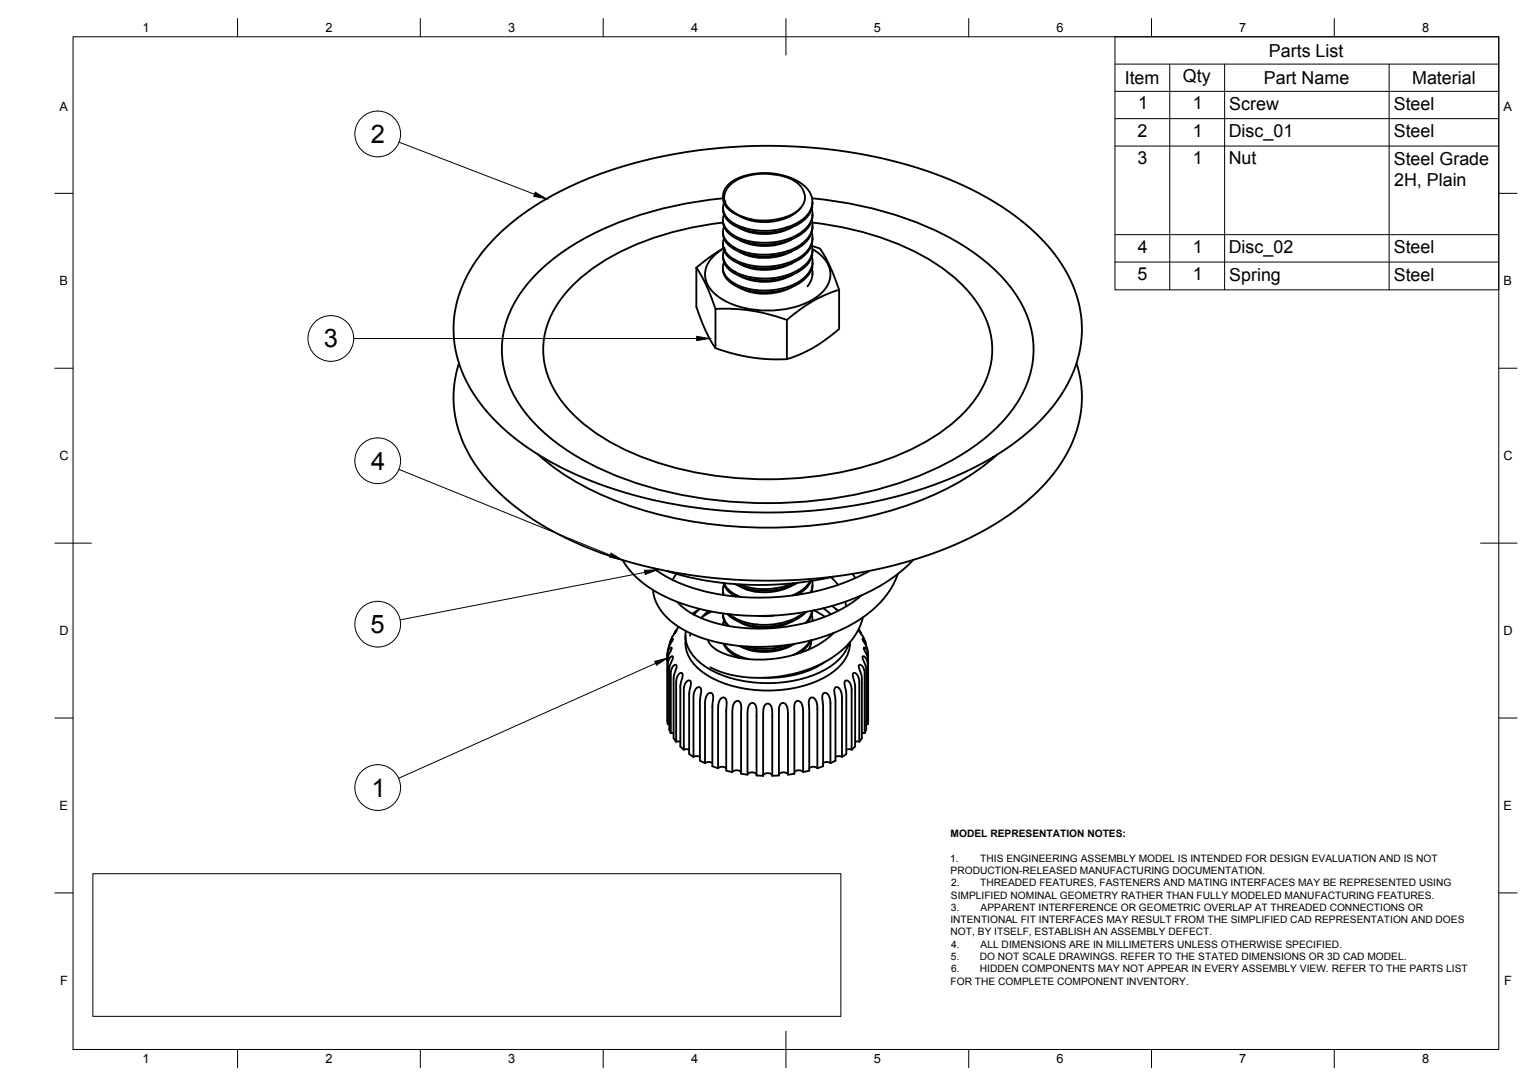
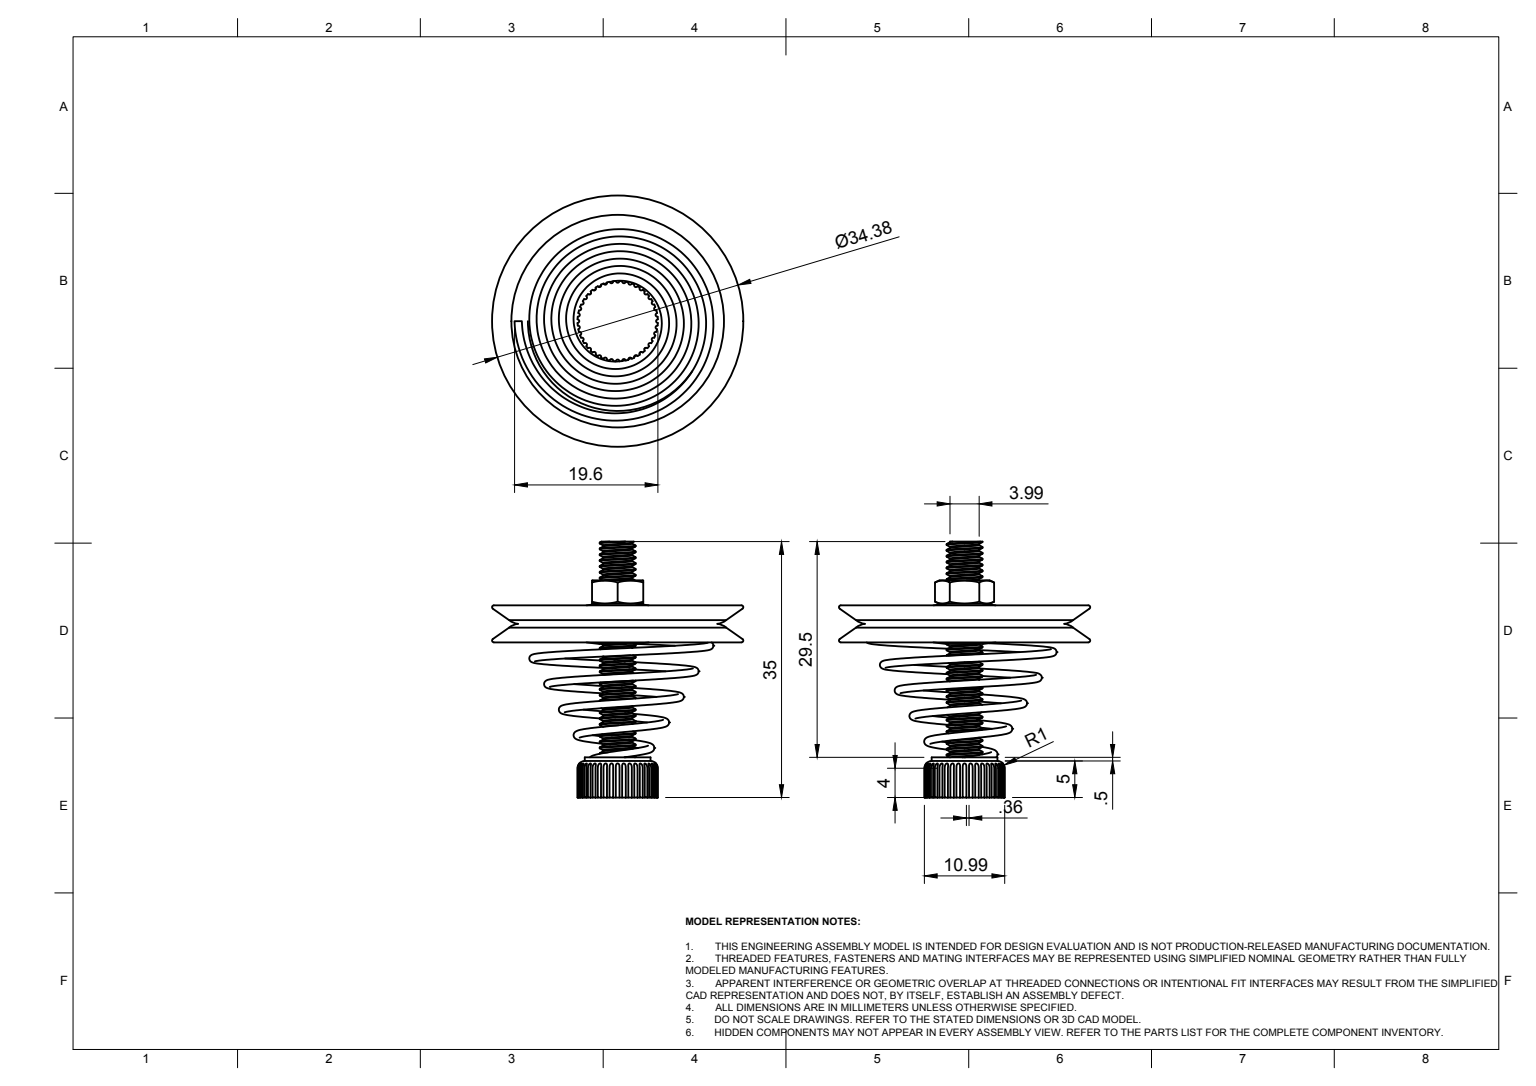
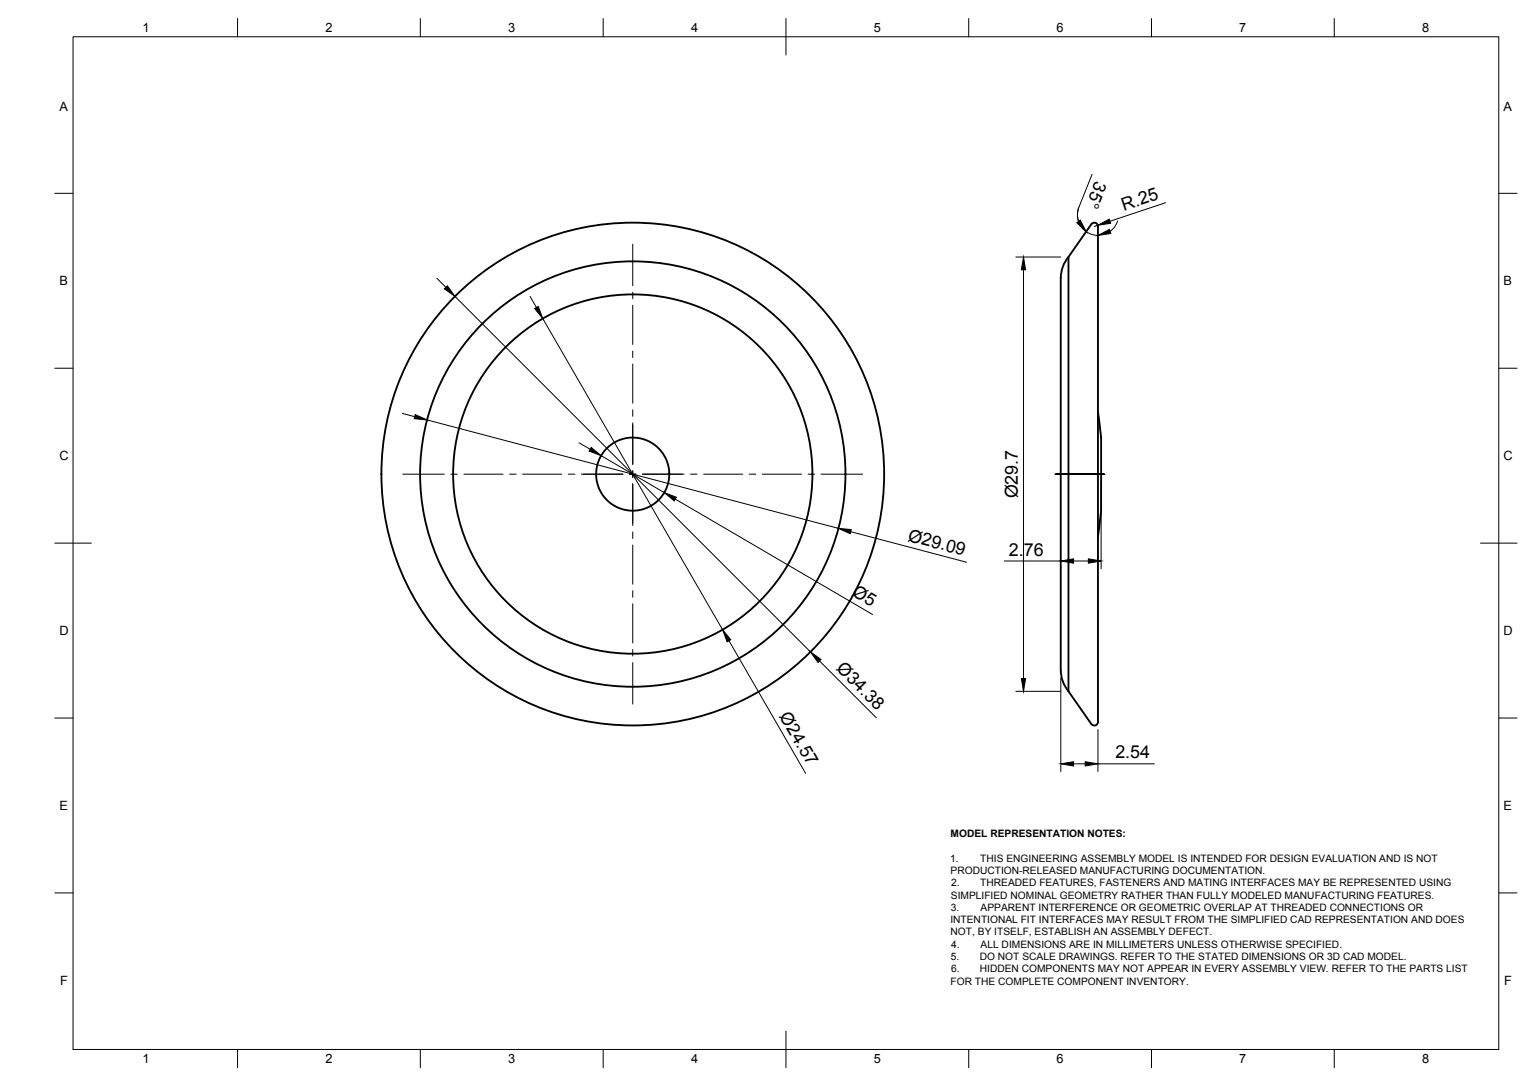
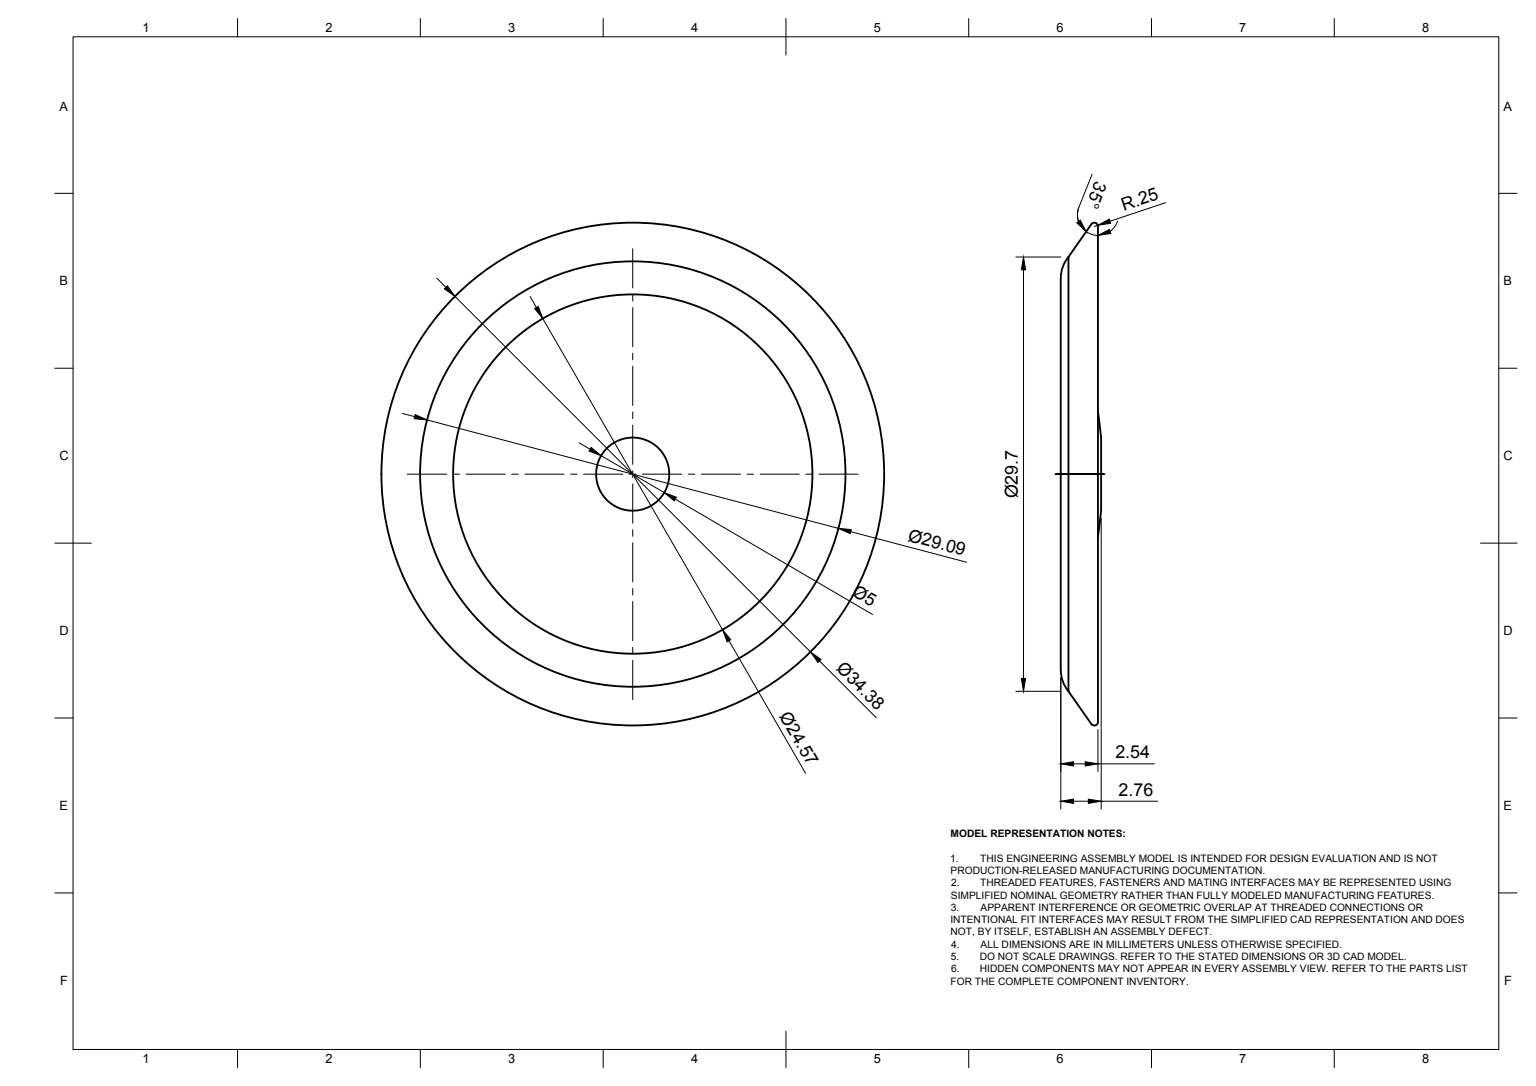
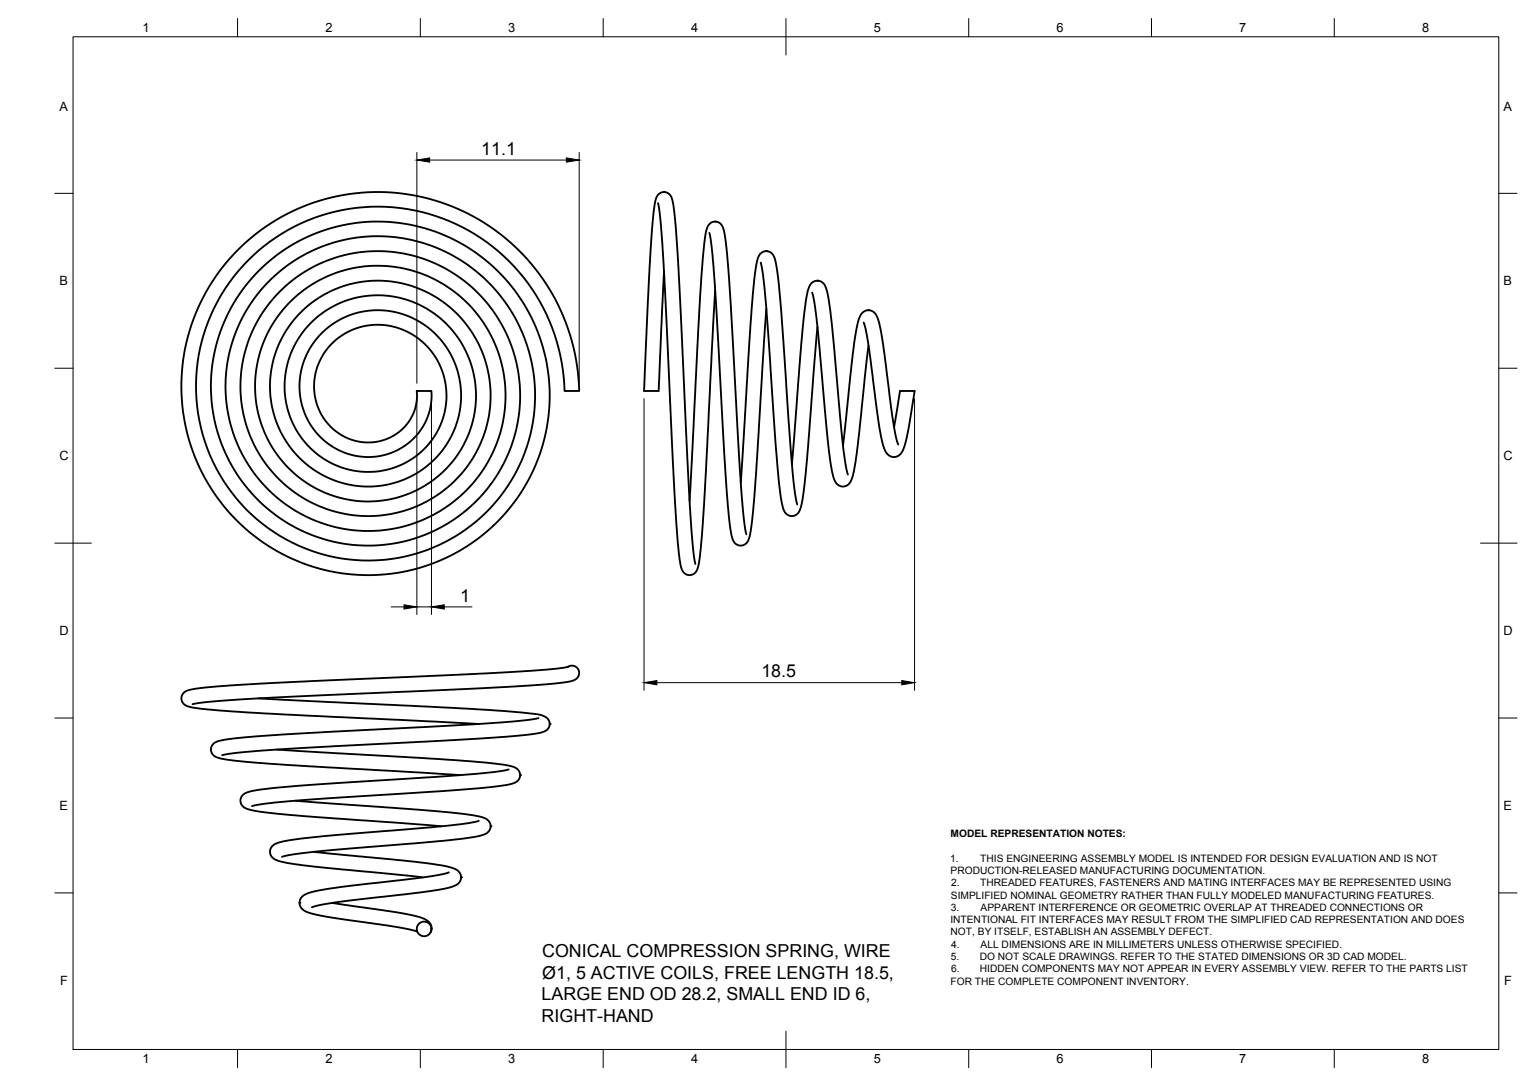
ISO-10303-21;
HEADER;
/* Generated by software containing ST-Developer
 * from STEP Tools, Inc. (www.steptools.com) 
 */

FILE_DESCRIPTION(
/* description */ (''),
/* implementation_level */ '2;1');

FILE_NAME(
/* name */ 'BR-106',
/* time_stamp */ '2026-10-04T16:36:43-07:00',
/* author */ (''),
/* organization */ (''),
/* preprocessor_version */ 'ST-DEVELOPER v20.2',
/* originating_system */ 'Autodesk Translation Framework v15.15.0.0',
/* authorisation */ '');

FILE_SCHEMA (('AUTOMOTIVE_DESIGN { 1 0 10303 214 3 1 1 }'));
ENDSEC;

DATA;
#10=MECHANICAL_DESIGN_GEOMETRIC_PRESENTATION_REPRESENTATION('',(#67,#68,
#69,#70,#71),#33474);
#11=ITEM_DEFINED_TRANSFORMATION($,$,#2869,#3144);
#12=ITEM_DEFINED_TRANSFORMATION($,$,#3089,#3145);
#13=ITEM_DEFINED_TRANSFORMATION($,$,#3107,#3146);
#14=ITEM_DEFINED_TRANSFORMATION($,$,#3125,#3147);
#15=ITEM_DEFINED_TRANSFORMATION($,$,#3128,#3148);
#16=(
REPRESENTATION_RELATIONSHIP($,$,#33497,#33496)
REPRESENTATION_RELATIONSHIP_WITH_TRANSFORMATION(#11)
SHAPE_REPRESENTATION_RELATIONSHIP()
);
#17=(
REPRESENTATION_RELATIONSHIP($,$,#33498,#33496)
REPRESENTATION_RELATIONSHIP_WITH_TRANSFORMATION(#12)
SHAPE_REPRESENTATION_RELATIONSHIP()
);
#18=(
REPRESENTATION_RELATIONSHIP($,$,#33499,#33496)
REPRESENTATION_RELATIONSHIP_WITH_TRANSFORMATION(#13)
SHAPE_REPRESENTATION_RELATIONSHIP()
);
#19=(
REPRESENTATION_RELATIONSHIP($,$,#33500,#33496)
REPRESENTATION_RELATIONSHIP_WITH_TRANSFORMATION(#14)
SHAPE_REPRESENTATION_RELATIONSHIP()
);
#20=(
REPRESENTATION_RELATIONSHIP($,$,#33501,#33496)
REPRESENTATION_RELATIONSHIP_WITH_TRANSFORMATION(#15)
SHAPE_REPRESENTATION_RELATIONSHIP()
);
#21=CONTEXT_DEPENDENT_SHAPE_REPRESENTATION(#16,#33491);
#22=CONTEXT_DEPENDENT_SHAPE_REPRESENTATION(#17,#33492);
#23=CONTEXT_DEPENDENT_SHAPE_REPRESENTATION(#18,#33493);
#24=CONTEXT_DEPENDENT_SHAPE_REPRESENTATION(#19,#33494);
#25=CONTEXT_DEPENDENT_SHAPE_REPRESENTATION(#20,#33495);
#26=NEXT_ASSEMBLY_USAGE_OCCURRENCE('Screw:1','Screw:1','Screw:1',#33503,
#33504,'Screw:1');
#27=NEXT_ASSEMBLY_USAGE_OCCURRENCE('Disc_01:1','Disc_01:1','Disc_01:1',
#33503,#33505,'Disc_01:1');
#28=NEXT_ASSEMBLY_USAGE_OCCURRENCE('Disc_02:1','Disc_02:1','Disc_02:1',
#33503,#33506,'Disc_02:1');
#29=NEXT_ASSEMBLY_USAGE_OCCURRENCE('Spring:1','Spring:1','Spring:1',#33503,
#33507,'Spring:1');
#30=NEXT_ASSEMBLY_USAGE_OCCURRENCE('Nut:1','Nut:1','Nut:1',#33503,#33508,
'Nut:1');
#31=(
BOUNDED_CURVE()
B_SPLINE_CURVE(5,(#31814,#31815,#31816,#31817,#31818,#31819,#31820,#31821,
#31822,#31823,#31824,#31825,#31826,#31827,#31828,#31829,#31830,#31831,#31832,
#31833,#31834,#31835,#31836,#31837,#31838),.UNSPECIFIED.,.F.,.F.)
B_SPLINE_CURVE_WITH_KNOTS((6,5,1,1,1,1,1,1,1,1,1,1,1,1,1,1,6),(-0.120132019601874,
0.,0.0666666666666667,0.133333333333333,0.2,0.266666666666667,0.333333333333333,
0.4,0.466666666666667,0.533333333333333,0.6,0.666666666666667,0.733333333333333,
0.8,0.866666666666667,0.933333333333333,1.),.UNSPECIFIED.)
CURVE()
GEOMETRIC_REPRESENTATION_ITEM()
RATIONAL_B_SPLINE_CURVE((1.,1.,1.,1.,1.,1.,1.,1.,1.,1.,1.,1.,1.,1.,1.,1.,
1.,1.,1.,1.,1.,1.,1.,1.,1.))
REPRESENTATION_ITEM('')
);
#32=(
BOUNDED_CURVE()
B_SPLINE_CURVE(5,(#32307,#32308,#32309,#32310,#32311,#32312,#32313,#32314,
#32315,#32316,#32317,#32318,#32319,#32320,#32321,#32322,#32323,#32324,#32325,
#32326,#32327,#32328,#32329,#32330,#32331),.UNSPECIFIED.,.F.,.F.)
B_SPLINE_CURVE_WITH_KNOTS((6,5,1,1,1,1,1,1,1,1,1,1,1,1,1,1,6),(-0.120132019601874,
0.,0.0666666666666667,0.133333333333333,0.2,0.266666666666667,0.333333333333333,
0.4,0.466666666666667,0.533333333333333,0.6,0.666666666666667,0.733333333333333,
0.8,0.866666666666667,0.933333333333333,1.),.UNSPECIFIED.)
CURVE()
GEOMETRIC_REPRESENTATION_ITEM()
RATIONAL_B_SPLINE_CURVE((1.,1.,1.,1.,1.,1.,1.,1.,1.,1.,1.,1.,1.,1.,1.,1.,
1.,1.,1.,1.,1.,1.,1.,1.,1.))
REPRESENTATION_ITEM('')
);
#33=(
BOUNDED_CURVE()
B_SPLINE_CURVE(2,(#33377,#33378,#33379),.UNSPECIFIED.,.F.,.F.)
B_SPLINE_CURVE_WITH_KNOTS((3,3),(0.000182870967167632,0.407532766922341),
 .UNSPECIFIED.)
CURVE()
GEOMETRIC_REPRESENTATION_ITEM()
RATIONAL_B_SPLINE_CURVE((1.00013898062186,1.15486101937814,1.00013898062186))
REPRESENTATION_ITEM('')
);
#34=(
BOUNDED_CURVE()
B_SPLINE_CURVE(2,(#33382,#33383,#33384),.UNSPECIFIED.,.F.,.F.)
B_SPLINE_CURVE_WITH_KNOTS((3,3),(0.000182870967168132,0.407532766922342),
 .UNSPECIFIED.)
CURVE()
GEOMETRIC_REPRESENTATION_ITEM()
RATIONAL_B_SPLINE_CURVE((1.00013898062186,1.15486101937814,1.00013898062186))
REPRESENTATION_ITEM('')
);
#35=(
BOUNDED_CURVE()
B_SPLINE_CURVE(2,(#33387,#33388,#33389),.UNSPECIFIED.,.F.,.F.)
B_SPLINE_CURVE_WITH_KNOTS((3,3),(0.000182870967167337,0.407532766922341),
 .UNSPECIFIED.)
CURVE()
GEOMETRIC_REPRESENTATION_ITEM()
RATIONAL_B_SPLINE_CURVE((1.00013898062186,1.15486101937814,1.00013898062186))
REPRESENTATION_ITEM('')
);
#36=(
BOUNDED_CURVE()
B_SPLINE_CURVE(2,(#33392,#33393,#33394),.UNSPECIFIED.,.F.,.F.)
B_SPLINE_CURVE_WITH_KNOTS((3,3),(0.000182870967167613,0.407532766922341),
 .UNSPECIFIED.)
CURVE()
GEOMETRIC_REPRESENTATION_ITEM()
RATIONAL_B_SPLINE_CURVE((1.00013898062186,1.15486101937814,1.00013898062186))
REPRESENTATION_ITEM('')
);
#37=(
BOUNDED_CURVE()
B_SPLINE_CURVE(2,(#33401,#33402,#33403),.UNSPECIFIED.,.F.,.F.)
B_SPLINE_CURVE_WITH_KNOTS((3,3),(0.203857818944754,0.407532766922341),
 .UNSPECIFIED.)
CURVE()
GEOMETRIC_REPRESENTATION_ITEM()
RATIONAL_B_SPLINE_CURVE((1.0775,1.0775,1.00013898062186))
REPRESENTATION_ITEM('')
);
#38=(
BOUNDED_CURVE()
B_SPLINE_CURVE(2,(#33405,#33406,#33407),.UNSPECIFIED.,.F.,.F.)
B_SPLINE_CURVE_WITH_KNOTS((3,3),(0.000182870967167808,0.407532766922341),
 .UNSPECIFIED.)
CURVE()
GEOMETRIC_REPRESENTATION_ITEM()
RATIONAL_B_SPLINE_CURVE((1.00013898062186,1.15486101937814,1.00013898062186))
REPRESENTATION_ITEM('')
);
#39=(
BOUNDED_CURVE()
B_SPLINE_CURVE(2,(#33408,#33409,#33410),.UNSPECIFIED.,.F.,.F.)
B_SPLINE_CURVE_WITH_KNOTS((3,3),(0.000182870967168059,0.407532766922341),
 .UNSPECIFIED.)
CURVE()
GEOMETRIC_REPRESENTATION_ITEM()
RATIONAL_B_SPLINE_CURVE((1.00013898062186,1.15486101937814,1.00013898062186))
REPRESENTATION_ITEM('')
);
#40=(
BOUNDED_CURVE()
B_SPLINE_CURVE(2,(#33412,#33413,#33414),.UNSPECIFIED.,.F.,.F.)
B_SPLINE_CURVE_WITH_KNOTS((3,3),(0.000182870967167986,0.407532766922341),
 .UNSPECIFIED.)
CURVE()
GEOMETRIC_REPRESENTATION_ITEM()
RATIONAL_B_SPLINE_CURVE((1.00013898062186,1.15486101937814,1.00013898062186))
REPRESENTATION_ITEM('')
);
#41=(
BOUNDED_CURVE()
B_SPLINE_CURVE(2,(#33415,#33416,#33417),.UNSPECIFIED.,.F.,.F.)
B_SPLINE_CURVE_WITH_KNOTS((3,3),(0.000182870967167794,0.203857818944754),
 .UNSPECIFIED.)
CURVE()
GEOMETRIC_REPRESENTATION_ITEM()
RATIONAL_B_SPLINE_CURVE((1.00013898062186,1.0775,1.0775))
REPRESENTATION_ITEM('')
);
#42=(
BOUNDED_CURVE()
B_SPLINE_CURVE(2,(#33420,#33421,#33422),.UNSPECIFIED.,.F.,.F.)
B_SPLINE_CURVE_WITH_KNOTS((3,3),(0.000182870967168019,0.407532766922341),
 .UNSPECIFIED.)
CURVE()
GEOMETRIC_REPRESENTATION_ITEM()
RATIONAL_B_SPLINE_CURVE((1.00013898062186,1.15486101937814,1.00013898062186))
REPRESENTATION_ITEM('')
);
#43=(
BOUNDED_CURVE()
B_SPLINE_CURVE(2,(#33426,#33427,#33428),.UNSPECIFIED.,.F.,.F.)
B_SPLINE_CURVE_WITH_KNOTS((3,3),(0.203857818944755,0.407532766922341),
 .UNSPECIFIED.)
CURVE()
GEOMETRIC_REPRESENTATION_ITEM()
RATIONAL_B_SPLINE_CURVE((1.0775,1.0775,1.00013898062186))
REPRESENTATION_ITEM('')
);
#44=(
BOUNDED_CURVE()
B_SPLINE_CURVE(2,(#33430,#33431,#33432),.UNSPECIFIED.,.F.,.F.)
B_SPLINE_CURVE_WITH_KNOTS((3,3),(0.000182870967167917,0.203857818944755),
 .UNSPECIFIED.)
CURVE()
GEOMETRIC_REPRESENTATION_ITEM()
RATIONAL_B_SPLINE_CURVE((1.00013898062186,1.0775,1.0775))
REPRESENTATION_ITEM('')
);
#45=(
BOUNDED_CURVE()
B_SPLINE_CURVE(2,(#33436,#33437,#33438),.UNSPECIFIED.,.F.,.F.)
B_SPLINE_CURVE_WITH_KNOTS((3,3),(0.000182870967168095,0.407532766922342),
 .UNSPECIFIED.)
CURVE()
GEOMETRIC_REPRESENTATION_ITEM()
RATIONAL_B_SPLINE_CURVE((1.00013898062186,1.15486101937814,1.00013898062186))
REPRESENTATION_ITEM('')
);
#46=(
BOUNDED_CURVE()
B_SPLINE_CURVE(2,(#33441,#33442,#33443),.UNSPECIFIED.,.F.,.F.)
B_SPLINE_CURVE_WITH_KNOTS((3,3),(0.000182870967167807,0.407532766922341),
 .UNSPECIFIED.)
CURVE()
GEOMETRIC_REPRESENTATION_ITEM()
RATIONAL_B_SPLINE_CURVE((1.00013898062186,1.15486101937814,1.00013898062186))
REPRESENTATION_ITEM('')
);
#47=(
BOUNDED_SURFACE()
B_SPLINE_SURFACE(5,2,((#31588,#31589,#31590,#31591,#31592,#31593,#31594,
#31595,#31596),(#31597,#31598,#31599,#31600,#31601,#31602,#31603,#31604,
#31605),(#31606,#31607,#31608,#31609,#31610,#31611,#31612,#31613,#31614),
(#31615,#31616,#31617,#31618,#31619,#31620,#31621,#31622,#31623),(#31624,
#31625,#31626,#31627,#31628,#31629,#31630,#31631,#31632),(#31633,#31634,
#31635,#31636,#31637,#31638,#31639,#31640,#31641),(#31642,#31643,#31644,
#31645,#31646,#31647,#31648,#31649,#31650),(#31651,#31652,#31653,#31654,
#31655,#31656,#31657,#31658,#31659),(#31660,#31661,#31662,#31663,#31664,
#31665,#31666,#31667,#31668),(#31669,#31670,#31671,#31672,#31673,#31674,
#31675,#31676,#31677),(#31678,#31679,#31680,#31681,#31682,#31683,#31684,
#31685,#31686),(#31687,#31688,#31689,#31690,#31691,#31692,#31693,#31694,
#31695),(#31696,#31697,#31698,#31699,#31700,#31701,#31702,#31703,#31704),
(#31705,#31706,#31707,#31708,#31709,#31710,#31711,#31712,#31713),(#31714,
#31715,#31716,#31717,#31718,#31719,#31720,#31721,#31722),(#31723,#31724,
#31725,#31726,#31727,#31728,#31729,#31730,#31731),(#31732,#31733,#31734,
#31735,#31736,#31737,#31738,#31739,#31740),(#31741,#31742,#31743,#31744,
#31745,#31746,#31747,#31748,#31749),(#31750,#31751,#31752,#31753,#31754,
#31755,#31756,#31757,#31758),(#31759,#31760,#31761,#31762,#31763,#31764,
#31765,#31766,#31767),(#31768,#31769,#31770,#31771,#31772,#31773,#31774,
#31775,#31776),(#31777,#31778,#31779,#31780,#31781,#31782,#31783,#31784,
#31785),(#31786,#31787,#31788,#31789,#31790,#31791,#31792,#31793,#31794),
(#31795,#31796,#31797,#31798,#31799,#31800,#31801,#31802,#31803),(#31804,
#31805,#31806,#31807,#31808,#31809,#31810,#31811,#31812)),.UNSPECIFIED.,
 .F.,.T.,.F.)
B_SPLINE_SURFACE_WITH_KNOTS((6,5,1,1,1,1,1,1,1,1,1,1,1,1,1,1,6),(3,2,2,
2,3),(-0.300330049004687,0.,0.0666666666666667,0.133333333333333,0.2,0.266666666666667,
0.333333333333333,0.4,0.466666666666667,0.533333333333333,0.6,0.666666666666667,
0.733333333333333,0.8,0.866666666666667,0.933333333333333,1.),(0.,1.5707963267949,
3.14159265358979,4.71238898038469,6.28318530717959),.UNSPECIFIED.)
GEOMETRIC_REPRESENTATION_ITEM()
RATIONAL_B_SPLINE_SURFACE(((1.,0.707106781186548,1.,0.707106781186548,1.,
0.707106781186548,1.,0.707106781186548,1.),(1.,0.707106781186548,1.,0.707106781186548,
1.,0.707106781186548,1.,0.707106781186548,1.),(1.,0.707106781186548,1.,
0.707106781186548,1.,0.707106781186548,1.,0.707106781186548,1.),(1.,0.707106781186548,
1.,0.707106781186548,1.,0.707106781186548,1.,0.707106781186548,1.),(1.,
0.707106781186548,1.,0.707106781186548,1.,0.707106781186548,1.,0.707106781186548,
1.),(1.,0.707106781186548,1.,0.707106781186548,1.,0.707106781186548,1.,
0.707106781186548,1.),(1.,0.707106781186548,1.,0.707106781186548,1.,0.707106781186548,
1.,0.707106781186548,1.),(1.,0.707106781186548,1.,0.707106781186548,1.,
0.707106781186548,1.,0.707106781186548,1.),(1.,0.707106781186548,1.,0.707106781186548,
1.,0.707106781186548,1.,0.707106781186548,1.),(1.,0.707106781186548,1.,
0.707106781186548,1.,0.707106781186548,1.,0.707106781186548,1.),(1.,0.707106781186548,
1.,0.707106781186548,1.,0.707106781186548,1.,0.707106781186548,1.),(1.,
0.707106781186548,1.,0.707106781186548,1.,0.707106781186548,1.,0.707106781186548,
1.),(1.,0.707106781186548,1.,0.707106781186548,1.,0.707106781186548,1.,
0.707106781186548,1.),(1.,0.707106781186548,1.,0.707106781186548,1.,0.707106781186548,
1.,0.707106781186548,1.),(1.,0.707106781186548,1.,0.707106781186548,1.,
0.707106781186548,1.,0.707106781186548,1.),(1.,0.707106781186548,1.,0.707106781186548,
1.,0.707106781186548,1.,0.707106781186548,1.),(1.,0.707106781186548,1.,
0.707106781186548,1.,0.707106781186548,1.,0.707106781186548,1.),(1.,0.707106781186548,
1.,0.707106781186548,1.,0.707106781186548,1.,0.707106781186548,1.),(1.,
0.707106781186548,1.,0.707106781186548,1.,0.707106781186548,1.,0.707106781186548,
1.),(1.,0.707106781186548,1.,0.707106781186548,1.,0.707106781186548,1.,
0.707106781186548,1.),(1.,0.707106781186548,1.,0.707106781186548,1.,0.707106781186548,
1.,0.707106781186548,1.),(1.,0.707106781186548,1.,0.707106781186548,1.,
0.707106781186548,1.,0.707106781186548,1.),(1.,0.707106781186548,1.,0.707106781186548,
1.,0.707106781186548,1.,0.707106781186548,1.),(1.,0.707106781186548,1.,
0.707106781186548,1.,0.707106781186548,1.,0.707106781186548,1.),(1.,0.707106781186548,
1.,0.707106781186548,1.,0.707106781186548,1.,0.707106781186548,1.)))
REPRESENTATION_ITEM('')
SURFACE()
);
#48=(
BOUNDED_SURFACE()
B_SPLINE_SURFACE(3,2,((#31924,#31925,#31926,#31927,#31928,#31929,#31930,
#31931,#31932),(#31933,#31934,#31935,#31936,#31937,#31938,#31939,#31940,
#31941),(#31942,#31943,#31944,#31945,#31946,#31947,#31948,#31949,#31950),
(#31951,#31952,#31953,#31954,#31955,#31956,#31957,#31958,#31959),(#31960,
#31961,#31962,#31963,#31964,#31965,#31966,#31967,#31968),(#31969,#31970,
#31971,#31972,#31973,#31974,#31975,#31976,#31977),(#31978,#31979,#31980,
#31981,#31982,#31983,#31984,#31985,#31986),(#31987,#31988,#31989,#31990,
#31991,#31992,#31993,#31994,#31995),(#31996,#31997,#31998,#31999,#32000,
#32001,#32002,#32003,#32004),(#32005,#32006,#32007,#32008,#32009,#32010,
#32011,#32012,#32013),(#32014,#32015,#32016,#32017,#32018,#32019,#32020,
#32021,#32022),(#32023,#32024,#32025,#32026,#32027,#32028,#32029,#32030,
#32031),(#32032,#32033,#32034,#32035,#32036,#32037,#32038,#32039,#32040)),
 .UNSPECIFIED.,.F.,.T.,.F.)
B_SPLINE_SURFACE_WITH_KNOTS((4,3,3,3,4),(3,2,2,2,3),(-0.984123122879426,
-0.97309206569331,-0.499330519660681,-0.00706539599512239,0.2972933688639),
(0.,1.5707963267949,3.14159265358979,4.71238898038469,6.28318530717959),
 .UNSPECIFIED.)
GEOMETRIC_REPRESENTATION_ITEM()
RATIONAL_B_SPLINE_SURFACE(((1.,0.707106781186548,1.,0.707106781186548,1.,
0.707106781186548,1.,0.707106781186548,1.),(1.,0.707106781186548,1.,0.707106781186548,
1.,0.707106781186548,1.,0.707106781186548,1.),(1.,0.707106781186548,1.,
0.707106781186548,1.,0.707106781186548,1.,0.707106781186548,1.),(1.,0.707106781186548,
1.,0.707106781186548,1.,0.707106781186548,1.,0.707106781186548,1.),(1.,
0.707106781186548,1.,0.707106781186548,1.,0.707106781186548,1.,0.707106781186548,
1.),(1.,0.707106781186548,1.,0.707106781186548,1.,0.707106781186548,1.,
0.707106781186548,1.),(1.,0.707106781186548,1.,0.707106781186548,1.,0.707106781186548,
1.,0.707106781186548,1.),(1.,0.707106781186548,1.,0.707106781186548,1.,
0.707106781186548,1.,0.707106781186548,1.),(1.,0.707106781186548,1.,0.707106781186548,
1.,0.707106781186548,1.,0.707106781186548,1.),(1.,0.707106781186548,1.,
0.707106781186548,1.,0.707106781186548,1.,0.707106781186548,1.),(1.,0.707106781186548,
1.,0.707106781186548,1.,0.707106781186548,1.,0.707106781186548,1.),(1.,
0.707106781186548,1.,0.707106781186548,1.,0.707106781186548,1.,0.707106781186548,
1.),(1.,0.707106781186548,1.,0.707106781186548,1.,0.707106781186548,1.,
0.707106781186548,1.)))
REPRESENTATION_ITEM('')
SURFACE()
);
#49=(
BOUNDED_SURFACE()
B_SPLINE_SURFACE(5,2,((#32081,#32082,#32083,#32084,#32085,#32086,#32087,
#32088,#32089),(#32090,#32091,#32092,#32093,#32094,#32095,#32096,#32097,
#32098),(#32099,#32100,#32101,#32102,#32103,#32104,#32105,#32106,#32107),
(#32108,#32109,#32110,#32111,#32112,#32113,#32114,#32115,#32116),(#32117,
#32118,#32119,#32120,#32121,#32122,#32123,#32124,#32125),(#32126,#32127,
#32128,#32129,#32130,#32131,#32132,#32133,#32134),(#32135,#32136,#32137,
#32138,#32139,#32140,#32141,#32142,#32143),(#32144,#32145,#32146,#32147,
#32148,#32149,#32150,#32151,#32152),(#32153,#32154,#32155,#32156,#32157,
#32158,#32159,#32160,#32161),(#32162,#32163,#32164,#32165,#32166,#32167,
#32168,#32169,#32170),(#32171,#32172,#32173,#32174,#32175,#32176,#32177,
#32178,#32179),(#32180,#32181,#32182,#32183,#32184,#32185,#32186,#32187,
#32188),(#32189,#32190,#32191,#32192,#32193,#32194,#32195,#32196,#32197),
(#32198,#32199,#32200,#32201,#32202,#32203,#32204,#32205,#32206),(#32207,
#32208,#32209,#32210,#32211,#32212,#32213,#32214,#32215),(#32216,#32217,
#32218,#32219,#32220,#32221,#32222,#32223,#32224),(#32225,#32226,#32227,
#32228,#32229,#32230,#32231,#32232,#32233),(#32234,#32235,#32236,#32237,
#32238,#32239,#32240,#32241,#32242),(#32243,#32244,#32245,#32246,#32247,
#32248,#32249,#32250,#32251),(#32252,#32253,#32254,#32255,#32256,#32257,
#32258,#32259,#32260),(#32261,#32262,#32263,#32264,#32265,#32266,#32267,
#32268,#32269),(#32270,#32271,#32272,#32273,#32274,#32275,#32276,#32277,
#32278),(#32279,#32280,#32281,#32282,#32283,#32284,#32285,#32286,#32287),
(#32288,#32289,#32290,#32291,#32292,#32293,#32294,#32295,#32296),(#32297,
#32298,#32299,#32300,#32301,#32302,#32303,#32304,#32305)),.UNSPECIFIED.,
 .F.,.T.,.F.)
B_SPLINE_SURFACE_WITH_KNOTS((6,5,1,1,1,1,1,1,1,1,1,1,1,1,1,1,6),(3,2,2,
2,3),(-0.300330049004687,0.,0.0666666666666667,0.133333333333333,0.2,0.266666666666667,
0.333333333333333,0.4,0.466666666666667,0.533333333333333,0.6,0.666666666666667,
0.733333333333333,0.8,0.866666666666667,0.933333333333333,1.),(0.,1.5707963267949,
3.14159265358979,4.71238898038469,6.28318530717959),.UNSPECIFIED.)
GEOMETRIC_REPRESENTATION_ITEM()
RATIONAL_B_SPLINE_SURFACE(((1.,0.707106781186548,1.,0.707106781186548,1.,
0.707106781186548,1.,0.707106781186548,1.),(1.,0.707106781186548,1.,0.707106781186548,
1.,0.707106781186548,1.,0.707106781186548,1.),(1.,0.707106781186548,1.,
0.707106781186548,1.,0.707106781186548,1.,0.707106781186548,1.),(1.,0.707106781186548,
1.,0.707106781186548,1.,0.707106781186548,1.,0.707106781186548,1.),(1.,
0.707106781186548,1.,0.707106781186548,1.,0.707106781186548,1.,0.707106781186548,
1.),(1.,0.707106781186548,1.,0.707106781186548,1.,0.707106781186548,1.,
0.707106781186548,1.),(1.,0.707106781186548,1.,0.707106781186548,1.,0.707106781186548,
1.,0.707106781186548,1.),(1.,0.707106781186548,1.,0.707106781186548,1.,
0.707106781186548,1.,0.707106781186548,1.),(1.,0.707106781186548,1.,0.707106781186548,
1.,0.707106781186548,1.,0.707106781186548,1.),(1.,0.707106781186548,1.,
0.707106781186548,1.,0.707106781186548,1.,0.707106781186548,1.),(1.,0.707106781186548,
1.,0.707106781186548,1.,0.707106781186548,1.,0.707106781186548,1.),(1.,
0.707106781186548,1.,0.707106781186548,1.,0.707106781186548,1.,0.707106781186548,
1.),(1.,0.707106781186548,1.,0.707106781186548,1.,0.707106781186548,1.,
0.707106781186548,1.),(1.,0.707106781186548,1.,0.707106781186548,1.,0.707106781186548,
1.,0.707106781186548,1.),(1.,0.707106781186548,1.,0.707106781186548,1.,
0.707106781186548,1.,0.707106781186548,1.),(1.,0.707106781186548,1.,0.707106781186548,
1.,0.707106781186548,1.,0.707106781186548,1.),(1.,0.707106781186548,1.,
0.707106781186548,1.,0.707106781186548,1.,0.707106781186548,1.),(1.,0.707106781186548,
1.,0.707106781186548,1.,0.707106781186548,1.,0.707106781186548,1.),(1.,
0.707106781186548,1.,0.707106781186548,1.,0.707106781186548,1.,0.707106781186548,
1.),(1.,0.707106781186548,1.,0.707106781186548,1.,0.707106781186548,1.,
0.707106781186548,1.),(1.,0.707106781186548,1.,0.707106781186548,1.,0.707106781186548,
1.,0.707106781186548,1.),(1.,0.707106781186548,1.,0.707106781186548,1.,
0.707106781186548,1.,0.707106781186548,1.),(1.,0.707106781186548,1.,0.707106781186548,
1.,0.707106781186548,1.,0.707106781186548,1.),(1.,0.707106781186548,1.,
0.707106781186548,1.,0.707106781186548,1.,0.707106781186548,1.),(1.,0.707106781186548,
1.,0.707106781186548,1.,0.707106781186548,1.,0.707106781186548,1.)))
REPRESENTATION_ITEM('')
SURFACE()
);
#50=(
BOUNDED_SURFACE()
B_SPLINE_SURFACE(3,2,((#32417,#32418,#32419,#32420,#32421,#32422,#32423,
#32424,#32425),(#32426,#32427,#32428,#32429,#32430,#32431,#32432,#32433,
#32434),(#32435,#32436,#32437,#32438,#32439,#32440,#32441,#32442,#32443),
(#32444,#32445,#32446,#32447,#32448,#32449,#32450,#32451,#32452),(#32453,
#32454,#32455,#32456,#32457,#32458,#32459,#32460,#32461),(#32462,#32463,
#32464,#32465,#32466,#32467,#32468,#32469,#32470),(#32471,#32472,#32473,
#32474,#32475,#32476,#32477,#32478,#32479),(#32480,#32481,#32482,#32483,
#32484,#32485,#32486,#32487,#32488),(#32489,#32490,#32491,#32492,#32493,
#32494,#32495,#32496,#32497),(#32498,#32499,#32500,#32501,#32502,#32503,
#32504,#32505,#32506),(#32507,#32508,#32509,#32510,#32511,#32512,#32513,
#32514,#32515),(#32516,#32517,#32518,#32519,#32520,#32521,#32522,#32523,
#32524),(#32525,#32526,#32527,#32528,#32529,#32530,#32531,#32532,#32533)),
 .UNSPECIFIED.,.F.,.T.,.F.)
B_SPLINE_SURFACE_WITH_KNOTS((4,3,3,3,4),(3,2,2,2,3),(-0.984123122879426,
-0.97309206569331,-0.499330519660681,-0.00706539599512239,0.297293368863902),
(0.,1.5707963267949,3.14159265358979,4.71238898038469,6.28318530717959),
 .UNSPECIFIED.)
GEOMETRIC_REPRESENTATION_ITEM()
RATIONAL_B_SPLINE_SURFACE(((1.,0.707106781186548,1.,0.707106781186548,1.,
0.707106781186548,1.,0.707106781186548,1.),(1.,0.707106781186548,1.,0.707106781186548,
1.,0.707106781186548,1.,0.707106781186548,1.),(1.,0.707106781186548,1.,
0.707106781186548,1.,0.707106781186548,1.,0.707106781186548,1.),(1.,0.707106781186548,
1.,0.707106781186548,1.,0.707106781186548,1.,0.707106781186548,1.),(1.,
0.707106781186548,1.,0.707106781186548,1.,0.707106781186548,1.,0.707106781186548,
1.),(1.,0.707106781186548,1.,0.707106781186548,1.,0.707106781186548,1.,
0.707106781186548,1.),(1.,0.707106781186548,1.,0.707106781186548,1.,0.707106781186548,
1.,0.707106781186548,1.),(1.,0.707106781186548,1.,0.707106781186548,1.,
0.707106781186548,1.,0.707106781186548,1.),(1.,0.707106781186548,1.,0.707106781186548,
1.,0.707106781186548,1.,0.707106781186548,1.),(1.,0.707106781186548,1.,
0.707106781186548,1.,0.707106781186548,1.,0.707106781186548,1.),(1.,0.707106781186548,
1.,0.707106781186548,1.,0.707106781186548,1.,0.707106781186548,1.),(1.,
0.707106781186548,1.,0.707106781186548,1.,0.707106781186548,1.,0.707106781186548,
1.),(1.,0.707106781186548,1.,0.707106781186548,1.,0.707106781186548,1.,
0.707106781186548,1.)))
REPRESENTATION_ITEM('')
SURFACE()
);
#51=CONICAL_SURFACE('',#3090,16.067990296595,0.959931088596882);
#52=CONICAL_SURFACE('',#3096,15.7712719335665,0.959931088596882);
#53=CONICAL_SURFACE('',#3108,16.067990296595,0.959931088596882);
#54=CONICAL_SURFACE('',#3114,15.7712719335665,0.959931088596882);
#55=CONICAL_SURFACE('',#3131,3.73625,1.13446401379631);
#56=CONICAL_SURFACE('',#3140,3.73625,1.13446401379632);
#57=SHAPE_REPRESENTATION_RELATIONSHIP('SRR','None',#33497,#62);
#58=SHAPE_REPRESENTATION_RELATIONSHIP('SRR','None',#33498,#63);
#59=SHAPE_REPRESENTATION_RELATIONSHIP('SRR','None',#33499,#64);
#60=SHAPE_REPRESENTATION_RELATIONSHIP('SRR','None',#33500,#65);
#61=SHAPE_REPRESENTATION_RELATIONSHIP('SRR','None',#33501,#66);
#62=ADVANCED_BREP_SHAPE_REPRESENTATION('',(#72),#33469);
#63=ADVANCED_BREP_SHAPE_REPRESENTATION('',(#73),#33470);
#64=ADVANCED_BREP_SHAPE_REPRESENTATION('',(#74),#33471);
#65=ADVANCED_BREP_SHAPE_REPRESENTATION('',(#75),#33472);
#66=ADVANCED_BREP_SHAPE_REPRESENTATION('',(#76),#33473);
#67=STYLED_ITEM('',(#33531),#72);
#68=STYLED_ITEM('',(#33531),#73);
#69=STYLED_ITEM('',(#33531),#74);
#70=STYLED_ITEM('',(#33531),#75);
#71=STYLED_ITEM('',(#33530),#76);
#72=MANIFOLD_SOLID_BREP('Body1',#2807);
#73=MANIFOLD_SOLID_BREP('Body1',#2808);
#74=MANIFOLD_SOLID_BREP('Body1',#2809);
#75=MANIFOLD_SOLID_BREP('Body1',#2810);
#76=MANIFOLD_SOLID_BREP('Body1',#2811);
#77=TOROIDAL_SURFACE('',#3082,4.5,1.);
#78=TOROIDAL_SURFACE('',#3093,16.9386060980155,0.25);
#79=TOROIDAL_SURFACE('',#3098,13.4131653526691,1.72390117308562);
#80=TOROIDAL_SURFACE('',#3105,13.4131653526691,2.22390117308562);
#81=TOROIDAL_SURFACE('',#3111,16.9386060980155,0.25);
#82=TOROIDAL_SURFACE('',#3116,13.4131653526691,1.72390117308562);
#83=TOROIDAL_SURFACE('',#3123,13.4131653526691,2.22390117308562);
#84=B_SPLINE_SURFACE_WITH_KNOTS('',3,3,((#27469,#27470,#27471,#27472,#27473,
#27474,#27475,#27476,#27477,#27478,#27479,#27480,#27481,#27482,#27483,#27484,
#27485,#27486,#27487,#27488,#27489,#27490,#27491,#27492,#27493,#27494,#27495,
#27496,#27497,#27498,#27499,#27500,#27501,#27502,#27503,#27504,#27505,#27506,
#27507,#27508,#27509,#27510,#27511,#27512,#27513,#27514,#27515,#27516,#27517,
#27518,#27519,#27520,#27521,#27522,#27523,#27524,#27525,#27526,#27527,#27528,
#27529,#27530,#27531,#27532,#27533,#27534,#27535,#27536,#27537,#27538,#27539,
#27540,#27541,#27542,#27543,#27544,#27545,#27546,#27547,#27548,#27549,#27550,
#27551,#27552,#27553,#27554,#27555,#27556,#27557,#27558,#27559,#27560,#27561,
#27562,#27563,#27564,#27565,#27566,#27567,#27568,#27569,#27570,#27571,#27572,
#27573,#27574,#27575,#27576,#27577,#27578,#27579,#27580,#27581,#27582,#27583,
#27584,#27585,#27586,#27587,#27588,#27589,#27590,#27591,#27592,#27593,#27594,
#27595,#27596,#27597,#27598,#27599,#27600,#27601,#27602,#27603,#27604,#27605,
#27606,#27607,#27608,#27609,#27610,#27611,#27612,#27613,#27614,#27615,#27616,
#27617,#27618,#27619,#27620,#27621,#27622,#27623,#27624,#27625,#27626,#27627,
#27628,#27629,#27630,#27631,#27632,#27633,#27634,#27635,#27636,#27637,#27638,
#27639,#27640,#27641,#27642,#27643,#27644,#27645,#27646,#27647,#27648,#27649,
#27650,#27651,#27652,#27653,#27654,#27655,#27656,#27657,#27658,#27659,#27660,
#27661,#27662,#27663,#27664,#27665,#27666,#27667,#27668,#27669,#27670,#27671,
#27672,#27673,#27674,#27675,#27676,#27677,#27678,#27679,#27680,#27681,#27682,
#27683,#27684,#27685,#27686,#27687,#27688,#27689,#27690,#27691,#27692,#27693,
#27694,#27695,#27696,#27697,#27698,#27699,#27700,#27701,#27702,#27703,#27704,
#27705,#27706,#27707,#27708,#27709),(#27710,#27711,#27712,#27713,#27714,
#27715,#27716,#27717,#27718,#27719,#27720,#27721,#27722,#27723,#27724,#27725,
#27726,#27727,#27728,#27729,#27730,#27731,#27732,#27733,#27734,#27735,#27736,
#27737,#27738,#27739,#27740,#27741,#27742,#27743,#27744,#27745,#27746,#27747,
#27748,#27749,#27750,#27751,#27752,#27753,#27754,#27755,#27756,#27757,#27758,
#27759,#27760,#27761,#27762,#27763,#27764,#27765,#27766,#27767,#27768,#27769,
#27770,#27771,#27772,#27773,#27774,#27775,#27776,#27777,#27778,#27779,#27780,
#27781,#27782,#27783,#27784,#27785,#27786,#27787,#27788,#27789,#27790,#27791,
#27792,#27793,#27794,#27795,#27796,#27797,#27798,#27799,#27800,#27801,#27802,
#27803,#27804,#27805,#27806,#27807,#27808,#27809,#27810,#27811,#27812,#27813,
#27814,#27815,#27816,#27817,#27818,#27819,#27820,#27821,#27822,#27823,#27824,
#27825,#27826,#27827,#27828,#27829,#27830,#27831,#27832,#27833,#27834,#27835,
#27836,#27837,#27838,#27839,#27840,#27841,#27842,#27843,#27844,#27845,#27846,
#27847,#27848,#27849,#27850,#27851,#27852,#27853,#27854,#27855,#27856,#27857,
#27858,#27859,#27860,#27861,#27862,#27863,#27864,#27865,#27866,#27867,#27868,
#27869,#27870,#27871,#27872,#27873,#27874,#27875,#27876,#27877,#27878,#27879,
#27880,#27881,#27882,#27883,#27884,#27885,#27886,#27887,#27888,#27889,#27890,
#27891,#27892,#27893,#27894,#27895,#27896,#27897,#27898,#27899,#27900,#27901,
#27902,#27903,#27904,#27905,#27906,#27907,#27908,#27909,#27910,#27911,#27912,
#27913,#27914,#27915,#27916,#27917,#27918,#27919,#27920,#27921,#27922,#27923,
#27924,#27925,#27926,#27927,#27928,#27929,#27930,#27931,#27932,#27933,#27934,
#27935,#27936,#27937,#27938,#27939,#27940,#27941,#27942,#27943,#27944,#27945,
#27946,#27947,#27948,#27949,#27950),(#27951,#27952,#27953,#27954,#27955,
#27956,#27957,#27958,#27959,#27960,#27961,#27962,#27963,#27964,#27965,#27966,
#27967,#27968,#27969,#27970,#27971,#27972,#27973,#27974,#27975,#27976,#27977,
#27978,#27979,#27980,#27981,#27982,#27983,#27984,#27985,#27986,#27987,#27988,
#27989,#27990,#27991,#27992,#27993,#27994,#27995,#27996,#27997,#27998,#27999,
#28000,#28001,#28002,#28003,#28004,#28005,#28006,#28007,#28008,#28009,#28010,
#28011,#28012,#28013,#28014,#28015,#28016,#28017,#28018,#28019,#28020,#28021,
#28022,#28023,#28024,#28025,#28026,#28027,#28028,#28029,#28030,#28031,#28032,
#28033,#28034,#28035,#28036,#28037,#28038,#28039,#28040,#28041,#28042,#28043,
#28044,#28045,#28046,#28047,#28048,#28049,#28050,#28051,#28052,#28053,#28054,
#28055,#28056,#28057,#28058,#28059,#28060,#28061,#28062,#28063,#28064,#28065,
#28066,#28067,#28068,#28069,#28070,#28071,#28072,#28073,#28074,#28075,#28076,
#28077,#28078,#28079,#28080,#28081,#28082,#28083,#28084,#28085,#28086,#28087,
#28088,#28089,#28090,#28091,#28092,#28093,#28094,#28095,#28096,#28097,#28098,
#28099,#28100,#28101,#28102,#28103,#28104,#28105,#28106,#28107,#28108,#28109,
#28110,#28111,#28112,#28113,#28114,#28115,#28116,#28117,#28118,#28119,#28120,
#28121,#28122,#28123,#28124,#28125,#28126,#28127,#28128,#28129,#28130,#28131,
#28132,#28133,#28134,#28135,#28136,#28137,#28138,#28139,#28140,#28141,#28142,
#28143,#28144,#28145,#28146,#28147,#28148,#28149,#28150,#28151,#28152,#28153,
#28154,#28155,#28156,#28157,#28158,#28159,#28160,#28161,#28162,#28163,#28164,
#28165,#28166,#28167,#28168,#28169,#28170,#28171,#28172,#28173,#28174,#28175,
#28176,#28177,#28178,#28179,#28180,#28181,#28182,#28183,#28184,#28185,#28186,
#28187,#28188,#28189,#28190,#28191),(#28192,#28193,#28194,#28195,#28196,
#28197,#28198,#28199,#28200,#28201,#28202,#28203,#28204,#28205,#28206,#28207,
#28208,#28209,#28210,#28211,#28212,#28213,#28214,#28215,#28216,#28217,#28218,
#28219,#28220,#28221,#28222,#28223,#28224,#28225,#28226,#28227,#28228,#28229,
#28230,#28231,#28232,#28233,#28234,#28235,#28236,#28237,#28238,#28239,#28240,
#28241,#28242,#28243,#28244,#28245,#28246,#28247,#28248,#28249,#28250,#28251,
#28252,#28253,#28254,#28255,#28256,#28257,#28258,#28259,#28260,#28261,#28262,
#28263,#28264,#28265,#28266,#28267,#28268,#28269,#28270,#28271,#28272,#28273,
#28274,#28275,#28276,#28277,#28278,#28279,#28280,#28281,#28282,#28283,#28284,
#28285,#28286,#28287,#28288,#28289,#28290,#28291,#28292,#28293,#28294,#28295,
#28296,#28297,#28298,#28299,#28300,#28301,#28302,#28303,#28304,#28305,#28306,
#28307,#28308,#28309,#28310,#28311,#28312,#28313,#28314,#28315,#28316,#28317,
#28318,#28319,#28320,#28321,#28322,#28323,#28324,#28325,#28326,#28327,#28328,
#28329,#28330,#28331,#28332,#28333,#28334,#28335,#28336,#28337,#28338,#28339,
#28340,#28341,#28342,#28343,#28344,#28345,#28346,#28347,#28348,#28349,#28350,
#28351,#28352,#28353,#28354,#28355,#28356,#28357,#28358,#28359,#28360,#28361,
#28362,#28363,#28364,#28365,#28366,#28367,#28368,#28369,#28370,#28371,#28372,
#28373,#28374,#28375,#28376,#28377,#28378,#28379,#28380,#28381,#28382,#28383,
#28384,#28385,#28386,#28387,#28388,#28389,#28390,#28391,#28392,#28393,#28394,
#28395,#28396,#28397,#28398,#28399,#28400,#28401,#28402,#28403,#28404,#28405,
#28406,#28407,#28408,#28409,#28410,#28411,#28412,#28413,#28414,#28415,#28416,
#28417,#28418,#28419,#28420,#28421,#28422,#28423,#28424,#28425,#28426,#28427,
#28428,#28429,#28430,#28431,#28432)),.UNSPECIFIED.,.F.,.F.,.F.,(4,4),(4,
1,1,1,1,1,1,1,1,1,1,1,1,1,1,1,1,1,1,1,1,1,1,1,1,1,1,1,1,1,1,1,1,1,1,1,1,
1,1,1,1,1,1,1,1,1,1,1,1,1,1,1,1,1,1,1,1,1,1,1,1,1,1,1,1,1,1,1,1,1,1,1,1,
1,1,1,1,1,1,1,1,1,1,1,1,1,1,1,1,1,1,1,1,1,1,1,1,1,1,1,1,1,1,1,1,1,1,1,1,
1,1,1,1,1,1,1,1,1,1,1,1,1,1,1,1,1,1,1,1,1,1,1,1,1,1,1,1,1,1,1,1,1,1,1,1,
1,1,1,1,1,1,1,1,1,1,1,1,1,1,1,1,1,1,1,1,1,1,1,1,1,1,1,1,1,1,1,1,1,1,1,1,
1,1,1,1,1,1,1,1,1,1,1,1,1,1,1,1,1,1,1,1,1,1,1,1,1,1,1,1,1,1,1,1,1,1,1,1,
1,1,1,1,1,1,1,1,1,1,1,1,1,1,1,1,1,1,1,1,1,4),(-0.000412226121642421,0.0529946871768046),
(8.30797483681352,9.30683859552365,10.3055194638844,11.3042003322452,12.3028812006059,
13.3015620689667,14.3002429373274,15.2989238056882,16.2976046740489,17.2962855424097,
18.2949664107704,19.2936472791312,20.2923281474919,21.2910090158527,22.2896898842134,
23.2883707525742,24.2870516209349,25.2857324892957,26.2844133576564,27.2830942260172,
28.2817750943779,29.2804559627387,30.2791368310994,31.2778176994602,32.2764985678209,
33.2751794361817,34.2738603045424,35.2725411729032,36.2712220412639,37.2699029096247,
38.2685837779855,39.2672646463462,40.265945514707,41.2646263830677,42.2633072514285,
43.2619881197892,44.26066898815,45.2593498565107,46.2580307248715,47.2567115932322,
48.255392461593,49.2540733299537,50.2527541983145,51.2514350666752,52.250115935036,
53.2487968033967,54.2474776717575,55.2461585401182,56.244839408479,57.2435202768397,
58.2422011452005,59.2408820135612,60.239562881922,61.2382437502827,62.2369246186435,
63.2356054870042,64.234286355365,65.2329672237257,66.2316480920865,67.2303289604472,
68.229009828808,69.2276906971688,70.2263715655295,71.2250524338903,72.223733302251,
73.2224141706118,74.2210950389725,75.2197759073333,76.218456775694,77.2171376440548,
78.2158185124155,79.2144993807763,80.213180249137,81.2118611174978,82.2105419858585,
83.2092228542193,84.20790372258,85.2065845909408,86.2052654593015,87.2039463276623,
88.202627196023,89.2013080643838,90.1999889327445,91.1986698011053,92.197350669466,
93.1960315378268,94.1947124061875,95.1933932745483,96.192074142909,97.1907550112698,
98.1894358796306,99.1881167479913,100.186797616352,101.185478484713,102.184159353074,
103.182840221434,104.181521089795,105.180201958156,106.178882826517,107.177563694877,
108.176244563238,109.174925431599,110.17360629996,111.17228716832,112.170968036681,
113.169648905042,114.168329773403,115.167010641763,116.165691510124,117.164372378485,
118.163053246846,119.161734115206,120.160414983567,121.159095851928,122.157776720289,
123.156457588649,124.15513845701,125.153819325371,126.152500193732,127.151181062092,
128.149861930453,129.148542798814,130.147223667175,131.145904535535,132.144585403896,
133.143266272257,134.141947140618,135.140628008978,136.139308877339,137.1379897457,
138.136670614061,139.135351482421,140.134032350782,141.132713219143,142.131394087504,
143.130074955864,144.128755824225,145.127436692586,146.126117560947,147.124798429307,
148.123479297668,149.122160166029,150.12084103439,151.11952190275,152.118202771111,
153.116883639472,154.115564507833,155.114245376193,156.112926244554,157.111607112915,
158.110287981276,159.108968849636,160.107649717997,161.106330586358,162.105011454719,
163.103692323079,164.10237319144,165.101054059801,166.099734928162,167.098415796522,
168.097096664883,169.095777533244,170.094458401605,171.093139269965,172.091820138326,
173.090501006687,174.089181875048,175.087862743408,176.086543611769,177.08522448013,
178.083905348491,179.082586216851,180.081267085212,181.079947953573,182.078628821934,
183.077309690294,184.075990558655,185.074671427016,186.073352295377,187.072033163737,
188.070714032098,189.069394900459,190.06807576882,191.06675663718,192.065437505541,
193.064118373902,194.062799242263,195.061480110623,196.060160978984,197.058841847345,
198.057522715706,199.056203584066,200.054884452427,201.053565320788,202.052246189149,
203.050927057509,204.04960792587,205.048288794231,206.046969662592,207.045650530952,
208.044331399313,209.043012267674,210.041693136035,211.040374004395,212.039054872756,
213.037735741117,214.036416609478,215.035097477838,216.033778346199,217.03245921456,
218.031140082921,219.029820951281,220.028501819642,221.027182688003,222.025863556364,
223.024544424724,224.023225293085,225.021906161446,226.020587029807,227.019267898167,
228.017948766528,229.016629634889,230.01531050325,231.01399137161,232.012672239971,
233.011353108332,234.010033976693,235.008714845054,236.007395713414,237.006076581775,
238.004757450136,239.003438318497,240.002119186857,241.000800055218,241.999480923579,
242.99816179194,243.9968426603,244.995523528661,245.994616623144),
 .UNSPECIFIED.);
#85=B_SPLINE_SURFACE_WITH_KNOTS('',3,3,((#28611,#28612,#28613,#28614,#28615,
#28616,#28617,#28618,#28619,#28620,#28621,#28622,#28623,#28624,#28625,#28626,
#28627,#28628,#28629,#28630,#28631,#28632,#28633,#28634,#28635,#28636,#28637,
#28638,#28639,#28640,#28641,#28642,#28643,#28644,#28645,#28646,#28647,#28648,
#28649,#28650,#28651,#28652,#28653,#28654,#28655,#28656,#28657,#28658,#28659,
#28660,#28661,#28662,#28663,#28664,#28665,#28666,#28667,#28668,#28669,#28670,
#28671,#28672,#28673,#28674,#28675,#28676,#28677,#28678,#28679,#28680,#28681,
#28682,#28683,#28684,#28685,#28686,#28687,#28688,#28689,#28690,#28691,#28692,
#28693,#28694,#28695,#28696,#28697,#28698,#28699,#28700,#28701,#28702,#28703,
#28704,#28705,#28706,#28707,#28708,#28709,#28710,#28711,#28712,#28713,#28714,
#28715,#28716,#28717,#28718,#28719,#28720,#28721,#28722,#28723,#28724,#28725,
#28726,#28727,#28728,#28729,#28730,#28731,#28732,#28733,#28734,#28735,#28736,
#28737,#28738,#28739,#28740,#28741,#28742,#28743,#28744,#28745,#28746,#28747,
#28748,#28749,#28750,#28751,#28752,#28753,#28754,#28755,#28756,#28757,#28758,
#28759,#28760,#28761,#28762,#28763,#28764,#28765,#28766,#28767,#28768,#28769,
#28770,#28771,#28772,#28773,#28774,#28775,#28776,#28777,#28778,#28779,#28780,
#28781,#28782,#28783,#28784,#28785,#28786,#28787,#28788,#28789,#28790,#28791,
#28792,#28793,#28794,#28795,#28796,#28797,#28798,#28799,#28800,#28801,#28802,
#28803,#28804,#28805,#28806,#28807,#28808,#28809,#28810,#28811,#28812,#28813,
#28814,#28815,#28816,#28817,#28818,#28819,#28820,#28821,#28822,#28823,#28824,
#28825,#28826,#28827,#28828,#28829,#28830,#28831,#28832,#28833,#28834,#28835,
#28836,#28837,#28838,#28839,#28840,#28841,#28842,#28843,#28844,#28845,#28846,
#28847,#28848,#28849,#28850,#28851),(#28852,#28853,#28854,#28855,#28856,
#28857,#28858,#28859,#28860,#28861,#28862,#28863,#28864,#28865,#28866,#28867,
#28868,#28869,#28870,#28871,#28872,#28873,#28874,#28875,#28876,#28877,#28878,
#28879,#28880,#28881,#28882,#28883,#28884,#28885,#28886,#28887,#28888,#28889,
#28890,#28891,#28892,#28893,#28894,#28895,#28896,#28897,#28898,#28899,#28900,
#28901,#28902,#28903,#28904,#28905,#28906,#28907,#28908,#28909,#28910,#28911,
#28912,#28913,#28914,#28915,#28916,#28917,#28918,#28919,#28920,#28921,#28922,
#28923,#28924,#28925,#28926,#28927,#28928,#28929,#28930,#28931,#28932,#28933,
#28934,#28935,#28936,#28937,#28938,#28939,#28940,#28941,#28942,#28943,#28944,
#28945,#28946,#28947,#28948,#28949,#28950,#28951,#28952,#28953,#28954,#28955,
#28956,#28957,#28958,#28959,#28960,#28961,#28962,#28963,#28964,#28965,#28966,
#28967,#28968,#28969,#28970,#28971,#28972,#28973,#28974,#28975,#28976,#28977,
#28978,#28979,#28980,#28981,#28982,#28983,#28984,#28985,#28986,#28987,#28988,
#28989,#28990,#28991,#28992,#28993,#28994,#28995,#28996,#28997,#28998,#28999,
#29000,#29001,#29002,#29003,#29004,#29005,#29006,#29007,#29008,#29009,#29010,
#29011,#29012,#29013,#29014,#29015,#29016,#29017,#29018,#29019,#29020,#29021,
#29022,#29023,#29024,#29025,#29026,#29027,#29028,#29029,#29030,#29031,#29032,
#29033,#29034,#29035,#29036,#29037,#29038,#29039,#29040,#29041,#29042,#29043,
#29044,#29045,#29046,#29047,#29048,#29049,#29050,#29051,#29052,#29053,#29054,
#29055,#29056,#29057,#29058,#29059,#29060,#29061,#29062,#29063,#29064,#29065,
#29066,#29067,#29068,#29069,#29070,#29071,#29072,#29073,#29074,#29075,#29076,
#29077,#29078,#29079,#29080,#29081,#29082,#29083,#29084,#29085,#29086,#29087,
#29088,#29089,#29090,#29091,#29092),(#29093,#29094,#29095,#29096,#29097,
#29098,#29099,#29100,#29101,#29102,#29103,#29104,#29105,#29106,#29107,#29108,
#29109,#29110,#29111,#29112,#29113,#29114,#29115,#29116,#29117,#29118,#29119,
#29120,#29121,#29122,#29123,#29124,#29125,#29126,#29127,#29128,#29129,#29130,
#29131,#29132,#29133,#29134,#29135,#29136,#29137,#29138,#29139,#29140,#29141,
#29142,#29143,#29144,#29145,#29146,#29147,#29148,#29149,#29150,#29151,#29152,
#29153,#29154,#29155,#29156,#29157,#29158,#29159,#29160,#29161,#29162,#29163,
#29164,#29165,#29166,#29167,#29168,#29169,#29170,#29171,#29172,#29173,#29174,
#29175,#29176,#29177,#29178,#29179,#29180,#29181,#29182,#29183,#29184,#29185,
#29186,#29187,#29188,#29189,#29190,#29191,#29192,#29193,#29194,#29195,#29196,
#29197,#29198,#29199,#29200,#29201,#29202,#29203,#29204,#29205,#29206,#29207,
#29208,#29209,#29210,#29211,#29212,#29213,#29214,#29215,#29216,#29217,#29218,
#29219,#29220,#29221,#29222,#29223,#29224,#29225,#29226,#29227,#29228,#29229,
#29230,#29231,#29232,#29233,#29234,#29235,#29236,#29237,#29238,#29239,#29240,
#29241,#29242,#29243,#29244,#29245,#29246,#29247,#29248,#29249,#29250,#29251,
#29252,#29253,#29254,#29255,#29256,#29257,#29258,#29259,#29260,#29261,#29262,
#29263,#29264,#29265,#29266,#29267,#29268,#29269,#29270,#29271,#29272,#29273,
#29274,#29275,#29276,#29277,#29278,#29279,#29280,#29281,#29282,#29283,#29284,
#29285,#29286,#29287,#29288,#29289,#29290,#29291,#29292,#29293,#29294,#29295,
#29296,#29297,#29298,#29299,#29300,#29301,#29302,#29303,#29304,#29305,#29306,
#29307,#29308,#29309,#29310,#29311,#29312,#29313,#29314,#29315,#29316,#29317,
#29318,#29319,#29320,#29321,#29322,#29323,#29324,#29325,#29326,#29327,#29328,
#29329,#29330,#29331,#29332,#29333),(#29334,#29335,#29336,#29337,#29338,
#29339,#29340,#29341,#29342,#29343,#29344,#29345,#29346,#29347,#29348,#29349,
#29350,#29351,#29352,#29353,#29354,#29355,#29356,#29357,#29358,#29359,#29360,
#29361,#29362,#29363,#29364,#29365,#29366,#29367,#29368,#29369,#29370,#29371,
#29372,#29373,#29374,#29375,#29376,#29377,#29378,#29379,#29380,#29381,#29382,
#29383,#29384,#29385,#29386,#29387,#29388,#29389,#29390,#29391,#29392,#29393,
#29394,#29395,#29396,#29397,#29398,#29399,#29400,#29401,#29402,#29403,#29404,
#29405,#29406,#29407,#29408,#29409,#29410,#29411,#29412,#29413,#29414,#29415,
#29416,#29417,#29418,#29419,#29420,#29421,#29422,#29423,#29424,#29425,#29426,
#29427,#29428,#29429,#29430,#29431,#29432,#29433,#29434,#29435,#29436,#29437,
#29438,#29439,#29440,#29441,#29442,#29443,#29444,#29445,#29446,#29447,#29448,
#29449,#29450,#29451,#29452,#29453,#29454,#29455,#29456,#29457,#29458,#29459,
#29460,#29461,#29462,#29463,#29464,#29465,#29466,#29467,#29468,#29469,#29470,
#29471,#29472,#29473,#29474,#29475,#29476,#29477,#29478,#29479,#29480,#29481,
#29482,#29483,#29484,#29485,#29486,#29487,#29488,#29489,#29490,#29491,#29492,
#29493,#29494,#29495,#29496,#29497,#29498,#29499,#29500,#29501,#29502,#29503,
#29504,#29505,#29506,#29507,#29508,#29509,#29510,#29511,#29512,#29513,#29514,
#29515,#29516,#29517,#29518,#29519,#29520,#29521,#29522,#29523,#29524,#29525,
#29526,#29527,#29528,#29529,#29530,#29531,#29532,#29533,#29534,#29535,#29536,
#29537,#29538,#29539,#29540,#29541,#29542,#29543,#29544,#29545,#29546,#29547,
#29548,#29549,#29550,#29551,#29552,#29553,#29554,#29555,#29556,#29557,#29558,
#29559,#29560,#29561,#29562,#29563,#29564,#29565,#29566,#29567,#29568,#29569,
#29570,#29571,#29572,#29573,#29574)),.UNSPECIFIED.,.F.,.F.,.F.,(4,4),(4,
1,1,1,1,1,1,1,1,1,1,1,1,1,1,1,1,1,1,1,1,1,1,1,1,1,1,1,1,1,1,1,1,1,1,1,1,
1,1,1,1,1,1,1,1,1,1,1,1,1,1,1,1,1,1,1,1,1,1,1,1,1,1,1,1,1,1,1,1,1,1,1,1,
1,1,1,1,1,1,1,1,1,1,1,1,1,1,1,1,1,1,1,1,1,1,1,1,1,1,1,1,1,1,1,1,1,1,1,1,
1,1,1,1,1,1,1,1,1,1,1,1,1,1,1,1,1,1,1,1,1,1,1,1,1,1,1,1,1,1,1,1,1,1,1,1,
1,1,1,1,1,1,1,1,1,1,1,1,1,1,1,1,1,1,1,1,1,1,1,1,1,1,1,1,1,1,1,1,1,1,1,1,
1,1,1,1,1,1,1,1,1,1,1,1,1,1,1,1,1,1,1,1,1,1,1,1,1,1,1,1,1,1,1,1,1,1,1,1,
1,1,1,1,1,1,1,1,1,1,1,1,1,1,1,1,1,1,1,1,1,4),(-0.000369208222476486,0.0530376906591354),
(11.6159809837193,12.6150740657025,13.6137549340633,14.612435802424,15.6111166707848,
16.6097975391455,17.6084784075063,18.607159275867,19.6058401442278,20.6045210125885,
21.6032018809493,22.60188274931,23.6005636176708,24.5992444860315,25.5979253543923,
26.596606222753,27.5952870911138,28.5939679594746,29.5926488278353,30.5913296961961,
31.5900105645568,32.5886914329176,33.5873723012783,34.5860531696391,35.5847340379998,
36.5834149063606,37.5820957747213,38.5807766430821,39.5794575114428,40.5781383798036,
41.5768192481643,42.5755001165251,43.5741809848858,44.5728618532466,45.5715427216073,
46.5702235899681,47.5689044583288,48.5675853266896,49.5662661950503,50.5649470634111,
51.5636279317718,52.5623088001326,53.5609896684933,54.5596705368541,55.5583514052148,
56.5570322735756,57.5557131419363,58.5543940102971,59.5530748786578,60.5517557470186,
61.5504366153793,62.5491174837401,63.5477983521008,64.5464792204616,65.5451600888223,
66.5438409571831,67.5425218255438,68.5412026939046,69.5398835622653,70.5385644306261,
71.5372452989868,72.5359261673476,73.5346070357083,74.5332879040691,75.5319687724298,
76.5306496407906,77.5293305091514,78.5280113775121,79.5266922458729,80.5253731142336,
81.5240539825944,82.5227348509551,83.5214157193159,84.5200965876766,85.5187774560374,
86.5174583243981,87.5161391927589,88.5148200611196,89.5135009294804,90.5121817978411,
91.5108626662019,92.5095435345626,93.5082244029234,94.5069052712841,95.5055861396449,
96.5042670080056,97.5029478763664,98.5016287447271,99.5003096130879,100.498990481449,
101.497671349809,102.49635221817,103.495033086531,104.493713954892,105.492394823252,
106.491075691613,107.489756559974,108.488437428335,109.487118296695,110.485799165056,
111.484480033417,112.483160901778,113.481841770138,114.480522638499,115.47920350686,
116.477884375221,117.476565243581,118.475246111942,119.473926980303,120.472607848664,
121.471288717024,122.469969585385,123.468650453746,124.467331322107,125.466012190467,
126.464693058828,127.463373927189,128.46205479555,129.46073566391,130.459416532271,
131.458097400632,132.456778268993,133.455459137353,134.454140005714,135.452820874075,
136.451501742436,137.450182610796,138.448863479157,139.447544347518,140.446225215879,
141.444906084239,142.4435869526,143.442267820961,144.440948689322,145.439629557682,
146.438310426043,147.436991294404,148.435672162765,149.434353031125,150.433033899486,
151.431714767847,152.430395636208,153.429076504568,154.427757372929,155.42643824129,
156.425119109651,157.423799978011,158.422480846372,159.421161714733,160.419842583094,
161.418523451454,162.417204319815,163.415885188176,164.414566056537,165.413246924897,
166.411927793258,167.410608661619,168.40928952998,169.40797039834,170.406651266701,
171.405332135062,172.404013003423,173.402693871783,174.401374740144,175.400055608505,
176.398736476866,177.397417345226,178.396098213587,179.394779081948,180.393459950309,
181.392140818669,182.39082168703,183.389502555391,184.388183423752,185.386864292112,
186.385545160473,187.384226028834,188.382906897195,189.381587765555,190.380268633916,
191.378949502277,192.377630370638,193.376311238999,194.374992107359,195.37367297572,
196.372353844081,197.371034712442,198.369715580802,199.368396449163,200.367077317524,
201.365758185885,202.364439054245,203.363119922606,204.361800790967,205.360481659328,
206.359162527688,207.357843396049,208.35652426441,209.355205132771,210.353886001131,
211.352566869492,212.351247737853,213.349928606214,214.348609474574,215.347290342935,
216.345971211296,217.344652079657,218.343332948017,219.342013816378,220.340694684739,
221.3393755531,222.33805642146,223.336737289821,224.335418158182,225.334099026543,
226.332779894903,227.331460763264,228.330141631625,229.328822499986,230.327503368346,
231.326184236707,232.324865105068,233.323545973429,234.322226841789,235.32090771015,
236.319588578511,237.318269446872,238.316950315232,239.315631183593,240.314312051954,
241.312992920315,242.311673788675,243.310354657036,244.309035525397,245.307716393758,
246.306397262118,247.305078130479,248.30375899884,249.302622768849),
 .UNSPECIFIED.);
#86=B_SPLINE_SURFACE_WITH_KNOTS('',3,3,((#32554,#32555,#32556,#32557,#32558,
#32559,#32560,#32561,#32562,#32563,#32564,#32565,#32566,#32567,#32568,#32569,
#32570,#32571,#32572,#32573,#32574,#32575,#32576,#32577,#32578,#32579,#32580,
#32581,#32582,#32583,#32584,#32585,#32586,#32587,#32588,#32589,#32590,#32591,
#32592,#32593,#32594,#32595,#32596,#32597,#32598,#32599,#32600,#32601,#32602,
#32603,#32604,#32605,#32606,#32607,#32608,#32609,#32610,#32611,#32612,#32613,
#32614,#32615,#32616,#32617,#32618,#32619,#32620),(#32621,#32622,#32623,
#32624,#32625,#32626,#32627,#32628,#32629,#32630,#32631,#32632,#32633,#32634,
#32635,#32636,#32637,#32638,#32639,#32640,#32641,#32642,#32643,#32644,#32645,
#32646,#32647,#32648,#32649,#32650,#32651,#32652,#32653,#32654,#32655,#32656,
#32657,#32658,#32659,#32660,#32661,#32662,#32663,#32664,#32665,#32666,#32667,
#32668,#32669,#32670,#32671,#32672,#32673,#32674,#32675,#32676,#32677,#32678,
#32679,#32680,#32681,#32682,#32683,#32684,#32685,#32686,#32687),(#32688,
#32689,#32690,#32691,#32692,#32693,#32694,#32695,#32696,#32697,#32698,#32699,
#32700,#32701,#32702,#32703,#32704,#32705,#32706,#32707,#32708,#32709,#32710,
#32711,#32712,#32713,#32714,#32715,#32716,#32717,#32718,#32719,#32720,#32721,
#32722,#32723,#32724,#32725,#32726,#32727,#32728,#32729,#32730,#32731,#32732,
#32733,#32734,#32735,#32736,#32737,#32738,#32739,#32740,#32741,#32742,#32743,
#32744,#32745,#32746,#32747,#32748,#32749,#32750,#32751,#32752,#32753,#32754),
(#32755,#32756,#32757,#32758,#32759,#32760,#32761,#32762,#32763,#32764,
#32765,#32766,#32767,#32768,#32769,#32770,#32771,#32772,#32773,#32774,#32775,
#32776,#32777,#32778,#32779,#32780,#32781,#32782,#32783,#32784,#32785,#32786,
#32787,#32788,#32789,#32790,#32791,#32792,#32793,#32794,#32795,#32796,#32797,
#32798,#32799,#32800,#32801,#32802,#32803,#32804,#32805,#32806,#32807,#32808,
#32809,#32810,#32811,#32812,#32813,#32814,#32815,#32816,#32817,#32818,#32819,
#32820,#32821),(#32822,#32823,#32824,#32825,#32826,#32827,#32828,#32829,
#32830,#32831,#32832,#32833,#32834,#32835,#32836,#32837,#32838,#32839,#32840,
#32841,#32842,#32843,#32844,#32845,#32846,#32847,#32848,#32849,#32850,#32851,
#32852,#32853,#32854,#32855,#32856,#32857,#32858,#32859,#32860,#32861,#32862,
#32863,#32864,#32865,#32866,#32867,#32868,#32869,#32870,#32871,#32872,#32873,
#32874,#32875,#32876,#32877,#32878,#32879,#32880,#32881,#32882,#32883,#32884,
#32885,#32886,#32887,#32888),(#32889,#32890,#32891,#32892,#32893,#32894,
#32895,#32896,#32897,#32898,#32899,#32900,#32901,#32902,#32903,#32904,#32905,
#32906,#32907,#32908,#32909,#32910,#32911,#32912,#32913,#32914,#32915,#32916,
#32917,#32918,#32919,#32920,#32921,#32922,#32923,#32924,#32925,#32926,#32927,
#32928,#32929,#32930,#32931,#32932,#32933,#32934,#32935,#32936,#32937,#32938,
#32939,#32940,#32941,#32942,#32943,#32944,#32945,#32946,#32947,#32948,#32949,
#32950,#32951,#32952,#32953,#32954,#32955),(#32956,#32957,#32958,#32959,
#32960,#32961,#32962,#32963,#32964,#32965,#32966,#32967,#32968,#32969,#32970,
#32971,#32972,#32973,#32974,#32975,#32976,#32977,#32978,#32979,#32980,#32981,
#32982,#32983,#32984,#32985,#32986,#32987,#32988,#32989,#32990,#32991,#32992,
#32993,#32994,#32995,#32996,#32997,#32998,#32999,#33000,#33001,#33002,#33003,
#33004,#33005,#33006,#33007,#33008,#33009,#33010,#33011,#33012,#33013,#33014,
#33015,#33016,#33017,#33018,#33019,#33020,#33021,#33022),(#33023,#33024,
#33025,#33026,#33027,#33028,#33029,#33030,#33031,#33032,#33033,#33034,#33035,
#33036,#33037,#33038,#33039,#33040,#33041,#33042,#33043,#33044,#33045,#33046,
#33047,#33048,#33049,#33050,#33051,#33052,#33053,#33054,#33055,#33056,#33057,
#33058,#33059,#33060,#33061,#33062,#33063,#33064,#33065,#33066,#33067,#33068,
#33069,#33070,#33071,#33072,#33073,#33074,#33075,#33076,#33077,#33078,#33079,
#33080,#33081,#33082,#33083,#33084,#33085,#33086,#33087,#33088,#33089),
(#33090,#33091,#33092,#33093,#33094,#33095,#33096,#33097,#33098,#33099,
#33100,#33101,#33102,#33103,#33104,#33105,#33106,#33107,#33108,#33109,#33110,
#33111,#33112,#33113,#33114,#33115,#33116,#33117,#33118,#33119,#33120,#33121,
#33122,#33123,#33124,#33125,#33126,#33127,#33128,#33129,#33130,#33131,#33132,
#33133,#33134,#33135,#33136,#33137,#33138,#33139,#33140,#33141,#33142,#33143,
#33144,#33145,#33146,#33147,#33148,#33149,#33150,#33151,#33152,#33153,#33154,
#33155,#33156),(#33157,#33158,#33159,#33160,#33161,#33162,#33163,#33164,
#33165,#33166,#33167,#33168,#33169,#33170,#33171,#33172,#33173,#33174,#33175,
#33176,#33177,#33178,#33179,#33180,#33181,#33182,#33183,#33184,#33185,#33186,
#33187,#33188,#33189,#33190,#33191,#33192,#33193,#33194,#33195,#33196,#33197,
#33198,#33199,#33200,#33201,#33202,#33203,#33204,#33205,#33206,#33207,#33208,
#33209,#33210,#33211,#33212,#33213,#33214,#33215,#33216,#33217,#33218,#33219,
#33220,#33221,#33222,#33223)),.UNSPECIFIED.,.T.,.F.,.F.,(4,1,1,1,1,1,1,
4),(4,1,1,1,1,1,1,1,1,1,1,1,1,1,1,1,1,1,1,1,1,1,1,1,1,1,1,1,1,1,1,1,1,1,
1,1,1,1,1,1,1,1,1,1,1,1,1,1,1,1,1,1,1,1,1,1,1,1,1,1,1,1,1,1,4),(-3.14159265358979,
-2.24399475256414,-1.34639685153848,-0.448798950512828,0.448798950512828,
1.34639685153848,2.24399475256414,3.14159265358979),(0.,0.490873852123405,
0.98174770424681,1.47262155637022,1.96349540849362,2.45436926061703,2.94524311274043,
3.43611696486384,3.92699081698724,4.41786466911065,4.90873852123405,5.39961237335746,
5.89048622548086,6.38136007760427,6.87223392972767,7.36310778185108,7.85398163397448,
8.34485548609789,8.83572933822129,9.3266031903447,9.8174770424681,10.3083508945915,
10.7992247467149,11.2900985988383,11.7809724509617,12.2718463030851,12.7627201552085,
13.2535940073319,13.7444678594553,14.2353417115787,14.7262155637022,15.2170894158256,
15.707963267949,16.1988371200724,16.6897109721958,17.1805848243192,17.6714586764426,
18.162332528566,18.6532063806894,19.1440802328128,19.6349540849362,20.1258279370596,
20.616701789183,21.1075756413064,21.5984494934298,22.0893233455532,22.5801971976766,
23.0710710498,23.5619449019234,24.0528187540469,24.5436926061703,25.0345664582937,
25.5254403104171,26.0163141625405,26.5071880146639,26.9980618667873,27.4889357189107,
27.9798095710341,28.4706834231575,28.9615572752809,29.4524311274043,29.9433049795277,
30.4341788316511,30.9250526837745,31.4159265358979),.UNSPECIFIED.);
#87=FACE_BOUND('',#425,.T.);
#88=FACE_BOUND('',#511,.T.);
#89=FACE_BOUND('',#540,.T.);
#90=FACE_BOUND('',#543,.T.);
#91=PLANE('',#2883);
#92=PLANE('',#2962);
#93=PLANE('',#3087);
#94=PLANE('',#3088);
#95=PLANE('',#3126);
#96=PLANE('',#3127);
#97=PLANE('',#3129);
#98=PLANE('',#3130);
#99=PLANE('',#3133);
#100=PLANE('',#3134);
#101=PLANE('',#3135);
#102=PLANE('',#3136);
#103=PLANE('',#3137);
#104=PLANE('',#3141);
#105=LINE('',#27458,#202);
#106=LINE('',#27464,#203);
#107=LINE('',#29795,#204);
#108=LINE('',#29798,#205);
#109=LINE('',#29837,#206);
#110=LINE('',#29840,#207);
#111=LINE('',#29879,#208);
#112=LINE('',#29882,#209);
#113=LINE('',#29921,#210);
#114=LINE('',#29924,#211);
#115=LINE('',#29963,#212);
#116=LINE('',#29966,#213);
#117=LINE('',#30005,#214);
#118=LINE('',#30008,#215);
#119=LINE('',#30047,#216);
#120=LINE('',#30050,#217);
#121=LINE('',#30089,#218);
#122=LINE('',#30092,#219);
#123=LINE('',#30131,#220);
#124=LINE('',#30134,#221);
#125=LINE('',#30159,#222);
#126=LINE('',#30163,#223);
#127=LINE('',#30220,#224);
#128=LINE('',#30223,#225);
#129=LINE('',#30262,#226);
#130=LINE('',#30265,#227);
#131=LINE('',#30304,#228);
#132=LINE('',#30307,#229);
#133=LINE('',#30346,#230);
#134=LINE('',#30349,#231);
#135=LINE('',#30388,#232);
#136=LINE('',#30391,#233);
#137=LINE('',#30430,#234);
#138=LINE('',#30433,#235);
#139=LINE('',#30472,#236);
#140=LINE('',#30475,#237);
#141=LINE('',#30514,#238);
#142=LINE('',#30517,#239);
#143=LINE('',#30556,#240);
#144=LINE('',#30559,#241);
#145=LINE('',#30598,#242);
#146=LINE('',#30601,#243);
#147=LINE('',#30640,#244);
#148=LINE('',#30643,#245);
#149=LINE('',#30682,#246);
#150=LINE('',#30685,#247);
#151=LINE('',#30724,#248);
#152=LINE('',#30727,#249);
#153=LINE('',#30766,#250);
#154=LINE('',#30769,#251);
#155=LINE('',#30808,#252);
#156=LINE('',#30811,#253);
#157=LINE('',#30850,#254);
#158=LINE('',#30853,#255);
#159=LINE('',#30892,#256);
#160=LINE('',#30895,#257);
#161=LINE('',#30934,#258);
#162=LINE('',#30937,#259);
#163=LINE('',#30976,#260);
#164=LINE('',#30979,#261);
#165=LINE('',#31018,#262);
#166=LINE('',#31021,#263);
#167=LINE('',#31060,#264);
#168=LINE('',#31063,#265);
#169=LINE('',#31102,#266);
#170=LINE('',#31105,#267);
#171=LINE('',#31144,#268);
#172=LINE('',#31147,#269);
#173=LINE('',#31186,#270);
#174=LINE('',#31189,#271);
#175=LINE('',#31228,#272);
#176=LINE('',#31231,#273);
#177=LINE('',#31270,#274);
#178=LINE('',#31273,#275);
#179=LINE('',#31312,#276);
#180=LINE('',#31315,#277);
#181=LINE('',#31354,#278);
#182=LINE('',#31357,#279);
#183=LINE('',#31396,#280);
#184=LINE('',#31399,#281);
#185=LINE('',#31447,#282);
#186=LINE('',#31563,#283);
#187=LINE('',#31572,#284);
#188=LINE('',#31581,#285);
#189=LINE('',#31923,#286);
#190=LINE('',#32065,#287);
#191=LINE('',#32074,#288);
#192=LINE('',#32416,#289);
#193=LINE('',#33375,#290);
#194=LINE('',#33381,#291);
#195=LINE('',#33391,#292);
#196=LINE('',#33399,#293);
#197=LINE('',#33423,#294);
#198=LINE('',#33433,#295);
#199=LINE('',#33439,#296);
#200=LINE('',#33450,#297);
#201=LINE('',#33455,#298);
#202=VECTOR('',#3169,4.);
#203=VECTOR('',#3176,4.5);
#204=VECTOR('',#3185,10.);
#205=VECTOR('',#3188,10.);
#206=VECTOR('',#3191,10.);
#207=VECTOR('',#3194,10.);
#208=VECTOR('',#3197,10.);
#209=VECTOR('',#3200,10.);
#210=VECTOR('',#3203,10.);
#211=VECTOR('',#3206,10.);
#212=VECTOR('',#3209,10.);
#213=VECTOR('',#3212,10.);
#214=VECTOR('',#3215,10.);
#215=VECTOR('',#3218,10.);
#216=VECTOR('',#3221,10.);
#217=VECTOR('',#3224,10.);
#218=VECTOR('',#3227,10.);
#219=VECTOR('',#3230,10.);
#220=VECTOR('',#3233,10.);
#221=VECTOR('',#3236,10.);
#222=VECTOR('',#3239,10.);
#223=VECTOR('',#3242,10.);
#224=VECTOR('',#3245,10.);
#225=VECTOR('',#3248,10.);
#226=VECTOR('',#3251,10.);
#227=VECTOR('',#3254,10.);
#228=VECTOR('',#3257,10.);
#229=VECTOR('',#3260,10.);
#230=VECTOR('',#3263,10.);
#231=VECTOR('',#3266,10.);
#232=VECTOR('',#3269,10.);
#233=VECTOR('',#3272,10.);
#234=VECTOR('',#3275,10.);
#235=VECTOR('',#3278,10.);
#236=VECTOR('',#3281,10.);
#237=VECTOR('',#3284,10.);
#238=VECTOR('',#3287,10.);
#239=VECTOR('',#3290,10.);
#240=VECTOR('',#3293,10.);
#241=VECTOR('',#3296,10.);
#242=VECTOR('',#3299,10.);
#243=VECTOR('',#3302,10.);
#244=VECTOR('',#3305,10.);
#245=VECTOR('',#3308,10.);
#246=VECTOR('',#3311,10.);
#247=VECTOR('',#3314,10.);
#248=VECTOR('',#3317,10.);
#249=VECTOR('',#3320,10.);
#250=VECTOR('',#3323,10.);
#251=VECTOR('',#3326,10.);
#252=VECTOR('',#3329,10.);
#253=VECTOR('',#3332,10.);
#254=VECTOR('',#3335,10.);
#255=VECTOR('',#3338,10.);
#256=VECTOR('',#3341,10.);
#257=VECTOR('',#3344,10.);
#258=VECTOR('',#3347,10.);
#259=VECTOR('',#3350,10.);
#260=VECTOR('',#3353,10.);
#261=VECTOR('',#3356,10.);
#262=VECTOR('',#3359,10.);
#263=VECTOR('',#3362,10.);
#264=VECTOR('',#3365,10.);
#265=VECTOR('',#3368,10.);
#266=VECTOR('',#3371,10.);
#267=VECTOR('',#3374,10.);
#268=VECTOR('',#3377,10.);
#269=VECTOR('',#3380,10.);
#270=VECTOR('',#3383,10.);
#271=VECTOR('',#3386,10.);
#272=VECTOR('',#3389,10.);
#273=VECTOR('',#3392,10.);
#274=VECTOR('',#3395,10.);
#275=VECTOR('',#3398,10.);
#276=VECTOR('',#3401,10.);
#277=VECTOR('',#3404,10.);
#278=VECTOR('',#3407,10.);
#279=VECTOR('',#3410,10.);
#280=VECTOR('',#3413,10.);
#281=VECTOR('',#3416,10.);
#282=VECTOR('',#3505,10.);
#283=VECTOR('',#3666,10.);
#284=VECTOR('',#3679,16.067990296595);
#285=VECTOR('',#3692,15.7712719335665);
#286=VECTOR('',#3703,3.5);
#287=VECTOR('',#3718,16.067990296595);
#288=VECTOR('',#3731,15.7712719335665);
#289=VECTOR('',#3742,3.5);
#290=VECTOR('',#3761,10.);
#291=VECTOR('',#3762,10.);
#292=VECTOR('',#3765,10.);
#293=VECTOR('',#3770,3.73625);
#294=VECTOR('',#3773,10.);
#295=VECTOR('',#3776,10.);
#296=VECTOR('',#3779,10.);
#297=VECTOR('',#3790,3.73625);
#298=VECTOR('',#3797,2.);
#299=FACE_OUTER_BOUND('',#420,.T.);
#300=FACE_OUTER_BOUND('',#421,.T.);
#301=FACE_OUTER_BOUND('',#422,.T.);
#302=FACE_OUTER_BOUND('',#423,.T.);
#303=FACE_OUTER_BOUND('',#424,.T.);
#304=FACE_OUTER_BOUND('',#426,.T.);
#305=FACE_OUTER_BOUND('',#427,.T.);
#306=FACE_OUTER_BOUND('',#428,.T.);
#307=FACE_OUTER_BOUND('',#429,.T.);
#308=FACE_OUTER_BOUND('',#430,.T.);
#309=FACE_OUTER_BOUND('',#431,.T.);
#310=FACE_OUTER_BOUND('',#432,.T.);
#311=FACE_OUTER_BOUND('',#433,.T.);
#312=FACE_OUTER_BOUND('',#434,.T.);
#313=FACE_OUTER_BOUND('',#435,.T.);
#314=FACE_OUTER_BOUND('',#436,.T.);
#315=FACE_OUTER_BOUND('',#437,.T.);
#316=FACE_OUTER_BOUND('',#438,.T.);
#317=FACE_OUTER_BOUND('',#439,.T.);
#318=FACE_OUTER_BOUND('',#440,.T.);
#319=FACE_OUTER_BOUND('',#441,.T.);
#320=FACE_OUTER_BOUND('',#442,.T.);
#321=FACE_OUTER_BOUND('',#443,.T.);
#322=FACE_OUTER_BOUND('',#444,.T.);
#323=FACE_OUTER_BOUND('',#445,.T.);
#324=FACE_OUTER_BOUND('',#446,.T.);
#325=FACE_OUTER_BOUND('',#447,.T.);
#326=FACE_OUTER_BOUND('',#448,.T.);
#327=FACE_OUTER_BOUND('',#449,.T.);
#328=FACE_OUTER_BOUND('',#450,.T.);
#329=FACE_OUTER_BOUND('',#451,.T.);
#330=FACE_OUTER_BOUND('',#452,.T.);
#331=FACE_OUTER_BOUND('',#453,.T.);
#332=FACE_OUTER_BOUND('',#454,.T.);
#333=FACE_OUTER_BOUND('',#455,.T.);
#334=FACE_OUTER_BOUND('',#456,.T.);
#335=FACE_OUTER_BOUND('',#457,.T.);
#336=FACE_OUTER_BOUND('',#458,.T.);
#337=FACE_OUTER_BOUND('',#459,.T.);
#338=FACE_OUTER_BOUND('',#460,.T.);
#339=FACE_OUTER_BOUND('',#461,.T.);
#340=FACE_OUTER_BOUND('',#462,.T.);
#341=FACE_OUTER_BOUND('',#463,.T.);
#342=FACE_OUTER_BOUND('',#464,.T.);
#343=FACE_OUTER_BOUND('',#465,.T.);
#344=FACE_OUTER_BOUND('',#466,.T.);
#345=FACE_OUTER_BOUND('',#467,.T.);
#346=FACE_OUTER_BOUND('',#468,.T.);
#347=FACE_OUTER_BOUND('',#469,.T.);
#348=FACE_OUTER_BOUND('',#470,.T.);
#349=FACE_OUTER_BOUND('',#471,.T.);
#350=FACE_OUTER_BOUND('',#472,.T.);
#351=FACE_OUTER_BOUND('',#473,.T.);
#352=FACE_OUTER_BOUND('',#474,.T.);
#353=FACE_OUTER_BOUND('',#475,.T.);
#354=FACE_OUTER_BOUND('',#476,.T.);
#355=FACE_OUTER_BOUND('',#477,.T.);
#356=FACE_OUTER_BOUND('',#478,.T.);
#357=FACE_OUTER_BOUND('',#479,.T.);
#358=FACE_OUTER_BOUND('',#480,.T.);
#359=FACE_OUTER_BOUND('',#481,.T.);
#360=FACE_OUTER_BOUND('',#482,.T.);
#361=FACE_OUTER_BOUND('',#483,.T.);
#362=FACE_OUTER_BOUND('',#484,.T.);
#363=FACE_OUTER_BOUND('',#485,.T.);
#364=FACE_OUTER_BOUND('',#486,.T.);
#365=FACE_OUTER_BOUND('',#487,.T.);
#366=FACE_OUTER_BOUND('',#488,.T.);
#367=FACE_OUTER_BOUND('',#489,.T.);
#368=FACE_OUTER_BOUND('',#490,.T.);
#369=FACE_OUTER_BOUND('',#491,.T.);
#370=FACE_OUTER_BOUND('',#492,.T.);
#371=FACE_OUTER_BOUND('',#493,.T.);
#372=FACE_OUTER_BOUND('',#494,.T.);
#373=FACE_OUTER_BOUND('',#495,.T.);
#374=FACE_OUTER_BOUND('',#496,.T.);
#375=FACE_OUTER_BOUND('',#497,.T.);
#376=FACE_OUTER_BOUND('',#498,.T.);
#377=FACE_OUTER_BOUND('',#499,.T.);
#378=FACE_OUTER_BOUND('',#500,.T.);
#379=FACE_OUTER_BOUND('',#501,.T.);
#380=FACE_OUTER_BOUND('',#502,.T.);
#381=FACE_OUTER_BOUND('',#503,.T.);
#382=FACE_OUTER_BOUND('',#504,.T.);
#383=FACE_OUTER_BOUND('',#505,.T.);
#384=FACE_OUTER_BOUND('',#506,.T.);
#385=FACE_OUTER_BOUND('',#507,.T.);
#386=FACE_OUTER_BOUND('',#508,.T.);
#387=FACE_OUTER_BOUND('',#509,.T.);
#388=FACE_OUTER_BOUND('',#510,.T.);
#389=FACE_OUTER_BOUND('',#512,.T.);
#390=FACE_OUTER_BOUND('',#513,.T.);
#391=FACE_OUTER_BOUND('',#514,.T.);
#392=FACE_OUTER_BOUND('',#515,.T.);
#393=FACE_OUTER_BOUND('',#516,.T.);
#394=FACE_OUTER_BOUND('',#517,.T.);
#395=FACE_OUTER_BOUND('',#518,.T.);
#396=FACE_OUTER_BOUND('',#519,.T.);
#397=FACE_OUTER_BOUND('',#520,.T.);
#398=FACE_OUTER_BOUND('',#521,.T.);
#399=FACE_OUTER_BOUND('',#522,.T.);
#400=FACE_OUTER_BOUND('',#523,.T.);
#401=FACE_OUTER_BOUND('',#524,.T.);
#402=FACE_OUTER_BOUND('',#525,.T.);
#403=FACE_OUTER_BOUND('',#526,.T.);
#404=FACE_OUTER_BOUND('',#527,.T.);
#405=FACE_OUTER_BOUND('',#528,.T.);
#406=FACE_OUTER_BOUND('',#529,.T.);
#407=FACE_OUTER_BOUND('',#530,.T.);
#408=FACE_OUTER_BOUND('',#531,.T.);
#409=FACE_OUTER_BOUND('',#532,.T.);
#410=FACE_OUTER_BOUND('',#533,.T.);
#411=FACE_OUTER_BOUND('',#534,.T.);
#412=FACE_OUTER_BOUND('',#535,.T.);
#413=FACE_OUTER_BOUND('',#536,.T.);
#414=FACE_OUTER_BOUND('',#537,.T.);
#415=FACE_OUTER_BOUND('',#538,.T.);
#416=FACE_OUTER_BOUND('',#539,.T.);
#417=FACE_OUTER_BOUND('',#541,.T.);
#418=FACE_OUTER_BOUND('',#542,.T.);
#419=FACE_OUTER_BOUND('',#544,.T.);
#420=EDGE_LOOP('',(#1687,#1688,#1689,#1690,#1691,#1692,#1693,#1694,#1695,
#1696,#1697,#1698,#1699,#1700,#1701,#1702,#1703,#1704,#1705,#1706,#1707,
#1708,#1709,#1710,#1711,#1712,#1713,#1714,#1715,#1716,#1717,#1718,#1719,
#1720,#1721,#1722,#1723,#1724,#1725,#1726,#1727,#1728,#1729,#1730,#1731,
#1732,#1733,#1734,#1735,#1736,#1737,#1738,#1739,#1740,#1741,#1742,#1743,
#1744,#1745,#1746,#1747,#1748,#1749,#1750,#1751,#1752,#1753,#1754,#1755,
#1756,#1757,#1758,#1759,#1760,#1761,#1762,#1763,#1764,#1765,#1766));
#421=EDGE_LOOP('',(#1767,#1768,#1769,#1770,#1771,#1772,#1773,#1774,#1775,
#1776,#1777,#1778,#1779,#1780,#1781,#1782,#1783,#1784,#1785,#1786,#1787,
#1788,#1789,#1790,#1791,#1792,#1793,#1794,#1795,#1796,#1797,#1798,#1799,
#1800,#1801,#1802,#1803,#1804,#1805,#1806,#1807,#1808,#1809,#1810,#1811,
#1812,#1813,#1814,#1815,#1816,#1817,#1818));
#422=EDGE_LOOP('',(#1819,#1820,#1821,#1822));
#423=EDGE_LOOP('',(#1823,#1824,#1825,#1826,#1827));
#424=EDGE_LOOP('',(#1828));
#425=EDGE_LOOP('',(#1829));
#426=EDGE_LOOP('',(#1830,#1831,#1832,#1833,#1834,#1835,#1836,#1837,#1838,
#1839,#1840,#1841,#1842,#1843,#1844,#1845,#1846,#1847,#1848,#1849,#1850,
#1851,#1852,#1853,#1854,#1855,#1856,#1857,#1858,#1859,#1860,#1861,#1862,
#1863,#1864,#1865,#1866,#1867,#1868,#1869,#1870,#1871,#1872,#1873,#1874,
#1875,#1876,#1877,#1878,#1879,#1880,#1881,#1882,#1883,#1884,#1885,#1886,
#1887,#1888,#1889,#1890,#1891,#1892,#1893,#1894,#1895,#1896));
#427=EDGE_LOOP('',(#1897,#1898,#1899,#1900,#1901,#1902,#1903,#1904,#1905,
#1906,#1907,#1908,#1909,#1910,#1911,#1912,#1913,#1914,#1915,#1916,#1917,
#1918,#1919,#1920,#1921,#1922,#1923,#1924,#1925,#1926,#1927,#1928,#1929,
#1930,#1931,#1932,#1933,#1934,#1935,#1936,#1937,#1938,#1939,#1940,#1941,
#1942,#1943,#1944,#1945,#1946,#1947,#1948,#1949,#1950,#1951,#1952,#1953,
#1954,#1955,#1956,#1957,#1958,#1959,#1960,#1961,#1962));
#428=EDGE_LOOP('',(#1963,#1964,#1965,#1966));
#429=EDGE_LOOP('',(#1967,#1968,#1969,#1970));
#430=EDGE_LOOP('',(#1971,#1972,#1973,#1974));
#431=EDGE_LOOP('',(#1975,#1976,#1977,#1978));
#432=EDGE_LOOP('',(#1979,#1980,#1981,#1982));
#433=EDGE_LOOP('',(#1983,#1984,#1985,#1986));
#434=EDGE_LOOP('',(#1987,#1988,#1989,#1990));
#435=EDGE_LOOP('',(#1991,#1992,#1993,#1994));
#436=EDGE_LOOP('',(#1995,#1996,#1997,#1998));
#437=EDGE_LOOP('',(#1999,#2000,#2001,#2002,#2003));
#438=EDGE_LOOP('',(#2004,#2005,#2006,#2007));
#439=EDGE_LOOP('',(#2008,#2009,#2010,#2011));
#440=EDGE_LOOP('',(#2012,#2013,#2014,#2015));
#441=EDGE_LOOP('',(#2016,#2017,#2018,#2019));
#442=EDGE_LOOP('',(#2020,#2021,#2022,#2023));
#443=EDGE_LOOP('',(#2024,#2025,#2026,#2027));
#444=EDGE_LOOP('',(#2028,#2029,#2030,#2031));
#445=EDGE_LOOP('',(#2032,#2033,#2034,#2035));
#446=EDGE_LOOP('',(#2036,#2037,#2038,#2039));
#447=EDGE_LOOP('',(#2040,#2041,#2042,#2043));
#448=EDGE_LOOP('',(#2044,#2045,#2046,#2047));
#449=EDGE_LOOP('',(#2048,#2049,#2050,#2051));
#450=EDGE_LOOP('',(#2052,#2053,#2054,#2055));
#451=EDGE_LOOP('',(#2056,#2057,#2058,#2059));
#452=EDGE_LOOP('',(#2060,#2061,#2062,#2063));
#453=EDGE_LOOP('',(#2064,#2065,#2066,#2067));
#454=EDGE_LOOP('',(#2068,#2069,#2070,#2071));
#455=EDGE_LOOP('',(#2072,#2073,#2074,#2075));
#456=EDGE_LOOP('',(#2076,#2077,#2078,#2079));
#457=EDGE_LOOP('',(#2080,#2081,#2082,#2083));
#458=EDGE_LOOP('',(#2084,#2085,#2086,#2087));
#459=EDGE_LOOP('',(#2088,#2089,#2090,#2091));
#460=EDGE_LOOP('',(#2092,#2093,#2094,#2095));
#461=EDGE_LOOP('',(#2096,#2097,#2098,#2099));
#462=EDGE_LOOP('',(#2100,#2101,#2102,#2103));
#463=EDGE_LOOP('',(#2104,#2105,#2106,#2107));
#464=EDGE_LOOP('',(#2108,#2109,#2110,#2111));
#465=EDGE_LOOP('',(#2112,#2113,#2114,#2115));
#466=EDGE_LOOP('',(#2116,#2117,#2118,#2119));
#467=EDGE_LOOP('',(#2120,#2121,#2122,#2123,#2124,#2125,#2126,#2127,#2128,
#2129,#2130,#2131,#2132,#2133,#2134,#2135,#2136,#2137,#2138,#2139,#2140,
#2141,#2142,#2143,#2144,#2145,#2146,#2147,#2148,#2149,#2150,#2151,#2152,
#2153,#2154,#2155,#2156,#2157,#2158,#2159,#2160,#2161,#2162,#2163,#2164,
#2165,#2166,#2167,#2168,#2169,#2170,#2171,#2172,#2173,#2174,#2175,#2176,
#2177,#2178,#2179,#2180,#2181,#2182,#2183,#2184,#2185,#2186,#2187,#2188,
#2189,#2190,#2191,#2192,#2193,#2194,#2195,#2196,#2197,#2198,#2199));
#468=EDGE_LOOP('',(#2200,#2201,#2202,#2203));
#469=EDGE_LOOP('',(#2204,#2205,#2206,#2207));
#470=EDGE_LOOP('',(#2208,#2209,#2210,#2211));
#471=EDGE_LOOP('',(#2212,#2213,#2214,#2215));
#472=EDGE_LOOP('',(#2216,#2217,#2218,#2219));
#473=EDGE_LOOP('',(#2220,#2221,#2222,#2223));
#474=EDGE_LOOP('',(#2224,#2225,#2226,#2227));
#475=EDGE_LOOP('',(#2228,#2229,#2230,#2231));
#476=EDGE_LOOP('',(#2232,#2233,#2234,#2235));
#477=EDGE_LOOP('',(#2236,#2237,#2238,#2239));
#478=EDGE_LOOP('',(#2240,#2241,#2242,#2243));
#479=EDGE_LOOP('',(#2244,#2245,#2246,#2247));
#480=EDGE_LOOP('',(#2248,#2249,#2250,#2251));
#481=EDGE_LOOP('',(#2252,#2253,#2254,#2255));
#482=EDGE_LOOP('',(#2256,#2257,#2258,#2259));
#483=EDGE_LOOP('',(#2260,#2261,#2262,#2263));
#484=EDGE_LOOP('',(#2264,#2265,#2266,#2267));
#485=EDGE_LOOP('',(#2268,#2269,#2270,#2271));
#486=EDGE_LOOP('',(#2272,#2273,#2274,#2275));
#487=EDGE_LOOP('',(#2276,#2277,#2278,#2279));
#488=EDGE_LOOP('',(#2280,#2281,#2282,#2283));
#489=EDGE_LOOP('',(#2284,#2285,#2286,#2287));
#490=EDGE_LOOP('',(#2288,#2289,#2290,#2291));
#491=EDGE_LOOP('',(#2292,#2293,#2294,#2295));
#492=EDGE_LOOP('',(#2296,#2297,#2298,#2299));
#493=EDGE_LOOP('',(#2300,#2301,#2302,#2303));
#494=EDGE_LOOP('',(#2304,#2305,#2306,#2307));
#495=EDGE_LOOP('',(#2308,#2309,#2310,#2311));
#496=EDGE_LOOP('',(#2312,#2313,#2314,#2315));
#497=EDGE_LOOP('',(#2316,#2317,#2318,#2319));
#498=EDGE_LOOP('',(#2320,#2321,#2322,#2323));
#499=EDGE_LOOP('',(#2324,#2325,#2326,#2327));
#500=EDGE_LOOP('',(#2328,#2329,#2330,#2331));
#501=EDGE_LOOP('',(#2332,#2333,#2334,#2335));
#502=EDGE_LOOP('',(#2336,#2337,#2338,#2339));
#503=EDGE_LOOP('',(#2340,#2341,#2342,#2343));
#504=EDGE_LOOP('',(#2344,#2345,#2346,#2347));
#505=EDGE_LOOP('',(#2348,#2349,#2350,#2351));
#506=EDGE_LOOP('',(#2352,#2353,#2354,#2355));
#507=EDGE_LOOP('',(#2356,#2357,#2358,#2359,#2360,#2361,#2362,#2363,#2364,
#2365,#2366,#2367,#2368,#2369,#2370,#2371,#2372,#2373,#2374,#2375,#2376,
#2377,#2378,#2379,#2380,#2381,#2382,#2383,#2384,#2385,#2386,#2387,#2388,
#2389,#2390,#2391,#2392,#2393,#2394,#2395,#2396,#2397,#2398,#2399,#2400,
#2401,#2402,#2403,#2404,#2405,#2406,#2407,#2408,#2409,#2410,#2411,#2412,
#2413,#2414,#2415,#2416,#2417,#2418,#2419,#2420,#2421,#2422,#2423,#2424,
#2425,#2426,#2427,#2428,#2429,#2430,#2431,#2432,#2433,#2434,#2435,#2436,
#2437,#2438,#2439,#2440));
#508=EDGE_LOOP('',(#2441,#2442,#2443,#2444));
#509=EDGE_LOOP('',(#2445,#2446,#2447,#2448));
#510=EDGE_LOOP('',(#2449));
#511=EDGE_LOOP('',(#2450,#2451,#2452,#2453,#2454));
#512=EDGE_LOOP('',(#2455,#2456,#2457,#2458));
#513=EDGE_LOOP('',(#2459,#2460,#2461,#2462));
#514=EDGE_LOOP('',(#2463,#2464,#2465,#2466));
#515=EDGE_LOOP('',(#2467,#2468,#2469,#2470));
#516=EDGE_LOOP('',(#2471,#2472,#2473,#2474,#2475));
#517=EDGE_LOOP('',(#2476,#2477,#2478,#2479,#2480,#2481));
#518=EDGE_LOOP('',(#2482,#2483,#2484,#2485,#2486,#2487));
#519=EDGE_LOOP('',(#2488,#2489,#2490,#2491,#2492,#2493));
#520=EDGE_LOOP('',(#2494,#2495,#2496,#2497,#2498));
#521=EDGE_LOOP('',(#2499,#2500,#2501,#2502));
#522=EDGE_LOOP('',(#2503,#2504,#2505,#2506));
#523=EDGE_LOOP('',(#2507,#2508,#2509,#2510));
#524=EDGE_LOOP('',(#2511,#2512,#2513,#2514,#2515));
#525=EDGE_LOOP('',(#2516,#2517,#2518,#2519,#2520,#2521));
#526=EDGE_LOOP('',(#2522,#2523,#2524,#2525,#2526,#2527));
#527=EDGE_LOOP('',(#2528,#2529,#2530,#2531,#2532,#2533));
#528=EDGE_LOOP('',(#2534,#2535,#2536,#2537,#2538));
#529=EDGE_LOOP('',(#2539,#2540,#2541,#2542));
#530=EDGE_LOOP('',(#2543));
#531=EDGE_LOOP('',(#2544));
#532=EDGE_LOOP('',(#2545,#2546,#2547,#2548));
#533=EDGE_LOOP('',(#2549,#2550,#2551,#2552));
#534=EDGE_LOOP('',(#2553,#2554,#2555,#2556,#2557,#2558,#2559,#2560,#2561,
#2562));
#535=EDGE_LOOP('',(#2563,#2564,#2565,#2566));
#536=EDGE_LOOP('',(#2567,#2568,#2569,#2570,#2571,#2572));
#537=EDGE_LOOP('',(#2573,#2574,#2575,#2576));
#538=EDGE_LOOP('',(#2577,#2578,#2579,#2580));
#539=EDGE_LOOP('',(#2581));
#540=EDGE_LOOP('',(#2582));
#541=EDGE_LOOP('',(#2583,#2584,#2585,#2586,#2587,#2588,#2589,#2590,#2591,
#2592));
#542=EDGE_LOOP('',(#2593));
#543=EDGE_LOOP('',(#2594));
#544=EDGE_LOOP('',(#2595,#2596,#2597,#2598));
#545=CIRCLE('',#2871,2.4505);
#546=CIRCLE('',#2872,2.4505);
#547=CIRCLE('',#2874,1.99475);
#548=CIRCLE('',#2875,1.99475);
#549=CIRCLE('',#2877,4.);
#550=CIRCLE('',#2878,4.);
#551=CIRCLE('',#2880,4.5);
#552=CIRCLE('',#2881,4.5);
#553=CIRCLE('',#2882,4.5);
#554=CIRCLE('',#2885,0.25);
#555=CIRCLE('',#2887,0.25);
#556=CIRCLE('',#2889,0.25);
#557=CIRCLE('',#2891,0.25);
#558=CIRCLE('',#2893,0.25);
#559=CIRCLE('',#2895,0.25);
#560=CIRCLE('',#2897,0.25);
#561=CIRCLE('',#2899,0.25);
#562=CIRCLE('',#2901,0.25);
#563=CIRCLE('',#2903,0.25);
#564=CIRCLE('',#2905,0.25);
#565=CIRCLE('',#2907,0.25);
#566=CIRCLE('',#2909,0.25);
#567=CIRCLE('',#2911,0.25);
#568=CIRCLE('',#2913,0.25);
#569=CIRCLE('',#2915,0.25);
#570=CIRCLE('',#2917,0.25);
#571=CIRCLE('',#2919,0.25);
#572=CIRCLE('',#2921,0.25);
#573=CIRCLE('',#2923,0.25);
#574=CIRCLE('',#2925,0.25);
#575=CIRCLE('',#2927,0.25);
#576=CIRCLE('',#2929,0.25);
#577=CIRCLE('',#2931,0.25);
#578=CIRCLE('',#2933,0.25);
#579=CIRCLE('',#2935,0.25);
#580=CIRCLE('',#2937,0.25);
#581=CIRCLE('',#2939,0.25);
#582=CIRCLE('',#2941,0.25);
#583=CIRCLE('',#2943,0.25);
#584=CIRCLE('',#2945,0.25);
#585=CIRCLE('',#2947,0.25);
#586=CIRCLE('',#2949,0.25);
#587=CIRCLE('',#2951,0.25);
#588=CIRCLE('',#2953,0.25);
#589=CIRCLE('',#2955,0.25);
#590=CIRCLE('',#2957,0.25);
#591=CIRCLE('',#2959,0.25);
#592=CIRCLE('',#2961,0.25);
#593=CIRCLE('',#2963,5.5);
#594=CIRCLE('',#2964,5.5);
#595=CIRCLE('',#2965,5.5);
#596=CIRCLE('',#2966,5.5);
#597=CIRCLE('',#2967,5.5);
#598=CIRCLE('',#2968,5.5);
#599=CIRCLE('',#2969,5.5);
#600=CIRCLE('',#2970,5.5);
#601=CIRCLE('',#2971,5.5);
#602=CIRCLE('',#2972,5.5);
#603=CIRCLE('',#2973,5.5);
#604=CIRCLE('',#2974,5.5);
#605=CIRCLE('',#2975,5.5);
#606=CIRCLE('',#2976,5.5);
#607=CIRCLE('',#2977,5.5);
#608=CIRCLE('',#2978,5.5);
#609=CIRCLE('',#2979,5.5);
#610=CIRCLE('',#2980,5.5);
#611=CIRCLE('',#2981,5.5);
#612=CIRCLE('',#2982,5.5);
#613=CIRCLE('',#2983,5.5);
#614=CIRCLE('',#2984,5.5);
#615=CIRCLE('',#2985,5.5);
#616=CIRCLE('',#2986,5.5);
#617=CIRCLE('',#2987,5.5);
#618=CIRCLE('',#2988,5.5);
#619=CIRCLE('',#2989,5.5);
#620=CIRCLE('',#2990,5.5);
#621=CIRCLE('',#2991,5.5);
#622=CIRCLE('',#2992,5.5);
#623=CIRCLE('',#2993,5.5);
#624=CIRCLE('',#2994,5.5);
#625=CIRCLE('',#2995,5.5);
#626=CIRCLE('',#2996,5.5);
#627=CIRCLE('',#2997,5.5);
#628=CIRCLE('',#2998,5.5);
#629=CIRCLE('',#2999,5.5);
#630=CIRCLE('',#3000,5.5);
#631=CIRCLE('',#3001,5.5);
#632=CIRCLE('',#3002,0.25);
#633=CIRCLE('',#3003,5.5);
#634=CIRCLE('',#3005,5.5);
#635=CIRCLE('',#3007,5.5);
#636=CIRCLE('',#3009,5.5);
#637=CIRCLE('',#3011,5.5);
#638=CIRCLE('',#3013,5.5);
#639=CIRCLE('',#3015,5.5);
#640=CIRCLE('',#3017,5.5);
#641=CIRCLE('',#3019,5.5);
#642=CIRCLE('',#3021,5.5);
#643=CIRCLE('',#3023,5.5);
#644=CIRCLE('',#3025,5.5);
#645=CIRCLE('',#3027,5.5);
#646=CIRCLE('',#3029,5.5);
#647=CIRCLE('',#3031,5.5);
#648=CIRCLE('',#3033,5.5);
#649=CIRCLE('',#3035,5.5);
#650=CIRCLE('',#3037,5.5);
#651=CIRCLE('',#3039,5.5);
#652=CIRCLE('',#3041,5.5);
#653=CIRCLE('',#3043,5.5);
#654=CIRCLE('',#3045,5.5);
#655=CIRCLE('',#3047,5.5);
#656=CIRCLE('',#3049,5.5);
#657=CIRCLE('',#3051,5.5);
#658=CIRCLE('',#3053,5.5);
#659=CIRCLE('',#3055,5.5);
#660=CIRCLE('',#3057,5.5);
#661=CIRCLE('',#3059,5.5);
#662=CIRCLE('',#3061,5.5);
#663=CIRCLE('',#3063,5.5);
#664=CIRCLE('',#3065,5.5);
#665=CIRCLE('',#3067,5.5);
#666=CIRCLE('',#3069,5.5);
#667=CIRCLE('',#3071,5.5);
#668=CIRCLE('',#3073,5.5);
#669=CIRCLE('',#3075,5.5);
#670=CIRCLE('',#3077,5.5);
#671=CIRCLE('',#3079,5.5);
#672=CIRCLE('',#3081,5.5);
#673=CIRCLE('',#3083,1.);
#674=CIRCLE('',#3084,5.5);
#675=CIRCLE('',#3091,17.0820002071033);
#676=CIRCLE('',#3092,14.8491923750145);
#677=CIRCLE('',#3094,16.7952119889278);
#678=CIRCLE('',#3095,0.25);
#679=CIRCLE('',#3097,14.542543867133);
#680=CIRCLE('',#3099,12.2837868382051);
#681=CIRCLE('',#3100,12.2837868382051);
#682=CIRCLE('',#3101,1.72390117308562);
#683=CIRCLE('',#3103,12.0671767507335);
#684=CIRCLE('',#3104,12.0671767507335);
#685=CIRCLE('',#3106,2.22390117308562);
#686=CIRCLE('',#3109,17.0820002071033);
#687=CIRCLE('',#3110,14.8491923750145);
#688=CIRCLE('',#3112,16.7952119889278);
#689=CIRCLE('',#3113,0.25);
#690=CIRCLE('',#3115,14.542543867133);
#691=CIRCLE('',#3117,12.2837868382051);
#692=CIRCLE('',#3118,12.2837868382051);
#693=CIRCLE('',#3119,1.72390117308562);
#694=CIRCLE('',#3121,12.0671767507335);
#695=CIRCLE('',#3122,12.0671767507335);
#696=CIRCLE('',#3124,2.22390117308562);
#697=CIRCLE('',#3132,3.43);
#698=CIRCLE('',#3138,3.43);
#699=CIRCLE('',#3139,1.666);
#700=CIRCLE('',#3142,1.666);
#701=B_SPLINE_CURVE_WITH_KNOTS('',3,(#3813,#3814,#3815,#3816,#3817,#3818),
 .UNSPECIFIED.,.F.,.F.,(4,1,1,4),(-4.09157007060746,-3.994723473443,-2.99604260508226,
-2.0669567652117),.UNSPECIFIED.);
#702=B_SPLINE_CURVE_WITH_KNOTS('',3,(#3822,#3823,#3824,#3825,#3826,#3827,
#3828,#3829,#3830,#3831,#3832,#3833,#3834,#3835,#3836,#3837,#3838,#3839,
#3840,#3841,#3842,#3843,#3844,#3845,#3846,#3847,#3848,#3849,#3850,#3851,
#3852,#3853,#3854,#3855),.UNSPECIFIED.,.F.,.F.,(4,3,3,3,3,3,3,3,3,3,3,4),
(0.,0.102023156236483,0.203984576046395,0.30593583891409,0.407884768424913,
0.50985600275984,0.611874198231225,0.714044517939152,0.816293156139123,
0.918743873970227,0.998680868360744,1.11662023360707),.UNSPECIFIED.);
#703=B_SPLINE_CURVE_WITH_KNOTS('',3,(#3857,#3858,#3859,#3860,#3861,#3862,
#3863,#3864,#3865,#3866,#3867,#3868,#3869,#3870,#3871,#3872,#3873,#3874,
#3875,#3876,#3877,#3878,#3879,#3880,#3881,#3882,#3883,#3884,#3885,#3886,
#3887,#3888,#3889,#3890,#3891,#3892,#3893,#3894,#3895,#3896,#3897,#3898,
#3899,#3900,#3901,#3902,#3903,#3904,#3905,#3906,#3907,#3908,#3909,#3910,
#3911,#3912,#3913,#3914,#3915,#3916,#3917,#3918,#3919,#3920,#3921,#3922,
#3923,#3924,#3925,#3926,#3927,#3928,#3929,#3930,#3931,#3932,#3933,#3934,
#3935,#3936,#3937,#3938,#3939,#3940,#3941,#3942,#3943,#3944,#3945,#3946,
#3947,#3948,#3949,#3950,#3951,#3952,#3953,#3954,#3955,#3956,#3957,#3958,
#3959,#3960,#3961,#3962,#3963,#3964,#3965,#3966,#3967,#3968,#3969,#3970,
#3971,#3972,#3973,#3974,#3975,#3976,#3977,#3978,#3979,#3980,#3981,#3982,
#3983,#3984,#3985,#3986,#3987,#3988,#3989,#3990,#3991,#3992,#3993,#3994,
#3995,#3996,#3997,#3998,#3999,#4000,#4001,#4002,#4003,#4004,#4005,#4006,
#4007,#4008,#4009,#4010,#4011,#4012,#4013,#4014,#4015,#4016,#4017,#4018,
#4019,#4020,#4021,#4022,#4023,#4024,#4025,#4026,#4027,#4028,#4029,#4030,
#4031,#4032,#4033,#4034,#4035,#4036,#4037,#4038,#4039,#4040,#4041,#4042,
#4043,#4044,#4045,#4046),.UNSPECIFIED.,.F.,.F.,(4,3,3,3,3,3,3,3,3,3,3,3,
3,3,3,3,3,3,3,3,3,3,3,3,3,3,3,3,3,3,3,3,3,3,3,3,3,3,3,3,3,3,3,3,3,3,3,3,
3,3,3,3,3,3,3,3,3,3,3,3,3,3,3,4),(1.11662023381331,1.21393749512102,1.31186552532108,
1.40895568848407,1.50599774867716,1.60302436386015,1.70160870707549,1.79876006485995,
1.89806090079072,1.9973617367215,2.0971951147542,2.19688541258594,2.29678006164798,
2.39628986921115,2.49576606614439,2.59523889921085,2.6954398256787,2.79505356449904,
2.89554808479064,2.99604260508225,3.09590085771483,3.19561947633777,3.29550747597593,
3.39505385307093,3.4945696602538,3.59408510451255,3.69424469674516,3.79390804450808,
3.89431575897554,3.994723473443,4.09427171410558,4.19367485294064,4.29364103904853,
4.39286092752618,4.49204682472469,4.59122937758233,4.69177311863769,4.79109962130981,
4.89225198155678,4.99340434180375,5.09311693288323,5.19268643289398,5.29261128005279,
5.39200122521914,5.49135819719149,5.59071261738691,5.6910557655813,5.7905543529646,
5.89131978156455,5.9920852101645,6.0917896034481,6.19135123448222,6.2912780899876,
6.39066103446566,6.49001135007882,6.58935946901391,6.68971112139174,6.78920435337002,
6.88998521594764,6.99076607852525,7.10075815164408,7.21042743348155,7.31954741556262,
7.3998051206394),.UNSPECIFIED.);
#704=B_SPLINE_CURVE_WITH_KNOTS('',3,(#4048,#4049,#4050,#4051,#4052,#4053,
#4054,#4055,#4056,#4057),.UNSPECIFIED.,.F.,.F.,(4,1,1,1,1,1,1,4),(7.39980554078666,
7.98944694688601,8.98812781524676,9.98680868360752,10.9854895519683,11.984170420329,
12.9828512886898,13.6829908479662),.UNSPECIFIED.);
#705=B_SPLINE_CURVE_WITH_KNOTS('',3,(#4059,#4060,#4061,#4062,#4063,#4064,
#4065,#4066,#4067,#4068,#4069,#4070,#4071,#4072,#4073,#4074,#4075,#4076,
#4077,#4078,#4079,#4080,#4081,#4082,#4083,#4084,#4085,#4086,#4087,#4088,
#4089,#4090,#4091,#4092,#4093,#4094,#4095,#4096,#4097,#4098,#4099,#4100,
#4101,#4102,#4103,#4104,#4105,#4106,#4107,#4108,#4109,#4110,#4111,#4112,
#4113,#4114,#4115,#4116,#4117,#4118,#4119,#4120,#4121,#4122,#4123,#4124,
#4125,#4126,#4127,#4128,#4129,#4130,#4131,#4132,#4133,#4134,#4135,#4136,
#4137,#4138,#4139,#4140,#4141,#4142,#4143,#4144,#4145,#4146,#4147,#4148,
#4149,#4150,#4151,#4152,#4153,#4154,#4155,#4156,#4157,#4158,#4159,#4160,
#4161,#4162,#4163,#4164,#4165,#4166,#4167,#4168,#4169,#4170,#4171,#4172,
#4173,#4174,#4175,#4176,#4177,#4178,#4179,#4180,#4181,#4182,#4183,#4184,
#4185,#4186,#4187,#4188,#4189,#4190,#4191,#4192,#4193,#4194,#4195,#4196,
#4197,#4198,#4199,#4200,#4201,#4202,#4203,#4204,#4205,#4206,#4207,#4208,
#4209,#4210,#4211,#4212,#4213,#4214,#4215,#4216,#4217,#4218,#4219,#4220,
#4221,#4222,#4223,#4224,#4225,#4226,#4227,#4228,#4229,#4230,#4231,#4232,
#4233,#4234,#4235,#4236,#4237,#4238,#4239,#4240,#4241,#4242,#4243,#4244,
#4245,#4246,#4247,#4248),.UNSPECIFIED.,.F.,.F.,(4,3,3,3,3,3,3,3,3,3,3,3,
3,3,3,3,3,3,3,3,3,3,3,3,3,3,3,3,3,3,3,3,3,3,3,3,3,3,3,3,3,3,3,3,3,3,3,3,
3,3,3,3,3,3,3,3,3,3,3,3,3,3,3,4),(13.6829910273321,13.8027886851572,13.9242775395078,
13.9815321570505,14.0812158855861,14.1807563980189,14.2806884764429,14.3800493486247,
14.4793772813362,14.5787027361138,14.6790803084382,14.7785504119759,14.8793817186936,
14.9802130254113,15.0798966080951,15.1794369736886,15.279369088699,15.3787298127342,
15.4780575971396,15.5773829036542,15.6777606511837,15.7772306080887,15.8780622509303,
15.978893893772,16.0785774056108,16.1781176986771,16.2780498316091,16.3774104795357,
16.4767381866505,16.5760634147927,16.6764412516277,16.7759111282822,16.8767429452075,
16.9775747621328,17.0772583543262,17.176798728974,17.2767308416639,17.3760915735656,
17.4754193653706,17.5747446788055,17.6751224167275,17.7745923792929,17.8754240048932,
17.9762556304935,18.07593919654,18.1754795448068,18.2754116640627,18.3747723692092,
18.4741001341781,18.5734254207322,18.6738031902627,18.7732731261129,18.8741048124836,
18.9749364988543,19.0744883959638,19.1738971727394,19.2731905896819,19.3724208663801,
19.471618683102,19.570814680118,19.6701088383941,19.7694498169088,19.8689715645658,
19.9661761551458),.UNSPECIFIED.);
#706=B_SPLINE_CURVE_WITH_KNOTS('',3,(#4250,#4251,#4252,#4253,#4254,#4255,
#4256,#4257,#4258,#4259,#4260,#4261),.UNSPECIFIED.,.F.,.F.,(4,2,1,1,1,1,
1,1,4),(19.9661761551458,19.973617367215,20.9722982355758,21.9709791039365,
22.9696599722973,23.968340840658,24.9670217090188,25.9657025773795,26.2493568946854),
 .UNSPECIFIED.);
#707=B_SPLINE_CURVE_WITH_KNOTS('',3,(#4263,#4264,#4265,#4266,#4267,#4268,
#4269,#4270,#4271,#4272,#4273,#4274,#4275,#4276,#4277,#4278,#4279,#4280,
#4281,#4282,#4283,#4284,#4285,#4286,#4287,#4288,#4289,#4290,#4291,#4292,
#4293,#4294,#4295,#4296,#4297,#4298,#4299,#4300,#4301,#4302,#4303,#4304,
#4305,#4306,#4307,#4308,#4309,#4310,#4311,#4312,#4313,#4314,#4315,#4316,
#4317,#4318,#4319,#4320,#4321,#4322,#4323,#4324,#4325,#4326,#4327,#4328,
#4329,#4330,#4331,#4332,#4333,#4334,#4335,#4336,#4337,#4338,#4339,#4340,
#4341,#4342,#4343,#4344,#4345,#4346,#4347,#4348,#4349,#4350,#4351,#4352,
#4353,#4354,#4355,#4356,#4357,#4358,#4359,#4360,#4361,#4362,#4363,#4364,
#4365,#4366,#4367,#4368,#4369,#4370,#4371,#4372,#4373,#4374,#4375,#4376,
#4377,#4378,#4379,#4380,#4381,#4382,#4383,#4384,#4385,#4386,#4387,#4388,
#4389,#4390,#4391,#4392,#4393,#4394,#4395,#4396,#4397,#4398,#4399,#4400,
#4401,#4402,#4403,#4404,#4405,#4406,#4407,#4408,#4409,#4410,#4411,#4412,
#4413,#4414,#4415,#4416,#4417,#4418,#4419,#4420,#4421,#4422,#4423,#4424,
#4425,#4426,#4427,#4428,#4429,#4430,#4431,#4432,#4433,#4434,#4435,#4436,
#4437,#4438,#4439,#4440,#4441,#4442,#4443,#4444,#4445,#4446,#4447,#4448,
#4449,#4450,#4451,#4452,#4453,#4454,#4455),.UNSPECIFIED.,.F.,.F.,(4,3,3,
3,3,3,3,3,3,3,3,3,3,3,3,3,3,3,3,3,3,3,3,3,3,3,3,3,3,3,3,3,3,3,3,3,3,3,3,
3,3,3,3,3,3,3,3,3,3,3,3,3,3,3,3,3,3,3,3,3,3,3,3,3,4),(26.2493614623254,
26.3479492131184,26.4464925326639,26.545022844986,26.6435715522213,26.7422307023355,
26.8409562100383,26.9398413203745,26.9643834457403,27.0640670117324,27.1636073598688,
27.2635394791478,27.3629001839775,27.4622279485599,27.5615532346581,27.6619310045188,
27.7614009397454,27.8622326269232,27.963064314101,28.0627478801,28.162288228243,
28.2622203475203,28.3615810523563,28.4609088169447,28.5602341030488,28.6606118729021,
28.7600818081338,28.8609134952978,28.9617451824618,29.061428748488,29.1609690966589,
29.2609012159294,29.3602619207941,29.4595896854117,29.5589149715449,29.6592927413643,
29.7587626766259,29.8595943637242,29.9604260508225,30.0601096168314,30.1596499649844,
30.2595820842593,30.3589427891061,30.4582705537053,30.5575958398202,30.657973609661,
30.7574435449042,30.8582752320438,30.9591069191833,31.0587904851944,31.1583308333497,
31.258262952624,31.357623657473,31.4569514220748,31.5562767081925,31.6566544780304,
31.7561244132758,31.8569561004099,31.957787787544,32.0596638740538,32.1613737804538,
32.2629105875756,32.3643455803479,32.4656954588227,32.532546769505),
 .UNSPECIFIED.);
#708=B_SPLINE_CURVE_WITH_KNOTS('',3,(#4457,#4458,#4459,#4460,#4461,#4462,
#4463,#4464,#4465,#4466),.UNSPECIFIED.,.F.,.F.,(4,1,1,1,1,1,1,4),(32.5325523549555,
32.9564686559048,33.9551495242656,34.9538303926263,35.9525112609871,36.9511921293478,
37.9498729977086,38.8157320766846),.UNSPECIFIED.);
#709=B_SPLINE_CURVE_WITH_KNOTS('',3,(#4468,#4469,#4470,#4471,#4472,#4473,
#4474,#4475,#4476,#4477,#4478),.UNSPECIFIED.,.F.,.F.,(4,1,1,1,1,1,1,1,4),
(38.8157320766846,38.9485538660693,39.9472347344301,40.9459156027908,41.9445964711516,
42.9432773395123,43.9419582078731,44.9406390762338,45.0989173838642),
 .UNSPECIFIED.);
#710=B_SPLINE_CURVE_WITH_KNOTS('',3,(#4480,#4481,#4482,#4483,#4484,#4485,
#4486,#4487,#4488,#4489),.UNSPECIFIED.,.F.,.F.,(4,1,1,1,1,1,1,4),(45.0989173838642,
45.9393199445946,46.9380008129553,47.9366816813161,48.9353625496768,49.9340434180376,
50.9327242863983,51.3821026910438),.UNSPECIFIED.);
#711=B_SPLINE_CURVE_WITH_KNOTS('',3,(#4491,#4492,#4493,#4494,#4495,#4496,
#4497,#4498,#4499,#4500),.UNSPECIFIED.,.F.,.F.,(4,1,1,1,1,1,1,4),(51.3821026910438,
51.9314051547591,52.9300860231198,53.9287668914806,54.9274477598413,55.9261286282021,
56.9248094965628,57.6652879982234),.UNSPECIFIED.);
#712=B_SPLINE_CURVE_WITH_KNOTS('',3,(#4502,#4503,#4504,#4505,#4506,#4507,
#4508,#4509,#4510,#4511,#4512,#4513,#4514,#4515,#4516,#4517,#4518,#4519,
#4520,#4521,#4522,#4523,#4524,#4525,#4526,#4527,#4528,#4529,#4530,#4531,
#4532,#4533,#4534,#4535,#4536,#4537,#4538,#4539,#4540,#4541,#4542,#4543,
#4544,#4545,#4546,#4547,#4548,#4549,#4550,#4551,#4552,#4553,#4554,#4555,
#4556,#4557,#4558,#4559,#4560,#4561,#4562,#4563,#4564,#4565,#4566,#4567,
#4568,#4569,#4570,#4571,#4572,#4573,#4574,#4575,#4576,#4577,#4578,#4579,
#4580,#4581,#4582,#4583,#4584,#4585,#4586,#4587,#4588,#4589,#4590,#4591,
#4592,#4593,#4594,#4595,#4596,#4597,#4598,#4599,#4600,#4601,#4602,#4603,
#4604,#4605,#4606,#4607,#4608,#4609,#4610,#4611,#4612,#4613,#4614,#4615,
#4616,#4617,#4618,#4619,#4620,#4621,#4622,#4623,#4624,#4625,#4626,#4627,
#4628,#4629,#4630,#4631,#4632,#4633,#4634,#4635,#4636,#4637,#4638,#4639,
#4640,#4641,#4642,#4643,#4644,#4645,#4646,#4647,#4648,#4649,#4650,#4651,
#4652,#4653,#4654,#4655,#4656,#4657,#4658,#4659,#4660,#4661,#4662,#4663,
#4664,#4665,#4666,#4667,#4668,#4669,#4670,#4671,#4672,#4673,#4674,#4675,
#4676,#4677,#4678,#4679,#4680,#4681,#4682,#4683,#4684,#4685,#4686,#4687,
#4688,#4689,#4690,#4691),.UNSPECIFIED.,.F.,.F.,(4,3,3,3,3,3,3,3,3,3,3,3,
3,3,3,3,3,3,3,3,3,3,3,3,3,3,3,3,3,3,3,3,3,3,3,3,3,3,3,3,3,3,3,3,3,3,3,3,
3,3,3,3,3,3,3,3,3,3,3,3,3,3,3,4),(57.6652881545519,57.7943892597378,57.9234903649236,
58.0231739309364,58.1227142790933,58.2226463983672,58.3220071032179,58.4213348678212,
58.5206601539402,58.6210379237762,58.7205078590233,58.8213395461538,58.9221712332843,
59.0218547992971,59.1213951474542,59.221327266728,59.3206879715787,59.420015736182,
59.5193410223011,59.6197187921371,59.7191887273842,59.8200204145147,59.9208521016451,
60.0205356676579,60.1200760158151,60.2200081350889,60.3193688399396,60.418696604543,
60.5180218906621,60.618399660498,60.7178695957452,60.8187012828756,60.9195329700059,
61.0192165360187,61.1187568841757,61.2186890034496,61.3180497083003,61.4173774729035,
61.5167027590226,61.6170805288586,61.7165504641057,61.8173821512361,61.9182138383666,
62.0178974043794,62.1174377525365,62.2173698718104,62.316730576661,62.4160583412643,
62.5153836273834,62.6157613972194,62.7152313324666,62.816063019597,62.9168947067274,
63.0165782727402,63.1161186208972,63.2160507401711,63.3154114450218,63.4147392096251,
63.5140644957442,63.6144422655802,63.7139122008273,63.8147438879577,63.9155755750881,
63.948473305403),.UNSPECIFIED.);
#713=B_SPLINE_CURVE_WITH_KNOTS('',3,(#4693,#4694,#4695,#4696,#4697,#4698,
#4699,#4700,#4701,#4702),.UNSPECIFIED.,.F.,.F.,(4,1,1,1,1,1,1,4),(63.9484777838044,
64.9142564434489,65.9129373118096,66.9116181801704,67.9102990485311,68.9089799168918,
69.9076607852526,70.2316517155),.UNSPECIFIED.);
#714=B_SPLINE_CURVE_WITH_KNOTS('',3,(#4704,#4705,#4706,#4707,#4708,#4709,
#4710,#4711,#4712,#4713,#4714,#4715,#4716,#4717,#4718,#4719,#4720,#4721,
#4722,#4723,#4724,#4725,#4726,#4727,#4728,#4729,#4730,#4731,#4732,#4733,
#4734,#4735,#4736,#4737,#4738,#4739,#4740,#4741,#4742,#4743,#4744,#4745,
#4746,#4747,#4748,#4749,#4750,#4751,#4752,#4753,#4754,#4755,#4756,#4757,
#4758,#4759,#4760,#4761,#4762,#4763,#4764,#4765,#4766,#4767,#4768,#4769,
#4770,#4771,#4772,#4773,#4774,#4775,#4776,#4777,#4778,#4779,#4780,#4781,
#4782,#4783,#4784,#4785,#4786,#4787,#4788,#4789,#4790,#4791,#4792,#4793,
#4794,#4795,#4796,#4797,#4798,#4799,#4800,#4801,#4802,#4803,#4804,#4805,
#4806,#4807,#4808,#4809,#4810,#4811,#4812,#4813,#4814,#4815,#4816,#4817,
#4818,#4819,#4820,#4821,#4822,#4823,#4824,#4825,#4826,#4827,#4828,#4829,
#4830,#4831,#4832,#4833,#4834,#4835,#4836,#4837,#4838,#4839,#4840,#4841,
#4842,#4843,#4844,#4845,#4846,#4847,#4848,#4849,#4850,#4851,#4852,#4853,
#4854,#4855,#4856,#4857,#4858,#4859,#4860,#4861,#4862,#4863,#4864,#4865,
#4866,#4867,#4868,#4869,#4870,#4871,#4872,#4873,#4874,#4875,#4876,#4877,
#4878,#4879,#4880,#4881,#4882,#4883,#4884,#4885,#4886,#4887,#4888,#4889,
#4890,#4891,#4892,#4893),.UNSPECIFIED.,.F.,.F.,(4,3,3,3,3,3,3,3,3,3,3,3,
3,3,3,3,3,3,3,3,3,3,3,3,3,3,3,3,3,3,3,3,3,3,3,3,3,3,3,3,3,3,3,3,3,3,3,3,
3,3,3,3,3,3,3,3,3,3,3,3,3,3,3,4),(70.2316586125826,70.3307800166858,70.4298793745695,
70.5289873506871,70.6282047037803,70.7274781134284,70.8269336412923,70.9063416536133,
71.0060252196261,71.1055655677834,71.2054976870572,71.3048583919079,71.4041861565112,
71.5035114426302,71.6038892124662,71.7033591477134,71.8041908348438,71.9050225219741,
72.0047060879869,72.1042464361441,72.2041785554179,72.3035392602686,72.402867024872,
72.5021923109908,72.6025700808268,72.702040016074,72.8028717032045,72.9037033903349,
73.0033869563477,73.1029273045047,73.2028594237785,73.3022201286292,73.4015478932325,
73.5008731793516,73.6012509491876,73.7007208844348,73.8015525715652,73.9023842586956,
74.0020678247084,74.1016081728656,74.2015402921394,74.3009009969901,74.4002287615935,
74.4995540477125,74.5999318175485,74.6994017527956,74.800233439926,74.9010651270564,
75.0007486930691,75.1002890412263,75.2002211605002,75.299581865351,75.3989096299542,
75.4982349160732,75.5986126859092,75.6980826211565,75.7989143082868,75.8997459954171,
76.000471352571,76.1010449027966,76.204494657038,76.3048389751224,76.4098414474423,
76.5148439197622),.UNSPECIFIED.);
#715=B_SPLINE_CURVE_WITH_KNOTS('',3,(#4895,#4896,#4897,#4898,#4899,#4900,
#4901,#4902,#4903,#4904),.UNSPECIFIED.,.F.,.F.,(4,1,1,1,1,1,1,4),(76.5148513200435,
76.8984268637779,77.8971077321387,78.8957886004994,79.8944694688601,80.8931503372209,
81.8918312055816,82.7980204291147),.UNSPECIFIED.);
#716=B_SPLINE_CURVE_WITH_KNOTS('',3,(#4906,#4907,#4908,#4909,#4910,#4911,
#4912,#4913,#4914,#4915,#4916,#4917,#4918,#4919,#4920,#4921,#4922,#4923,
#4924,#4925,#4926,#4927,#4928,#4929,#4930,#4931,#4932,#4933,#4934,#4935,
#4936,#4937,#4938,#4939,#4940,#4941,#4942,#4943,#4944,#4945,#4946,#4947,
#4948,#4949,#4950,#4951,#4952,#4953,#4954,#4955,#4956,#4957,#4958,#4959,
#4960,#4961,#4962,#4963,#4964,#4965,#4966,#4967,#4968,#4969,#4970,#4971,
#4972,#4973,#4974,#4975,#4976,#4977,#4978,#4979,#4980,#4981,#4982,#4983,
#4984,#4985,#4986,#4987,#4988,#4989,#4990,#4991,#4992,#4993,#4994,#4995,
#4996,#4997,#4998,#4999,#5000,#5001,#5002,#5003,#5004,#5005,#5006,#5007,
#5008,#5009,#5010,#5011,#5012,#5013,#5014,#5015,#5016,#5017,#5018,#5019,
#5020,#5021,#5022,#5023,#5024,#5025,#5026,#5027,#5028,#5029,#5030,#5031,
#5032,#5033,#5034,#5035,#5036,#5037,#5038,#5039,#5040,#5041,#5042,#5043,
#5044,#5045,#5046,#5047,#5048,#5049,#5050,#5051,#5052,#5053,#5054,#5055,
#5056,#5057,#5058,#5059,#5060,#5061,#5062,#5063,#5064,#5065,#5066,#5067,
#5068,#5069,#5070,#5071,#5072,#5073,#5074,#5075,#5076,#5077,#5078,#5079,
#5080,#5081,#5082,#5083,#5084,#5085,#5086,#5087,#5088,#5089,#5090,#5091,
#5092,#5093,#5094,#5095),.UNSPECIFIED.,.F.,.F.,(4,3,3,3,3,3,3,3,3,3,3,3,
3,3,3,3,3,3,3,3,3,3,3,3,3,3,3,3,3,3,3,3,3,3,3,3,3,3,3,3,3,3,3,3,3,3,3,3,
3,3,3,3,3,3,3,3,3,3,3,3,3,3,3,4),(82.7980292269418,82.8905120739424,82.9901956399552,
83.0897359881124,83.1896681073862,83.2890288122369,83.3883565768402,83.4876818629593,
83.5880596327953,83.6875295680425,83.7883612551728,83.8891929423031,83.9888765083159,
84.088416856473,84.1883489757469,84.2877096805976,84.3870374452009,84.48636273132,
84.586740501156,84.6862104364031,84.7870421235335,84.8878738106639,84.9875573766767,
85.0870977248337,85.1870298441076,85.2863905489582,85.3857183135615,85.4850435996806,
85.5854213695166,85.6848913047637,85.7857229918941,85.8865546790246,85.9862382450374,
86.0857785931945,86.1857107124683,86.285071417319,86.3843991819223,86.4837244680414,
86.5841022378774,86.6835721731245,86.784403860255,86.8852355473854,86.9849191133982,
87.0844594615553,87.1843915808292,87.2837522856799,87.3830800502832,87.4824053364024,
87.5827831062383,87.6822530414855,87.7830847286158,87.8839164157462,87.983599981759,
88.083140329916,88.1830724491899,88.2824331540406,88.3817609186438,88.4810862047629,
88.5814639745989,88.680933909846,88.7817655969764,88.8825972841069,89.0259343107751,
89.0812145341213),.UNSPECIFIED.);
#717=B_SPLINE_CURVE_WITH_KNOTS('',3,(#5097,#5098,#5099,#5100,#5101,#5102,
#5103,#5104,#5105,#5106,#5107,#5108,#5109,#5110,#5111,#5112,#5113,#5114,
#5115,#5116,#5117,#5118,#5119,#5120,#5121,#5122,#5123,#5124,#5125,#5126,
#5127,#5128,#5129,#5130,#5131,#5132,#5133,#5134,#5135,#5136,#5137,#5138,
#5139,#5140,#5141,#5142,#5143,#5144,#5145,#5146,#5147,#5148,#5149,#5150,
#5151,#5152,#5153,#5154,#5155,#5156,#5157,#5158,#5159,#5160,#5161,#5162,
#5163,#5164,#5165,#5166,#5167,#5168,#5169,#5170,#5171,#5172,#5173,#5174,
#5175,#5176,#5177,#5178,#5179,#5180,#5181,#5182,#5183,#5184,#5185,#5186,
#5187,#5188,#5189,#5190,#5191,#5192,#5193,#5194,#5195,#5196,#5197,#5198,
#5199,#5200,#5201,#5202,#5203,#5204,#5205,#5206,#5207,#5208,#5209,#5210,
#5211,#5212,#5213,#5214,#5215,#5216,#5217,#5218,#5219,#5220,#5221,#5222,
#5223,#5224,#5225,#5226,#5227,#5228,#5229,#5230,#5231,#5232,#5233,#5234,
#5235,#5236,#5237,#5238,#5239,#5240,#5241,#5242,#5243,#5244,#5245,#5246,
#5247,#5248,#5249,#5250,#5251,#5252,#5253,#5254,#5255,#5256,#5257,#5258,
#5259,#5260,#5261,#5262,#5263,#5264,#5265,#5266,#5267,#5268,#5269,#5270,
#5271,#5272,#5273,#5274,#5275,#5276,#5277,#5278,#5279,#5280,#5281,#5282,
#5283,#5284,#5285,#5286,#5287,#5288,#5289),.UNSPECIFIED.,.F.,.F.,(4,3,3,
3,3,3,3,3,3,3,3,3,3,3,3,3,3,3,3,3,3,3,3,3,3,3,3,3,3,3,3,3,3,3,3,3,3,3,3,
3,3,3,3,3,3,3,3,3,3,3,3,3,3,3,3,3,3,3,3,3,3,3,3,3,4),(89.0812145344659,
89.1812224867161,89.2791888648667,89.3771066451239,89.4750078977673,89.5765754614424,
89.6745991542258,89.7726889754984,89.8709299133438,89.8812781524677,89.9809617184804,
90.0805020666376,90.1804341859115,90.2797948907621,90.3791226553653,90.4784479414842,
90.5788257113202,90.6782956465674,90.7791273336979,90.8799590208284,90.9796425868411,
91.0791829349983,91.1791150542722,91.2784757591229,91.3778035237263,91.4771288098453,
91.5775065796813,91.6769765149286,91.7778082020589,91.8786398891892,91.978323455202,
92.0778638033592,92.1777959226331,92.2771566274838,92.376484392087,92.4758096782061,
92.5761874480421,92.6756573832893,92.7764890704196,92.8773207575499,92.9770043235627,
93.07654467172,93.1764767909939,93.2758374958446,93.3751652604479,93.4744905465672,
93.574868316403,93.6743382516501,93.7751699387804,93.8760016259107,93.9756851919234,
94.0752255400803,94.1751576593542,94.274518364205,94.3738461288083,94.4731714149275,
94.5735491847635,94.6730191200106,94.773850807141,94.8746824942714,94.9799562416788,
95.0849191111029,95.1896943939098,95.2942224671571,95.3643998410932),
 .UNSPECIFIED.);
#718=B_SPLINE_CURVE_WITH_KNOTS('',3,(#5291,#5292,#5293,#5294,#5295,#5296,
#5297,#5298,#5299,#5300,#5301,#5302,#5303,#5304,#5305,#5306,#5307,#5308,
#5309,#5310,#5311,#5312,#5313,#5314,#5315,#5316,#5317,#5318,#5319,#5320,
#5321,#5322,#5323,#5324,#5325,#5326,#5327,#5328,#5329,#5330,#5331,#5332,
#5333,#5334,#5335,#5336,#5337,#5338,#5339,#5340,#5341,#5342,#5343,#5344,
#5345,#5346,#5347,#5348,#5349,#5350,#5351,#5352,#5353,#5354,#5355,#5356,
#5357,#5358,#5359,#5360,#5361,#5362,#5363,#5364,#5365,#5366,#5367,#5368,
#5369,#5370,#5371,#5372,#5373,#5374,#5375,#5376,#5377,#5378,#5379,#5380,
#5381,#5382,#5383,#5384,#5385,#5386,#5387,#5388,#5389,#5390,#5391,#5392,
#5393,#5394,#5395,#5396,#5397,#5398,#5399,#5400,#5401,#5402,#5403,#5404,
#5405,#5406,#5407,#5408,#5409,#5410,#5411,#5412,#5413,#5414,#5415,#5416,
#5417,#5418,#5419,#5420,#5421,#5422,#5423,#5424,#5425,#5426,#5427,#5428,
#5429,#5430,#5431,#5432,#5433,#5434,#5435,#5436,#5437,#5438,#5439,#5440,
#5441,#5442,#5443,#5444,#5445,#5446,#5447,#5448,#5449,#5450,#5451,#5452,
#5453,#5454,#5455,#5456,#5457,#5458,#5459,#5460,#5461,#5462,#5463,#5464,
#5465,#5466,#5467,#5468,#5469,#5470,#5471,#5472,#5473,#5474,#5475,#5476,
#5477,#5478,#5479,#5480),.UNSPECIFIED.,.F.,.F.,(4,3,3,3,3,3,3,3,3,3,3,3,
3,3,3,3,3,3,3,3,3,3,3,3,3,3,3,3,3,3,3,3,3,3,3,3,3,3,3,3,3,3,3,3,3,3,3,3,
3,3,3,3,3,3,3,3,3,3,3,3,3,3,3,4),(95.3643998413009,95.4680336789824,95.5719312818759,
95.6759621223708,95.7802739763669,95.8733633626321,95.9730469286449,96.072587276802,
96.1725193960759,96.2718801009265,96.3712078655298,96.4705331516489,96.5709109214849,
96.670380856732,96.7712125438624,96.8720442309929,96.9717277970057,97.0712681451628,
97.1712002644367,97.2705609692874,97.3698887338907,97.4692140200096,97.5695917898456,
97.6690617250928,97.7698934122232,97.8707250993537,97.9704086653665,98.069949013524,
98.1698811327978,98.2692418376485,98.3685696022517,98.4678948883709,98.5682726582068,
98.667742593454,98.7685742805842,98.8694059677144,98.9690895337272,99.0686298818843,
99.1685620011582,99.2679227060087,99.3672504706121,99.4665757567313,99.5669535265673,
99.6664234618143,99.7672551489447,99.8680868360752,99.9677704020879,100.067310750245,
100.167242869519,100.26660357437,100.365931338973,100.465256625092,100.565634394928,
100.665104330175,100.765936017306,100.866767704436,100.965052680092,101.063210571496,
101.16127360859,101.259273897761,101.357280728377,101.455284337592,101.55338873245,
101.647585148481),.UNSPECIFIED.);
#719=B_SPLINE_CURVE_WITH_KNOTS('',3,(#5482,#5483,#5484,#5485,#5486,#5487,
#5488,#5489,#5490,#5491,#5492),.UNSPECIFIED.,.F.,.F.,(4,1,1,1,1,1,1,1,4),
(101.647585148481,101.865448572797,102.864129441157,103.862810309518,104.861491177879,
105.86017204624,106.8588529146,107.857533782961,107.93077045566),
 .UNSPECIFIED.);
#720=B_SPLINE_CURVE_WITH_KNOTS('',3,(#5494,#5495,#5496,#5497,#5498,#5499,
#5500,#5501,#5502,#5503,#5504,#5505,#5506,#5507,#5508,#5509,#5510,#5511,
#5512,#5513,#5514,#5515,#5516,#5517,#5518,#5519,#5520,#5521,#5522,#5523,
#5524,#5525,#5526,#5527,#5528,#5529,#5530,#5531,#5532,#5533,#5534,#5535,
#5536,#5537,#5538,#5539,#5540,#5541,#5542,#5543,#5544,#5545,#5546,#5547,
#5548,#5549,#5550,#5551,#5552,#5553,#5554,#5555,#5556,#5557,#5558,#5559,
#5560,#5561,#5562,#5563,#5564,#5565,#5566,#5567,#5568,#5569,#5570,#5571,
#5572,#5573,#5574,#5575,#5576,#5577,#5578,#5579,#5580,#5581,#5582,#5583,
#5584,#5585,#5586,#5587,#5588,#5589,#5590,#5591,#5592,#5593,#5594,#5595,
#5596,#5597,#5598,#5599,#5600,#5601,#5602,#5603,#5604,#5605,#5606,#5607,
#5608,#5609,#5610,#5611,#5612,#5613,#5614,#5615,#5616,#5617,#5618,#5619,
#5620,#5621,#5622,#5623,#5624,#5625,#5626,#5627,#5628,#5629,#5630,#5631,
#5632,#5633,#5634,#5635,#5636,#5637,#5638,#5639,#5640,#5641,#5642,#5643,
#5644,#5645,#5646,#5647,#5648,#5649,#5650,#5651,#5652,#5653,#5654,#5655,
#5656,#5657,#5658,#5659,#5660,#5661,#5662,#5663,#5664,#5665,#5666,#5667,
#5668,#5669,#5670,#5671,#5672,#5673,#5674,#5675,#5676,#5677,#5678,#5679,
#5680,#5681,#5682,#5683,#5684,#5685,#5686),.UNSPECIFIED.,.F.,.F.,(4,3,3,
3,3,3,3,3,3,3,3,3,3,3,3,3,3,3,3,3,3,3,3,3,3,3,3,3,3,3,3,3,3,3,3,3,3,3,3,
3,3,3,3,3,3,3,3,3,3,3,3,3,3,3,3,3,3,3,3,3,3,3,3,3,4),(107.93077045566,108.029399639198,
108.132751515713,108.231141282269,108.329479409736,108.42779758391,108.526127461288,
108.624561429513,108.723056288678,108.821710387347,108.856214651322,108.955898217335,
109.055438565492,109.155370684766,109.254731389617,109.35405915422,109.453384440339,
109.553762210175,109.653232145423,109.754063832553,109.854895519683,109.954579085695,
110.054119433852,110.154051553126,110.253412257977,110.35274002258,110.452065308699,
110.552443078535,110.651913013782,110.752744700912,110.853576388043,110.953259954056,
111.052800302213,111.152732421487,111.252093126338,111.351420890941,111.45074617706,
111.551123946896,111.650593882143,111.751425569273,111.852257256404,111.951940822417,
112.051481170574,112.151413289848,112.250773994699,112.350101759302,112.449427045422,
112.549804815257,112.649274750505,112.750106437635,112.850938124765,112.950621690778,
113.050162038935,113.150094158209,113.249454863059,113.348782627663,113.448107913782,
113.548485683618,113.647955618865,113.748787305995,113.849618993126,113.963410379371,
114.076729763095,114.189250107695,114.213955762605),.UNSPECIFIED.);
#721=B_SPLINE_CURVE_WITH_KNOTS('',3,(#5688,#5689,#5690,#5691,#5692,#5693,
#5694,#5695,#5696,#5697,#5698,#5699,#5700,#5701,#5702,#5703,#5704,#5705,
#5706,#5707,#5708,#5709,#5710,#5711,#5712,#5713,#5714,#5715,#5716,#5717,
#5718,#5719,#5720,#5721,#5722,#5723,#5724,#5725,#5726,#5727,#5728,#5729,
#5730,#5731,#5732,#5733,#5734,#5735,#5736,#5737,#5738,#5739,#5740,#5741,
#5742,#5743,#5744,#5745,#5746,#5747,#5748,#5749,#5750,#5751,#5752,#5753,
#5754,#5755,#5756,#5757,#5758,#5759,#5760,#5761,#5762,#5763,#5764,#5765,
#5766,#5767,#5768,#5769,#5770,#5771,#5772,#5773,#5774,#5775,#5776,#5777,
#5778,#5779,#5780,#5781,#5782,#5783,#5784,#5785,#5786,#5787,#5788,#5789,
#5790,#5791,#5792,#5793,#5794,#5795,#5796,#5797,#5798,#5799,#5800,#5801,
#5802,#5803,#5804,#5805,#5806,#5807,#5808,#5809,#5810,#5811,#5812,#5813,
#5814,#5815,#5816,#5817,#5818,#5819,#5820,#5821,#5822,#5823,#5824,#5825,
#5826,#5827,#5828,#5829,#5830,#5831,#5832,#5833,#5834,#5835,#5836,#5837,
#5838,#5839,#5840,#5841,#5842,#5843,#5844,#5845,#5846,#5847,#5848,#5849,
#5850,#5851,#5852,#5853,#5854,#5855,#5856,#5857,#5858,#5859,#5860,#5861,
#5862,#5863,#5864,#5865,#5866,#5867,#5868,#5869,#5870,#5871,#5872,#5873,
#5874,#5875,#5876,#5877,#5878,#5879,#5880),.UNSPECIFIED.,.F.,.F.,(4,3,3,
3,3,3,3,3,3,3,3,3,3,3,3,3,3,3,3,3,3,3,3,3,3,3,3,3,3,3,3,3,3,3,3,3,3,3,3,
3,3,3,3,3,3,3,3,3,3,3,3,3,3,3,3,3,3,3,3,3,3,3,3,3,4),(114.21395576284,114.31380774229,
114.413664648862,114.513555872153,114.613578633856,114.713677918333,114.813953963102,
114.848299861486,114.947983427499,115.047523775657,115.14745589493,115.246816599781,
115.346144364385,115.445469650504,115.54584742034,115.645317355587,115.746149042717,
115.846980729847,115.94666429586,116.046204644017,116.146136763291,116.245497468142,
116.344825232745,116.444150518864,116.5445282887,116.643998223947,116.744829911078,
116.845661598208,116.945345164221,117.044885512378,117.144817631652,117.244178336503,
117.343506101106,117.442831387225,117.543209157061,117.642679092308,117.743510779439,
117.844342466569,117.944026032582,118.043566380739,118.143498500012,118.242859204863,
118.342186969466,118.441512255585,118.541890025421,118.641359960668,118.742191647798,
118.843023334929,118.942706900942,119.042247249099,119.142179368373,119.241540073224,
119.340867837827,119.440193123946,119.540570893782,119.640040829029,119.74087251616,
119.84170420329,119.941520374619,120.041194654516,120.140757472728,120.240240659712,
120.339676519161,120.439118953947,120.497141070019),.UNSPECIFIED.);
#722=B_SPLINE_CURVE_WITH_KNOTS('',3,(#5882,#5883,#5884,#5885,#5886,#5887,
#5888,#5889,#5890,#5891,#5892,#5893,#5894,#5895,#5896,#5897,#5898,#5899,
#5900,#5901,#5902,#5903,#5904,#5905,#5906,#5907,#5908,#5909,#5910,#5911,
#5912,#5913,#5914,#5915,#5916,#5917,#5918,#5919,#5920,#5921,#5922,#5923,
#5924,#5925,#5926,#5927,#5928,#5929,#5930,#5931,#5932,#5933,#5934,#5935,
#5936,#5937,#5938,#5939,#5940,#5941,#5942,#5943,#5944,#5945,#5946,#5947,
#5948,#5949,#5950,#5951,#5952,#5953,#5954,#5955,#5956,#5957,#5958,#5959,
#5960,#5961,#5962,#5963,#5964,#5965,#5966,#5967,#5968,#5969,#5970,#5971,
#5972,#5973,#5974,#5975,#5976,#5977,#5978,#5979,#5980,#5981,#5982,#5983,
#5984,#5985,#5986,#5987,#5988,#5989,#5990,#5991,#5992,#5993,#5994,#5995,
#5996,#5997,#5998,#5999,#6000,#6001,#6002,#6003,#6004,#6005,#6006,#6007,
#6008,#6009,#6010,#6011,#6012,#6013,#6014,#6015,#6016,#6017,#6018,#6019,
#6020,#6021,#6022,#6023,#6024,#6025,#6026,#6027,#6028,#6029,#6030,#6031,
#6032,#6033,#6034,#6035,#6036,#6037,#6038,#6039,#6040,#6041,#6042,#6043,
#6044,#6045,#6046,#6047,#6048,#6049,#6050,#6051,#6052,#6053,#6054,#6055,
#6056,#6057,#6058,#6059,#6060,#6061,#6062,#6063,#6064,#6065,#6066,#6067,
#6068,#6069,#6070,#6071),.UNSPECIFIED.,.F.,.F.,(4,3,3,3,3,3,3,3,3,3,3,3,
3,3,3,3,3,3,3,3,3,3,3,3,3,3,3,3,3,3,3,3,3,3,3,3,3,3,3,3,3,3,3,3,3,3,3,3,
3,3,3,3,3,3,3,3,3,3,3,3,3,3,3,4),(120.497141070246,120.611799468103,120.727559034228,
120.840385071651,120.940068637664,121.039608985821,121.139541105095,121.238901809945,
121.338229574549,121.437554860668,121.537932630504,121.637402565751,121.738234252881,
121.839065940012,121.938749506025,122.038289854181,122.138221973455,122.237582678306,
122.336910442909,122.436235729027,122.536613498864,122.63608343411,122.736915121241,
122.837746808372,122.937430374385,123.036970722542,123.136902841816,123.236263546666,
123.33559131127,123.434916597389,123.535294367225,123.634764302472,123.735595989603,
123.836427676733,123.936111242746,124.035651590903,124.135583710177,124.234944415028,
124.334272179631,124.433597465751,124.533975235586,124.633445170834,124.734276857964,
124.835108545094,124.934792111107,125.034332459264,125.134264578538,125.233625283389,
125.332953047992,125.432278334111,125.532656103947,125.632126039194,125.732957726325,
125.833789413455,125.932685008728,126.031438152,126.130077732587,126.228656280004,
126.327205255562,126.425756081762,126.5244022177,126.623100091491,126.721959841375,
126.780326377199),.UNSPECIFIED.);
#723=B_SPLINE_CURVE_WITH_KNOTS('',3,(#6073,#6074,#6075,#6076,#6077,#6078,
#6079,#6080,#6081,#6082,#6083,#6084),.UNSPECIFIED.,.F.,.F.,(4,2,1,1,1,1,
1,1,4),(126.780326377199,126.832470281815,127.831151150176,128.829832018537,
129.828512886898,130.827193755258,131.825874623619,132.82455549198,133.063511684379),
 .UNSPECIFIED.);
#724=B_SPLINE_CURVE_WITH_KNOTS('',3,(#6086,#6087,#6088,#6089,#6090,#6091,
#6092,#6093,#6094,#6095),.UNSPECIFIED.,.F.,.F.,(4,1,1,1,1,1,1,4),(133.063511684379,
133.823236360341,134.821917228701,135.820598097062,136.819278965423,137.817959833784,
138.816640702144,139.346696991558),.UNSPECIFIED.);
#725=B_SPLINE_CURVE_WITH_KNOTS('',3,(#6097,#6098,#6099,#6100,#6101,#6102,
#6103,#6104,#6105,#6106,#6107,#6108,#6109,#6110,#6111,#6112,#6113,#6114,
#6115,#6116,#6117,#6118,#6119,#6120,#6121,#6122,#6123,#6124,#6125,#6126,
#6127,#6128,#6129,#6130,#6131,#6132,#6133,#6134,#6135,#6136,#6137,#6138,
#6139,#6140,#6141,#6142,#6143,#6144,#6145,#6146,#6147,#6148,#6149,#6150,
#6151,#6152,#6153,#6154,#6155,#6156,#6157,#6158,#6159,#6160,#6161,#6162,
#6163,#6164,#6165,#6166,#6167,#6168,#6169,#6170,#6171,#6172,#6173,#6174,
#6175,#6176,#6177,#6178,#6179,#6180,#6181,#6182,#6183,#6184,#6185,#6186,
#6187,#6188,#6189,#6190,#6191,#6192,#6193,#6194,#6195,#6196,#6197,#6198,
#6199,#6200,#6201,#6202,#6203,#6204,#6205,#6206,#6207,#6208,#6209,#6210,
#6211,#6212,#6213,#6214,#6215,#6216,#6217,#6218,#6219,#6220,#6221,#6222,
#6223,#6224,#6225,#6226,#6227,#6228,#6229,#6230,#6231,#6232,#6233,#6234,
#6235,#6236,#6237,#6238,#6239,#6240,#6241,#6242,#6243,#6244,#6245,#6246,
#6247,#6248,#6249,#6250,#6251,#6252,#6253,#6254,#6255,#6256,#6257,#6258,
#6259,#6260,#6261,#6262,#6263,#6264,#6265,#6266,#6267,#6268,#6269,#6270,
#6271,#6272,#6273,#6274,#6275,#6276,#6277,#6278,#6279,#6280,#6281,#6282,
#6283,#6284,#6285,#6286,#6287,#6288,#6289),.UNSPECIFIED.,.F.,.F.,(4,3,3,
3,3,3,3,3,3,3,3,3,3,3,3,3,3,3,3,3,3,3,3,3,3,3,3,3,3,3,3,3,3,3,3,3,3,3,3,
3,3,3,3,3,3,3,3,3,3,3,3,3,3,3,3,3,3,3,3,3,3,3,3,3,4),(139.34669715841,139.452165000516,
139.557994919341,139.6640172491,139.770348389444,139.815321570505,139.915005136518,
140.014545484675,140.114477603949,140.2138383088,140.313166073403,140.412491359522,
140.512869129358,140.612339064606,140.713170751736,140.814002438866,140.913686004879,
141.013226353036,141.11315847231,141.212519177161,141.311846941764,141.411172227884,
141.511549997719,141.611019932967,141.711851620097,141.812683307227,141.91236687324,
142.011907221396,142.11183934067,142.211200045521,142.310527810124,142.409853096242,
142.510230866079,142.609700801325,142.710532488456,142.811364175587,142.9110477416,
143.010588089757,143.110520209031,143.209880913881,143.309208678485,143.408533964604,
143.50891173444,143.608381669687,143.709213356817,143.810045043948,143.909728609961,
144.009268958118,144.109201077392,144.208561782243,144.307889546846,144.407214832966,
144.507592602801,144.607062538049,144.707894225179,144.808725912309,144.911370460613,
145.009401903958,145.107341864103,145.205222543426,145.303076064612,145.400976998535,
145.49890612746,145.596947071887,145.629882298738),.UNSPECIFIED.);
#726=B_SPLINE_CURVE_WITH_KNOTS('',3,(#6291,#6292,#6293,#6294,#6295,#6296,
#6297,#6298,#6299,#6300,#6301),.UNSPECIFIED.,.F.,.F.,(4,1,1,1,1,1,1,1,4),
(145.629882298738,145.80740678067,146.80608764903,147.804768517391,148.803449385752,
149.802130254113,150.800811122473,151.799491990834,151.913067605917),
 .UNSPECIFIED.);
#727=B_SPLINE_CURVE_WITH_KNOTS('',3,(#6303,#6304,#6305,#6306,#6307,#6308,
#6309,#6310,#6311,#6312,#6313,#6314,#6315,#6316,#6317,#6318,#6319,#6320,
#6321,#6322,#6323,#6324,#6325,#6326,#6327,#6328,#6329,#6330,#6331,#6332,
#6333,#6334,#6335,#6336,#6337,#6338,#6339,#6340,#6341,#6342,#6343,#6344,
#6345,#6346,#6347,#6348,#6349,#6350,#6351,#6352,#6353,#6354,#6355,#6356,
#6357,#6358,#6359,#6360,#6361,#6362,#6363,#6364,#6365,#6366,#6367,#6368,
#6369,#6370,#6371,#6372,#6373,#6374,#6375,#6376,#6377,#6378,#6379,#6380,
#6381,#6382,#6383,#6384,#6385,#6386,#6387,#6388,#6389,#6390,#6391,#6392,
#6393,#6394,#6395,#6396,#6397,#6398,#6399,#6400,#6401,#6402,#6403,#6404,
#6405,#6406,#6407,#6408,#6409,#6410,#6411,#6412,#6413,#6414,#6415,#6416,
#6417,#6418,#6419,#6420,#6421,#6422,#6423,#6424,#6425,#6426,#6427,#6428,
#6429,#6430,#6431,#6432,#6433,#6434,#6435,#6436,#6437,#6438,#6439,#6440,
#6441,#6442,#6443,#6444,#6445,#6446,#6447,#6448,#6449,#6450,#6451,#6452,
#6453,#6454,#6455,#6456,#6457,#6458,#6459,#6460,#6461,#6462,#6463,#6464,
#6465,#6466,#6467,#6468,#6469,#6470,#6471,#6472,#6473,#6474,#6475,#6476,
#6477,#6478,#6479,#6480,#6481,#6482,#6483,#6484,#6485,#6486,#6487,#6488,
#6489,#6490,#6491,#6492),.UNSPECIFIED.,.F.,.F.,(4,3,3,3,3,3,3,3,3,3,3,3,
3,3,3,3,3,3,3,3,3,3,3,3,3,3,3,3,3,3,3,3,3,3,3,3,3,3,3,3,3,3,3,3,3,3,3,3,
3,3,3,3,3,3,3,3,3,3,3,3,3,3,3,4),(151.913067605917,152.011345432823,152.10969886112,
152.207764087066,152.305785655644,152.403795535228,152.502389866219,152.600528477886,
152.69935066854,152.798172859195,152.897856425208,152.997396773365,153.097328892639,
153.19668959749,153.296017362093,153.395342648212,153.495720418048,153.595190353295,
153.696022040426,153.796853727556,153.896537293569,153.996077641725,154.096009760999,
154.19537046585,154.294698230453,154.394023516572,154.494401286408,154.593871221655,
154.694702908785,154.795534595916,154.895218161929,154.994758510086,155.09469062936,
155.19405133421,155.293379098814,155.392704384933,155.493082154769,155.592552090016,
155.693383777146,155.794215464277,155.89389903029,155.993439378447,156.093371497721,
156.192732202572,156.292059967175,156.391385253294,156.49176302313,156.591232958377,
156.692064645508,156.792896332638,156.892579898651,156.992120246808,157.092052366082,
157.191413070933,157.290740835536,157.390066121655,157.490443891491,157.589913826738,
157.690745513869,157.791577200999,157.901929993823,158.011949532061,158.121400059036,
158.196252481728),.UNSPECIFIED.);
#728=B_SPLINE_CURVE_WITH_KNOTS('',3,(#6494,#6495,#6496,#6497,#6498,#6499,
#6500,#6501,#6502,#6503),.UNSPECIFIED.,.F.,.F.,(4,1,1,1,1,1,1,4),(158.196252913097,
158.790258069359,159.78893893772,160.787619806081,161.786300674442,162.784981542803,
163.783662411163,164.479438220276),.UNSPECIFIED.);
#729=B_SPLINE_CURVE_WITH_KNOTS('',3,(#6505,#6506,#6507,#6508,#6509,#6510,
#6511,#6512,#6513,#6514,#6515,#6516,#6517,#6518,#6519,#6520,#6521,#6522,
#6523,#6524,#6525,#6526,#6527,#6528,#6529,#6530,#6531,#6532,#6533,#6534,
#6535,#6536,#6537,#6538,#6539,#6540,#6541,#6542,#6543,#6544,#6545,#6546,
#6547,#6548,#6549,#6550,#6551,#6552,#6553,#6554,#6555,#6556,#6557,#6558,
#6559,#6560,#6561,#6562,#6563,#6564,#6565,#6566,#6567,#6568,#6569,#6570,
#6571,#6572,#6573,#6574,#6575,#6576,#6577,#6578,#6579,#6580,#6581,#6582,
#6583,#6584,#6585,#6586,#6587,#6588,#6589,#6590,#6591,#6592,#6593,#6594,
#6595,#6596,#6597,#6598,#6599,#6600,#6601,#6602,#6603,#6604,#6605,#6606,
#6607,#6608,#6609,#6610,#6611,#6612,#6613,#6614,#6615,#6616,#6617,#6618,
#6619,#6620,#6621,#6622,#6623,#6624,#6625,#6626,#6627,#6628,#6629,#6630,
#6631,#6632,#6633,#6634,#6635,#6636,#6637,#6638,#6639,#6640,#6641,#6642,
#6643,#6644,#6645,#6646,#6647,#6648,#6649,#6650,#6651,#6652,#6653,#6654,
#6655,#6656,#6657,#6658,#6659,#6660,#6661,#6662,#6663,#6664,#6665,#6666,
#6667,#6668,#6669,#6670,#6671,#6672,#6673,#6674,#6675,#6676,#6677,#6678,
#6679,#6680,#6681,#6682,#6683,#6684,#6685,#6686,#6687,#6688,#6689,#6690,
#6691,#6692,#6693,#6694),.UNSPECIFIED.,.F.,.F.,(4,3,3,3,3,3,3,3,3,3,3,3,
3,3,3,3,3,3,3,3,3,3,3,3,3,3,3,3,3,3,3,3,3,3,3,3,3,3,3,3,3,3,3,3,3,3,3,3,
3,3,3,3,3,3,3,3,3,3,3,3,3,3,3,4),(164.479438408164,164.598666659614,164.719510400896,
164.782343279524,164.882026845537,164.981567193694,165.081499312967,165.180860017818,
165.280187782421,165.37951306854,165.479890838376,165.579360773623,165.680192460754,
165.781024147885,165.880707713898,165.980248062055,166.080180181329,166.17954088618,
166.278868650783,166.378193936903,166.478571706738,166.578041641986,166.678873329116,
166.779705016246,166.879388582259,166.978928930415,167.078861049689,167.17822175454,
167.277549519143,167.376874805262,167.477252575098,167.576722510345,167.677554197475,
167.778385884606,167.878069450619,167.977609798776,168.07754191805,168.1769026229,
168.276230387504,168.375555673623,168.475933443459,168.575403378706,168.676235065836,
168.777066752967,168.87675031898,168.976290667137,169.076222786411,169.175583491262,
169.274911255866,169.374236541985,169.474614311821,169.574084247068,169.674915934198,
169.775747621328,169.87522536163,169.974560042941,170.073779603311,170.172936277215,
170.272060841864,170.371184034681,170.470405346651,170.569674070912,170.669121992281,
170.762623527456),.UNSPECIFIED.);
#730=B_SPLINE_CURVE_WITH_KNOTS('',3,(#6696,#6697,#6698,#6699,#6700,#6701,
#6702,#6703,#6704,#6705,#6706,#6707),.UNSPECIFIED.,.F.,.F.,(4,2,1,1,1,1,
1,1,4),(170.762623527456,170.774428489689,171.773109358049,172.77179022641,
173.770471094771,174.769151963132,175.767832831492,176.766513699853,177.045804600382),
 .UNSPECIFIED.);
#731=B_SPLINE_CURVE_WITH_KNOTS('',3,(#6709,#6710,#6711,#6712,#6713,#6714,
#6715,#6716,#6717,#6718,#6719,#6720,#6721,#6722,#6723,#6724,#6725,#6726,
#6727,#6728,#6729,#6730,#6731,#6732,#6733,#6734,#6735,#6736,#6737,#6738,
#6739,#6740,#6741,#6742,#6743,#6744,#6745,#6746,#6747,#6748,#6749,#6750,
#6751,#6752,#6753,#6754,#6755,#6756,#6757,#6758,#6759,#6760,#6761,#6762,
#6763,#6764,#6765,#6766,#6767,#6768,#6769,#6770,#6771,#6772,#6773,#6774,
#6775,#6776,#6777,#6778,#6779,#6780,#6781,#6782,#6783,#6784,#6785,#6786,
#6787,#6788,#6789,#6790,#6791,#6792,#6793,#6794,#6795,#6796,#6797,#6798,
#6799,#6800,#6801,#6802,#6803,#6804,#6805,#6806,#6807,#6808,#6809,#6810,
#6811,#6812,#6813,#6814,#6815,#6816,#6817,#6818,#6819,#6820,#6821,#6822,
#6823,#6824,#6825,#6826,#6827,#6828,#6829,#6830,#6831,#6832,#6833,#6834,
#6835,#6836,#6837,#6838,#6839,#6840,#6841,#6842,#6843,#6844,#6845,#6846,
#6847,#6848,#6849,#6850,#6851,#6852,#6853,#6854,#6855,#6856,#6857,#6858,
#6859,#6860,#6861,#6862,#6863,#6864,#6865,#6866,#6867,#6868,#6869,#6870,
#6871,#6872,#6873,#6874,#6875,#6876,#6877,#6878,#6879,#6880,#6881,#6882,
#6883,#6884,#6885,#6886,#6887,#6888,#6889,#6890,#6891,#6892,#6893,#6894,
#6895,#6896,#6897,#6898,#6899,#6900,#6901),.UNSPECIFIED.,.F.,.F.,(4,3,3,
3,3,3,3,3,3,3,3,3,3,3,3,3,3,3,3,3,3,3,3,3,3,3,3,3,3,3,3,3,3,3,3,3,3,3,3,
3,3,3,3,3,3,3,3,3,3,3,3,3,3,3,3,3,3,3,3,3,3,3,3,3,4),(177.045808834635,
177.144350017315,177.242844566572,177.341323967424,177.439819680818,177.538424273858,
177.637093471072,177.735923162666,177.765194568214,177.864878134227,177.964418482384,
178.064350601658,178.163711306509,178.263039071112,178.362364357231,178.462742127067,
178.562212062314,178.663043749445,178.763875436575,178.863559002587,178.963099350744,
179.063031470018,179.162392174869,179.261719939472,179.361045225591,179.461422995427,
179.560892930674,179.661724617804,179.762556304935,179.862239870948,179.961780219105,
180.061712338379,180.161073043229,180.260400807833,180.359726093952,180.460103863788,
180.559573799035,180.660405486165,180.761237173296,180.860920739309,180.960461087466,
181.06039320674,181.159753911591,181.259081676194,181.358406962314,181.458784732149,
181.558254667397,181.659086354527,181.759918041657,181.85960160767,181.959141955827,
182.059074075101,182.158434779952,182.257762544555,182.357087830674,182.45746560051,
182.556935535757,182.657767222888,182.758598910018,182.860615373313,182.962463753037,
183.064135186073,183.165702513586,183.267179688219,183.328994141815),
 .UNSPECIFIED.);
#732=B_SPLINE_CURVE_WITH_KNOTS('',3,(#6903,#6904,#6905,#6906,#6907,#6908,
#6909,#6910,#6911,#6912),.UNSPECIFIED.,.F.,.F.,(4,1,1,1,1,1,1,4),(183.328999479296,
183.757279778378,184.755960646739,185.7546415151,186.753322383461,187.752003251821,
188.750684120182,189.612179448995),.UNSPECIFIED.);
#733=B_SPLINE_CURVE_WITH_KNOTS('',3,(#6914,#6915,#6916,#6917,#6918,#6919,
#6920,#6921,#6922,#6923,#6924),.UNSPECIFIED.,.F.,.F.,(4,1,1,1,1,1,1,1,4),
(189.612179448995,189.749364988543,190.748045856904,191.746726725264,192.745407593625,
193.744088461986,194.742769330347,195.741450198707,195.895364756174),
 .UNSPECIFIED.);
#734=B_SPLINE_CURVE_WITH_KNOTS('',3,(#6926,#6927,#6928,#6929,#6930,#6931,
#6932,#6933,#6934,#6935),.UNSPECIFIED.,.F.,.F.,(4,1,1,1,1,1,1,4),(195.895364756174,
196.740131067068,197.738811935429,198.73749280379,199.73617367215,200.734854540511,
201.733535408872,202.178550063354),.UNSPECIFIED.);
#735=B_SPLINE_CURVE_WITH_KNOTS('',3,(#6937,#6938,#6939,#6940,#6941,#6942,
#6943,#6944,#6945,#6946),.UNSPECIFIED.,.F.,.F.,(4,1,1,1,1,1,1,4),(202.178550063354,
202.732216277233,203.730897145593,204.729578013954,205.728258882315,206.726939750676,
207.725620619036,208.461735370533),.UNSPECIFIED.);
#736=B_SPLINE_CURVE_WITH_KNOTS('',3,(#6948,#6949,#6950,#6951,#6952,#6953,
#6954,#6955,#6956,#6957,#6958,#6959,#6960,#6961,#6962,#6963,#6964,#6965,
#6966,#6967,#6968,#6969,#6970,#6971,#6972,#6973,#6974,#6975,#6976,#6977,
#6978,#6979,#6980,#6981,#6982,#6983,#6984,#6985,#6986,#6987,#6988,#6989,
#6990,#6991,#6992,#6993,#6994,#6995,#6996,#6997,#6998,#6999,#7000,#7001,
#7002,#7003,#7004,#7005,#7006,#7007,#7008,#7009,#7010,#7011,#7012,#7013,
#7014,#7015,#7016,#7017,#7018,#7019,#7020,#7021,#7022,#7023,#7024,#7025,
#7026,#7027,#7028,#7029,#7030,#7031,#7032,#7033,#7034,#7035,#7036,#7037,
#7038,#7039,#7040,#7041,#7042,#7043,#7044,#7045,#7046,#7047,#7048,#7049,
#7050,#7051,#7052,#7053,#7054,#7055,#7056,#7057,#7058,#7059,#7060,#7061,
#7062,#7063,#7064,#7065,#7066,#7067,#7068,#7069,#7070,#7071,#7072,#7073,
#7074,#7075,#7076,#7077,#7078,#7079,#7080,#7081,#7082,#7083,#7084,#7085,
#7086,#7087,#7088,#7089,#7090,#7091,#7092,#7093,#7094,#7095,#7096,#7097,
#7098,#7099,#7100,#7101,#7102,#7103,#7104,#7105,#7106,#7107,#7108,#7109,
#7110,#7111,#7112,#7113,#7114,#7115,#7116,#7117,#7118,#7119,#7120,#7121,
#7122,#7123,#7124,#7125,#7126,#7127,#7128,#7129,#7130,#7131,#7132,#7133,
#7134,#7135,#7136,#7137),.UNSPECIFIED.,.F.,.F.,(4,3,3,3,3,3,3,3,3,3,3,3,
3,3,3,3,3,3,3,3,3,3,3,3,3,3,3,3,3,3,3,3,3,3,3,3,3,3,3,3,3,3,3,3,3,3,3,3,
3,3,3,3,3,3,3,3,3,3,3,3,3,3,3,4),(208.461735551838,208.593018519617,208.724301487397,
208.823985053394,208.923525401536,209.023457520813,209.122818225649,209.222145990237,
209.321471276341,209.421849046195,209.521318981428,209.622150668593,209.722982355758,
209.822665921751,209.922206269888,210.022138389167,210.121499093997,210.22082685858,
210.320152144678,210.420529914538,210.519999849765,210.620831536942,210.721663224119,
210.821346790229,210.920887138484,211.020819257734,211.120179962682,211.219507727383,
211.318833013599,211.419210783319,211.518680718661,211.61951240557,211.720344092479,
211.820027658363,211.919568006391,212.019500125697,212.118860830421,212.218188594898,
212.317513880893,212.417891650879,212.517361586006,212.618193273423,212.71902496084,
212.818708526764,212.91824887483,213.018180994127,213.117541698884,213.216869463392,
213.316194749415,213.416572519362,213.516042454512,213.616874141857,213.717705829201,
213.817389395867,213.916929744679,214.01686186379,214.116222569296,214.215550334553,
214.314875621323,214.415253390383,214.514723326269,214.615555011916,214.716386697562,
214.744920677713),.UNSPECIFIED.);
#737=B_SPLINE_CURVE_WITH_KNOTS('',3,(#7139,#7140,#7141,#7142,#7143,#7144,
#7145,#7146,#7147,#7148,#7149,#7150,#7151,#7152,#7153,#7154,#7155,#7156,
#7157,#7158,#7159,#7160,#7161,#7162,#7163,#7164,#7165,#7166,#7167,#7168,
#7169,#7170,#7171,#7172,#7173,#7174,#7175,#7176,#7177,#7178,#7179,#7180,
#7181,#7182,#7183,#7184,#7185,#7186,#7187,#7188,#7189,#7190,#7191,#7192,
#7193,#7194,#7195,#7196,#7197,#7198,#7199,#7200,#7201,#7202,#7203,#7204,
#7205,#7206,#7207,#7208,#7209,#7210,#7211,#7212,#7213,#7214,#7215,#7216,
#7217,#7218,#7219,#7220,#7221,#7222,#7223,#7224,#7225,#7226,#7227,#7228,
#7229,#7230,#7231,#7232,#7233,#7234,#7235,#7236,#7237,#7238,#7239,#7240,
#7241,#7242,#7243,#7244,#7245,#7246,#7247,#7248,#7249,#7250,#7251,#7252,
#7253,#7254,#7255,#7256,#7257,#7258,#7259,#7260,#7261,#7262,#7263,#7264,
#7265,#7266,#7267,#7268,#7269,#7270,#7271,#7272,#7273,#7274,#7275,#7276,
#7277,#7278,#7279,#7280,#7281,#7282,#7283,#7284,#7285,#7286,#7287,#7288,
#7289,#7290,#7291,#7292,#7293,#7294,#7295,#7296,#7297,#7298,#7299,#7300,
#7301,#7302,#7303,#7304,#7305,#7306,#7307,#7308,#7309,#7310,#7311,#7312,
#7313,#7314,#7315,#7316,#7317,#7318,#7319,#7320,#7321,#7322,#7323,#7324,
#7325,#7326,#7327,#7328),.UNSPECIFIED.,.F.,.F.,(4,3,3,3,3,3,3,3,3,3,3,3,
3,3,3,3,3,3,3,3,3,3,3,3,3,3,3,3,3,3,3,3,3,3,3,3,3,3,3,3,3,3,3,3,3,3,3,3,
3,3,3,3,3,3,3,3,3,3,3,3,3,3,3,4),(214.744920678121,214.844128676269,214.943195171378,
215.042149305934,215.141042635403,215.239906261421,215.338771247639,215.437735542156,
215.536750313415,215.635939296236,215.715067565922,215.814751131676,215.914291479564,
216.014223598904,216.11358430346,216.21291206776,216.312237353568,216.412615123747,
216.512085058666,216.612916746474,216.713748434283,216.813432004555,216.912972356988,
217.012904475195,217.112265184329,217.211592953209,217.310918243593,217.411296008356,
217.510765947794,217.611597625219,217.712429302644,217.812112860803,217.911653201114,
218.011585322351,218.110946019429,218.210273776305,218.309599054752,218.409976833815,
218.509446761601,218.610278466303,218.711110171005,218.810793737748,218.910334086561,
219.010266205662,219.109626910987,219.208954675997,219.308279962453,219.408657731681,
219.508127667096,219.60895935323,219.709791039365,219.809474632422,219.909015007748,
220.008947120245,220.108307852369,220.207635644225,220.306960957539,220.407338695086,
220.506808657111,220.607640282419,220.708471907726,220.827206194457,220.944620333216,
221.028105769477),.UNSPECIFIED.);
#738=B_SPLINE_CURVE_WITH_KNOTS('',3,(#7330,#7331,#7332,#7333,#7334,#7335,
#7336,#7337,#7338,#7339),.UNSPECIFIED.,.F.,.F.,(4,1,1,1,1,1,1,4),(221.028105984892,
221.707152776087,222.705833644448,223.704514512808,224.703195381169,225.70187624953,
226.700557117891,227.311291292072),.UNSPECIFIED.);
#739=B_SPLINE_CURVE_WITH_KNOTS('',3,(#7341,#7342,#7343,#7344,#7345,#7346,
#7347,#7348,#7349,#7350),.UNSPECIFIED.,.F.,.F.,(4,1,1,1,1,1,1,4),(227.311291292072,
227.699237986251,228.697918854612,229.696599722973,230.695280591334,231.693961459694,
232.692642328055,233.594476599252),.UNSPECIFIED.);
#740=B_SPLINE_CURVE_WITH_KNOTS('',3,(#7352,#7353,#7354,#7355,#7356,#7357),
 .UNSPECIFIED.,.F.,.F.,(4,1,1,4),(233.594476599252,233.691323196416,234.690004064777,
235.619089830444),.UNSPECIFIED.);
#741=B_SPLINE_CURVE_WITH_KNOTS('',3,(#7361,#7362,#7363,#7364,#7365,#7366,
#7367,#7368,#7369,#7370,#7371,#7372,#7373,#7374,#7375,#7376,#7377,#7378,
#7379,#7380,#7381,#7382,#7383,#7384,#7385,#7386,#7387,#7388,#7389,#7390,
#7391,#7392,#7393,#7394),.UNSPECIFIED.,.F.,.F.,(4,3,3,3,3,3,3,3,3,3,3,4),
(-237.686046669859,-237.58402334176,-237.482061745961,-237.380110302383,
-237.27816118961,-237.176189769977,-237.074171387682,-236.972000880612,
-236.869752054663,-236.767301150916,-236.687365801498,-236.569426436252),
 .UNSPECIFIED.);
#742=B_SPLINE_CURVE_WITH_KNOTS('',3,(#7396,#7397,#7398,#7399,#7400,#7401,
#7402,#7403,#7404,#7405,#7406,#7407,#7408,#7409,#7410,#7411,#7412,#7413,
#7414,#7415,#7416,#7417,#7418,#7419,#7420,#7421,#7422,#7423,#7424,#7425,
#7426,#7427,#7428,#7429,#7430,#7431,#7432,#7433,#7434,#7435,#7436,#7437,
#7438,#7439,#7440,#7441,#7442,#7443,#7444,#7445,#7446,#7447,#7448,#7449,
#7450,#7451,#7452,#7453,#7454,#7455,#7456,#7457,#7458,#7459,#7460,#7461,
#7462,#7463,#7464,#7465,#7466,#7467,#7468,#7469,#7470,#7471,#7472,#7473,
#7474,#7475,#7476,#7477,#7478,#7479,#7480,#7481,#7482,#7483,#7484,#7485,
#7486,#7487,#7488,#7489,#7490,#7491,#7492,#7493,#7494,#7495,#7496,#7497,
#7498,#7499,#7500,#7501,#7502,#7503,#7504,#7505,#7506,#7507,#7508,#7509,
#7510,#7511,#7512,#7513,#7514,#7515,#7516,#7517,#7518,#7519,#7520,#7521,
#7522,#7523,#7524,#7525,#7526,#7527,#7528,#7529,#7530,#7531,#7532,#7533,
#7534,#7535,#7536,#7537,#7538,#7539,#7540,#7541,#7542,#7543,#7544,#7545,
#7546,#7547,#7548,#7549,#7550,#7551,#7552,#7553,#7554,#7555,#7556,#7557,
#7558,#7559,#7560,#7561,#7562,#7563,#7564,#7565,#7566,#7567,#7568,#7569,
#7570,#7571,#7572,#7573,#7574,#7575,#7576,#7577,#7578,#7579,#7580,#7581,
#7582,#7583,#7584,#7585),.UNSPECIFIED.,.F.,.F.,(4,3,3,3,3,3,3,3,3,3,3,3,
3,3,3,3,3,3,3,3,3,3,3,3,3,3,3,3,3,3,3,3,3,3,3,3,3,3,3,3,3,3,3,3,3,3,3,3,
3,3,3,3,3,3,3,3,3,3,3,3,3,3,3,4),(-236.569426436046,-236.47210942377,-236.374181362441,
-236.277091450807,-236.180049642806,-236.083023280348,-235.984438693545,
-235.887287588253,-235.787986260695,-235.688684933137,-235.588851429478,
-235.489161004665,-235.389266387179,-235.289756450306,-235.190280123486,
-235.090807160138,-234.990606386298,-234.890992517576,-234.790498291177,
-234.690004064777,-234.590145789274,-234.490427147139,-234.390539153298,
-234.290992751295,-234.191476918733,-234.091961448655,-233.991801885595,
-233.892138511189,-233.791730853802,-233.691323196416,-233.591775013876,
-233.492371933963,-233.392405733225,-233.293185905218,-233.194000068945,
-233.094817577393,-232.994273765058,-232.894947324027,-232.793794826041,
-232.692642328055,-232.592929711517,-232.493360185805,-232.393435345041,
-232.294045373771,-232.194688375603,-232.095333929155,-231.994990811789,
-231.89549219828,-231.794726828987,-231.693961459694,-231.594257060298,
-231.494695422986,-231.39476856903,-231.295385617913,-231.196035295539,
-231.09668716973,-230.996335525131,-230.896842286067,-230.796061438701,
-230.695280591334,-230.585288532613,-230.475619265595,-230.366499298658,
-230.286241549226),.UNSPECIFIED.);
#743=B_SPLINE_CURVE_WITH_KNOTS('',3,(#7587,#7588,#7589,#7590,#7591,#7592,
#7593,#7594,#7595,#7596),.UNSPECIFIED.,.F.,.F.,(4,1,1,1,1,1,1,4),(-230.286241129072,
-229.696599722973,-228.697918854612,-227.699237986251,-226.700557117891,
-225.70187624953,-224.703195381169,-224.003055821893),.UNSPECIFIED.);
#744=B_SPLINE_CURVE_WITH_KNOTS('',3,(#7598,#7599,#7600,#7601,#7602,#7603,
#7604,#7605,#7606,#7607,#7608,#7609,#7610,#7611,#7612,#7613,#7614,#7615,
#7616,#7617,#7618,#7619,#7620,#7621,#7622,#7623,#7624,#7625,#7626,#7627,
#7628,#7629,#7630,#7631,#7632,#7633,#7634,#7635,#7636,#7637,#7638,#7639,
#7640,#7641,#7642,#7643,#7644,#7645,#7646,#7647,#7648,#7649,#7650,#7651,
#7652,#7653,#7654,#7655,#7656,#7657,#7658,#7659,#7660,#7661,#7662,#7663,
#7664,#7665,#7666,#7667,#7668,#7669,#7670,#7671,#7672,#7673,#7674,#7675,
#7676,#7677,#7678,#7679,#7680,#7681,#7682,#7683,#7684,#7685,#7686,#7687,
#7688,#7689,#7690,#7691,#7692,#7693,#7694,#7695,#7696,#7697,#7698,#7699,
#7700,#7701,#7702,#7703,#7704,#7705,#7706,#7707,#7708,#7709,#7710,#7711,
#7712,#7713,#7714,#7715,#7716,#7717,#7718,#7719,#7720,#7721,#7722,#7723,
#7724,#7725,#7726,#7727,#7728,#7729,#7730,#7731,#7732,#7733,#7734,#7735,
#7736,#7737,#7738,#7739,#7740,#7741,#7742,#7743,#7744,#7745,#7746,#7747,
#7748,#7749,#7750,#7751,#7752,#7753,#7754,#7755,#7756,#7757,#7758,#7759,
#7760,#7761,#7762,#7763,#7764,#7765,#7766,#7767,#7768,#7769,#7770,#7771,
#7772,#7773,#7774,#7775,#7776,#7777,#7778,#7779,#7780,#7781,#7782,#7783,
#7784,#7785,#7786,#7787),.UNSPECIFIED.,.F.,.F.,(4,3,3,3,3,3,3,3,3,3,3,3,
3,3,3,3,3,3,3,3,3,3,3,3,3,3,3,3,3,3,3,3,3,3,3,3,3,3,3,3,3,3,3,3,3,3,3,3,
3,3,3,3,3,3,3,3,3,3,3,3,3,3,3,4),(-224.003055642521,-223.88325798579,-223.761769132628,
-223.704514512808,-223.604830784056,-223.505290271404,-223.405358193035,
-223.30599732063,-223.206669387694,-223.107343932691,-223.00696636063,-222.907496256868,
-222.806664950658,-222.705833644448,-222.606150061763,-222.506609696167,
-222.406677581157,-222.307316857118,-222.207989072708,-222.108663766188,
-222.008286018663,-221.908816061752,-221.807984418919,-221.707152776087,
-221.607469264316,-221.507928971319,-221.40799683837,-221.308636190515,
-221.209308483473,-221.109983255403,-221.009605418484,-220.910135541903,
-220.809303724815,-220.708471907726,-220.608788315492,-220.509247940804,
-220.409315828124,-220.309955096181,-220.210627304334,-220.111301990857,
-220.010924252984,-219.911454290377,-219.810622664871,-219.709791039365,
-219.610107473322,-219.510567125058,-219.410635005801,-219.311274300658,
-219.211946535692,-219.11262124914,-219.012243479606,-218.912773543759,
-218.811941857382,-218.711110171005,-218.611558273906,-218.512149497141,
-218.412856080209,-218.313625803522,-218.214427986811,-218.115231989806,
-218.015937831542,-217.916596853038,-217.817075105393,-217.719870514713),
 .UNSPECIFIED.);
#745=B_SPLINE_CURVE_WITH_KNOTS('',3,(#7789,#7790,#7791,#7792,#7793,#7794,
#7795,#7796,#7797,#7798,#7799,#7800),.UNSPECIFIED.,.F.,.F.,(4,2,1,1,1,1,
1,1,4),(-217.719870514713,-217.712429302644,-216.713748434283,-215.715067565922,
-214.716386697562,-213.717705829201,-212.71902496084,-211.720344092479,
-211.436689775384),.UNSPECIFIED.);
#746=B_SPLINE_CURVE_WITH_KNOTS('',3,(#7802,#7803,#7804,#7805,#7806,#7807,
#7808,#7809,#7810,#7811,#7812,#7813,#7814,#7815,#7816,#7817,#7818,#7819,
#7820,#7821,#7822,#7823,#7824,#7825,#7826,#7827,#7828,#7829,#7830,#7831,
#7832,#7833,#7834,#7835,#7836,#7837,#7838,#7839,#7840,#7841,#7842,#7843,
#7844,#7845,#7846,#7847,#7848,#7849,#7850,#7851,#7852,#7853,#7854,#7855,
#7856,#7857,#7858,#7859,#7860,#7861,#7862,#7863,#7864,#7865,#7866,#7867,
#7868,#7869,#7870,#7871,#7872,#7873,#7874,#7875,#7876,#7877,#7878,#7879,
#7880,#7881,#7882,#7883,#7884,#7885,#7886,#7887,#7888,#7889,#7890,#7891,
#7892,#7893,#7894,#7895,#7896,#7897,#7898,#7899,#7900,#7901,#7902,#7903,
#7904,#7905,#7906,#7907,#7908,#7909,#7910,#7911,#7912,#7913,#7914,#7915,
#7916,#7917,#7918,#7919,#7920,#7921,#7922,#7923,#7924,#7925,#7926,#7927,
#7928,#7929,#7930,#7931,#7932,#7933,#7934,#7935,#7936,#7937,#7938,#7939,
#7940,#7941,#7942,#7943,#7944,#7945,#7946,#7947,#7948,#7949,#7950,#7951,
#7952,#7953,#7954,#7955,#7956,#7957,#7958,#7959,#7960,#7961,#7962,#7963,
#7964,#7965,#7966,#7967,#7968,#7969,#7970,#7971,#7972,#7973,#7974,#7975,
#7976,#7977,#7978,#7979,#7980,#7981,#7982,#7983,#7984,#7985,#7986,#7987,
#7988,#7989,#7990,#7991,#7992,#7993,#7994),.UNSPECIFIED.,.F.,.F.,(4,3,3,
3,3,3,3,3,3,3,3,3,3,3,3,3,3,3,3,3,3,3,3,3,3,3,3,3,3,3,3,3,3,3,3,3,3,3,3,
3,3,3,3,3,3,3,3,3,3,3,3,3,3,3,3,3,3,3,3,3,3,3,3,3,4),(-211.436685207534,
-211.338097456741,-211.239554137195,-211.141023824873,-211.042475117638,
-210.943815967523,-210.845090459821,-210.746205349484,-210.721663224119,
-210.621979658127,-210.522439309991,-210.422507190712,-210.323146485882,
-210.223818721299,-210.124493435201,-210.02411566534,-209.924645730114,
-209.823814042936,-209.722982355758,-209.623298789759,-209.523758441616,
-209.423826322339,-209.324465617503,-209.225137852914,-209.12581256681,
-209.025434796957,-208.925964861725,-208.825133174561,-208.724301487397,
-208.624617921371,-208.5250775732,-208.425145453929,-208.325784749064,-208.226456984446,
-208.127131698313,-208.026753928494,-207.927283993232,-207.826452306134,
-207.725620619036,-207.625937053027,-207.526396704874,-207.426464585599,
-207.327103880753,-207.227776116154,-207.128450830039,-207.028073060198,
-206.928603124955,-206.827771437816,-206.726939750676,-206.627256184665,
-206.527715836509,-206.427783717235,-206.328423012386,-206.229095247784,
-206.129769961667,-206.029392191829,-205.929922256584,-205.829090569449,
-205.728258882315,-205.626382795805,-205.524672889404,-205.423136082282,
-205.32170108951,-205.220351211035,-205.153499900354),.UNSPECIFIED.);
#747=B_SPLINE_CURVE_WITH_KNOTS('',3,(#7996,#7997,#7998,#7999,#8000,#8001,
#8002,#8003,#8004,#8005),.UNSPECIFIED.,.F.,.F.,(4,1,1,1,1,1,1,4),(-205.153494314817,
-204.729578013954,-203.730897145593,-202.732216277232,-201.733535408872,
-200.734854540511,-199.73617367215,-198.870314593174),.UNSPECIFIED.);
#748=B_SPLINE_CURVE_WITH_KNOTS('',3,(#8007,#8008,#8009,#8010,#8011,#8012,
#8013,#8014,#8015,#8016,#8017),.UNSPECIFIED.,.F.,.F.,(4,1,1,1,1,1,1,1,4),
(-198.870314593174,-198.737492803789,-197.738811935429,-196.740131067068,
-195.741450198707,-194.742769330346,-193.744088461986,-192.745407593625,
-192.587129285995),.UNSPECIFIED.);
#749=B_SPLINE_CURVE_WITH_KNOTS('',3,(#8019,#8020,#8021,#8022,#8023,#8024,
#8025,#8026,#8027,#8028),.UNSPECIFIED.,.F.,.F.,(4,1,1,1,1,1,1,4),(-192.587129285995,
-191.746726725264,-190.748045856903,-189.749364988543,-188.750684120182,
-187.752003251821,-186.75332238346,-186.303943978815),.UNSPECIFIED.);
#750=B_SPLINE_CURVE_WITH_KNOTS('',3,(#8030,#8031,#8032,#8033,#8034,#8035,
#8036,#8037,#8038,#8039),.UNSPECIFIED.,.F.,.F.,(4,1,1,1,1,1,1,4),(-186.303943978815,
-185.7546415151,-184.755960646739,-183.757279778378,-182.758598910017,-181.759918041657,
-180.761237173296,-180.020758671636),.UNSPECIFIED.);
#751=B_SPLINE_CURVE_WITH_KNOTS('',3,(#8041,#8042,#8043,#8044,#8045,#8046,
#8047,#8048,#8049,#8050,#8051,#8052,#8053,#8054,#8055,#8056,#8057,#8058,
#8059,#8060,#8061,#8062,#8063,#8064,#8065,#8066,#8067,#8068,#8069,#8070,
#8071,#8072,#8073,#8074,#8075,#8076,#8077,#8078,#8079,#8080,#8081,#8082,
#8083,#8084,#8085,#8086,#8087,#8088,#8089,#8090,#8091,#8092,#8093,#8094,
#8095,#8096,#8097,#8098,#8099,#8100,#8101,#8102,#8103,#8104,#8105,#8106,
#8107,#8108,#8109,#8110,#8111,#8112,#8113,#8114,#8115,#8116,#8117,#8118,
#8119,#8120,#8121,#8122,#8123,#8124,#8125,#8126,#8127,#8128,#8129,#8130,
#8131,#8132,#8133,#8134,#8135,#8136,#8137,#8138,#8139,#8140,#8141,#8142,
#8143,#8144,#8145,#8146,#8147,#8148,#8149,#8150,#8151,#8152,#8153,#8154,
#8155,#8156,#8157,#8158,#8159,#8160,#8161,#8162,#8163,#8164,#8165,#8166,
#8167,#8168,#8169,#8170,#8171,#8172,#8173,#8174,#8175,#8176,#8177,#8178,
#8179,#8180,#8181,#8182,#8183,#8184,#8185,#8186,#8187,#8188,#8189,#8190,
#8191,#8192,#8193,#8194,#8195,#8196,#8197,#8198,#8199,#8200,#8201,#8202,
#8203,#8204,#8205,#8206,#8207,#8208,#8209,#8210,#8211,#8212,#8213,#8214,
#8215,#8216,#8217,#8218,#8219,#8220,#8221,#8222,#8223,#8224,#8225,#8226,
#8227,#8228,#8229,#8230),.UNSPECIFIED.,.F.,.F.,(4,3,3,3,3,3,3,3,3,3,3,3,
3,3,3,3,3,3,3,3,3,3,3,3,3,3,3,3,3,3,3,3,3,3,3,3,3,3,3,3,3,3,3,3,3,3,3,3,
3,3,3,3,3,3,3,3,3,3,3,3,3,3,3,4),(-180.020758515293,-179.891657410114,-179.762556304935,
-179.662872738923,-179.563332390766,-179.463400271492,-179.364039566642,
-179.264711802039,-179.16538651592,-179.065008746084,-178.965538810837,
-178.864707123705,-178.763875436574,-178.664191870561,-178.564651522405,
-178.464719403131,-178.36535869828,-178.266030933677,-178.166705647558,
-178.066327877722,-177.966857942475,-177.866026255345,-177.765194568214,
-177.665511002201,-177.565970654044,-177.46603853477,-177.366677829919,
-177.267350065316,-177.168024779197,-177.067647009361,-176.968177074114,
-176.867345386983,-176.766513699853,-176.66683013384,-176.567289785683,
-176.467357666409,-176.367996961558,-176.268669196955,-176.169343910836,
-176.068966141,-175.969496205752,-175.868664518622,-175.767832831492,-175.668149265479,
-175.568608917322,-175.468676798048,-175.369316093197,-175.269988328594,
-175.170663042475,-175.070285272639,-174.970815337392,-174.869983650261,
-174.769151963131,-174.669468397118,-174.569928048962,-174.469995929688,
-174.370635224837,-174.271307460234,-174.171982174115,-174.071604404279,
-173.972134469032,-173.871302781902,-173.770471094771,-173.737573364456),
 .UNSPECIFIED.);
#752=B_SPLINE_CURVE_WITH_KNOTS('',3,(#8232,#8233,#8234,#8235,#8236,#8237,
#8238,#8239,#8240,#8241),.UNSPECIFIED.,.F.,.F.,(4,1,1,1,1,1,1,4),(-173.737568886119,
-172.77179022641,-171.773109358049,-170.774428489688,-169.775747621328,
-168.777066752967,-167.778385884606,-167.454394954544),.UNSPECIFIED.);
#753=B_SPLINE_CURVE_WITH_KNOTS('',3,(#8243,#8244,#8245,#8246,#8247,#8248,
#8249,#8250,#8251,#8252,#8253,#8254,#8255,#8256,#8257,#8258,#8259,#8260,
#8261,#8262,#8263,#8264,#8265,#8266,#8267,#8268,#8269,#8270,#8271,#8272,
#8273,#8274,#8275,#8276,#8277,#8278,#8279,#8280,#8281,#8282,#8283,#8284,
#8285,#8286,#8287,#8288,#8289,#8290,#8291,#8292,#8293,#8294,#8295,#8296,
#8297,#8298,#8299,#8300,#8301,#8302,#8303,#8304,#8305,#8306,#8307,#8308,
#8309,#8310,#8311,#8312,#8313,#8314,#8315,#8316,#8317,#8318,#8319,#8320,
#8321,#8322,#8323,#8324,#8325,#8326,#8327,#8328,#8329,#8330,#8331,#8332,
#8333,#8334,#8335,#8336,#8337,#8338,#8339,#8340,#8341,#8342,#8343,#8344,
#8345,#8346,#8347,#8348,#8349,#8350,#8351,#8352,#8353,#8354,#8355,#8356,
#8357,#8358,#8359,#8360,#8361,#8362,#8363,#8364,#8365,#8366,#8367,#8368,
#8369,#8370,#8371,#8372,#8373,#8374,#8375,#8376,#8377,#8378,#8379,#8380,
#8381,#8382,#8383,#8384,#8385,#8386,#8387,#8388,#8389,#8390,#8391,#8392,
#8393,#8394,#8395,#8396,#8397,#8398,#8399,#8400,#8401,#8402,#8403,#8404,
#8405,#8406,#8407,#8408,#8409,#8410,#8411,#8412,#8413,#8414,#8415,#8416,
#8417,#8418,#8419,#8420,#8421,#8422,#8423,#8424,#8425,#8426,#8427,#8428,
#8429,#8430,#8431,#8432),.UNSPECIFIED.,.F.,.F.,(4,3,3,3,3,3,3,3,3,3,3,3,
3,3,3,3,3,3,3,3,3,3,3,3,3,3,3,3,3,3,3,3,3,3,3,3,3,3,3,3,3,3,3,3,3,3,3,3,
3,3,3,3,3,3,3,3,3,3,3,3,3,3,3,4),(-167.454388057277,-167.355266653173,-167.256167295289,
-167.157059319171,-167.057841966077,-166.958568556428,-166.859113028564,
-166.779705016245,-166.680021450233,-166.580481102076,-166.480548982802,
-166.381188277952,-166.281860513349,-166.18253522723,-166.082157457394,
-165.982687522147,-165.881855835016,-165.781024147885,-165.681340581872,
-165.581800233715,-165.481868114441,-165.382507409591,-165.283179644987,
-165.183854358868,-165.083476589032,-164.984006653785,-164.883174966655,
-164.782343279524,-164.682659713511,-164.583119365354,-164.48318724608,
-164.383826541229,-164.284498776625,-164.185173490506,-164.08479572067,
-163.985325785423,-163.884494098293,-163.783662411163,-163.68397884515,
-163.584438496993,-163.484506377719,-163.385145672868,-163.285817908265,
-163.186492622146,-163.08611485231,-162.986644917063,-162.885813229932,
-162.784981542802,-162.685297976789,-162.585757628632,-162.485825509358,
-162.386464804508,-162.287137039905,-162.187811753786,-162.08743398395,
-161.987964048704,-161.887132361573,-161.786300674442,-161.685575317288,
-161.585001767063,-161.481552012821,-161.381207694737,-161.276205222417,
-161.171202750097),.UNSPECIFIED.);
#754=B_SPLINE_CURVE_WITH_KNOTS('',3,(#8434,#8435,#8436,#8437,#8438,#8439,
#8440,#8441,#8442,#8443),.UNSPECIFIED.,.F.,.F.,(4,1,1,1,1,1,1,4),(-161.171195349684,
-160.787619806081,-159.78893893772,-158.790258069359,-157.791577200999,
-156.792896332638,-155.794215464277,-154.888026240588),.UNSPECIFIED.);
#755=B_SPLINE_CURVE_WITH_KNOTS('',3,(#8445,#8446,#8447,#8448,#8449,#8450,
#8451,#8452,#8453,#8454,#8455,#8456,#8457,#8458,#8459,#8460,#8461,#8462,
#8463,#8464,#8465,#8466,#8467,#8468,#8469,#8470,#8471,#8472,#8473,#8474,
#8475,#8476,#8477,#8478,#8479,#8480,#8481,#8482,#8483,#8484,#8485,#8486,
#8487,#8488,#8489,#8490,#8491,#8492,#8493,#8494,#8495,#8496,#8497,#8498,
#8499,#8500,#8501,#8502,#8503,#8504,#8505,#8506,#8507,#8508,#8509,#8510,
#8511,#8512,#8513,#8514,#8515,#8516,#8517,#8518,#8519,#8520,#8521,#8522,
#8523,#8524,#8525,#8526,#8527,#8528,#8529,#8530,#8531,#8532,#8533,#8534,
#8535,#8536,#8537,#8538,#8539,#8540,#8541,#8542,#8543,#8544,#8545,#8546,
#8547,#8548,#8549,#8550,#8551,#8552,#8553,#8554,#8555,#8556,#8557,#8558,
#8559,#8560,#8561,#8562,#8563,#8564,#8565,#8566,#8567,#8568,#8569,#8570,
#8571,#8572,#8573,#8574,#8575,#8576,#8577,#8578,#8579,#8580,#8581,#8582,
#8583,#8584,#8585,#8586,#8587,#8588,#8589,#8590,#8591,#8592,#8593,#8594,
#8595,#8596,#8597,#8598,#8599,#8600,#8601,#8602,#8603,#8604,#8605,#8606,
#8607,#8608,#8609,#8610,#8611,#8612,#8613,#8614,#8615,#8616,#8617,#8618,
#8619,#8620,#8621,#8622,#8623,#8624,#8625,#8626,#8627,#8628,#8629,#8630,
#8631,#8632,#8633,#8634),.UNSPECIFIED.,.F.,.F.,(4,3,3,3,3,3,3,3,3,3,3,3,
3,3,3,3,3,3,3,3,3,3,3,3,3,3,3,3,3,3,3,3,3,3,3,3,3,3,3,3,3,3,3,3,3,3,3,3,
3,3,3,3,3,3,3,3,3,3,3,3,3,3,3,4),(-154.888017442918,-154.795534595916,-154.695851029908,
-154.596310681755,-154.49637856248,-154.397017857634,-154.297690093035,
-154.198364806921,-154.09798703708,-153.998517101837,-153.897685414697,
-153.796853727556,-153.697170161542,-153.597629813385,-153.497697694111,
-153.398336989259,-153.299009224655,-153.199683938535,-153.0993061687,-152.999836233452,
-152.899004546324,-152.798172859195,-152.698489293182,-152.598948945024,
-152.49901682575,-152.399656120899,-152.300328356295,-152.201003070175,
-152.10062530034,-152.001155365092,-151.900323677963,-151.799491990834,
-151.699808424822,-151.600268076665,-151.500335957391,-151.400975252541,
-151.301647487938,-151.202322201819,-151.101944431982,-151.002474496736,
-150.901642809604,-150.800811122473,-150.70112755646,-150.601587208303,
-150.501655089029,-150.402294384179,-150.302966619576,-150.203641333457,
-150.103263563621,-150.003793628374,-149.902961941243,-149.802130254113,
-149.7024466881,-149.602906339943,-149.502974220669,-149.403613515819,-149.304285751215,
-149.204960465096,-149.10458269526,-149.005112760013,-148.904281072882,
-148.803449385752,-148.660112359079,-148.604832135738),.UNSPECIFIED.);
#756=B_SPLINE_CURVE_WITH_KNOTS('',3,(#8636,#8637,#8638,#8639,#8640,#8641,
#8642,#8643,#8644,#8645,#8646,#8647,#8648,#8649,#8650,#8651,#8652,#8653,
#8654,#8655,#8656,#8657,#8658,#8659,#8660,#8661,#8662,#8663,#8664,#8665,
#8666,#8667,#8668,#8669,#8670,#8671,#8672,#8673,#8674,#8675,#8676,#8677,
#8678,#8679,#8680,#8681,#8682,#8683,#8684,#8685,#8686,#8687,#8688,#8689,
#8690,#8691,#8692,#8693,#8694,#8695,#8696,#8697,#8698,#8699,#8700,#8701,
#8702,#8703,#8704,#8705,#8706,#8707,#8708,#8709,#8710,#8711,#8712,#8713,
#8714,#8715,#8716,#8717,#8718,#8719,#8720,#8721,#8722,#8723,#8724,#8725,
#8726,#8727,#8728,#8729,#8730,#8731,#8732,#8733,#8734,#8735,#8736,#8737,
#8738,#8739,#8740,#8741,#8742,#8743,#8744,#8745,#8746,#8747,#8748,#8749,
#8750,#8751,#8752,#8753,#8754,#8755,#8756,#8757,#8758,#8759,#8760,#8761,
#8762,#8763,#8764,#8765,#8766,#8767,#8768,#8769,#8770,#8771,#8772,#8773,
#8774,#8775,#8776,#8777,#8778,#8779,#8780,#8781,#8782,#8783,#8784,#8785,
#8786,#8787,#8788,#8789,#8790,#8791,#8792,#8793,#8794,#8795,#8796,#8797,
#8798,#8799,#8800,#8801,#8802,#8803,#8804,#8805,#8806,#8807,#8808,#8809,
#8810,#8811,#8812,#8813,#8814,#8815,#8816,#8817,#8818,#8819,#8820,#8821,
#8822,#8823,#8824,#8825,#8826,#8827,#8828),.UNSPECIFIED.,.F.,.F.,(4,3,3,
3,3,3,3,3,3,3,3,3,3,3,3,3,3,3,3,3,3,3,3,3,3,3,3,3,3,3,3,3,3,3,3,3,3,3,3,
3,3,3,3,3,3,3,3,3,3,3,3,3,3,3,3,3,3,3,3,3,3,3,3,3,4),(-148.604832135393,
-148.504824183143,-148.406857804993,-148.308940024735,-148.211038772092,
-148.109471208417,-148.011447515633,-147.913357694361,-147.815116756516,
-147.804768517391,-147.705084951378,-147.605544603221,-147.505612483947,
-147.406251779096,-147.306924014493,-147.207598728373,-147.107220958538,
-147.00775102329,-146.90691933616,-146.80608764903,-146.706404083018,-146.606863734861,
-146.506931615587,-146.407570910736,-146.308243146133,-146.208917860014,
-146.108540090178,-146.009070154931,-145.908238467801,-145.80740678067,
-145.707723214657,-145.6081828665,-145.508250747226,-145.408890042376,-145.309562277772,
-145.210236991653,-145.109859221817,-145.01038928657,-144.90955759944,-144.808725912309,
-144.709042346296,-144.609501998139,-144.509569878865,-144.410209174014,
-144.310881409411,-144.211556123291,-144.111178353456,-144.011708418208,
-143.910876731078,-143.810045043948,-143.710361477935,-143.610821129778,
-143.510889010504,-143.411528305654,-143.31220054105,-143.212875254932,
-143.112497485096,-143.013027549848,-142.912195862718,-142.811364175587,
-142.70609042818,-142.601127558756,-142.496352275949,-142.391824202702,
-142.321646828766),.UNSPECIFIED.);
#757=B_SPLINE_CURVE_WITH_KNOTS('',3,(#8830,#8831,#8832,#8833,#8834,#8835,
#8836,#8837,#8838,#8839,#8840,#8841,#8842,#8843,#8844,#8845,#8846,#8847,
#8848,#8849,#8850,#8851,#8852,#8853,#8854,#8855,#8856,#8857,#8858,#8859,
#8860,#8861,#8862,#8863,#8864,#8865,#8866,#8867,#8868,#8869,#8870,#8871,
#8872,#8873,#8874,#8875,#8876,#8877,#8878,#8879,#8880,#8881,#8882,#8883,
#8884,#8885,#8886,#8887,#8888,#8889,#8890,#8891,#8892,#8893,#8894,#8895,
#8896,#8897,#8898,#8899,#8900,#8901,#8902,#8903,#8904,#8905,#8906,#8907,
#8908,#8909,#8910,#8911,#8912,#8913,#8914,#8915,#8916,#8917,#8918,#8919,
#8920,#8921,#8922,#8923,#8924,#8925,#8926,#8927,#8928,#8929,#8930,#8931,
#8932,#8933,#8934,#8935,#8936,#8937,#8938,#8939,#8940,#8941,#8942,#8943,
#8944,#8945,#8946,#8947,#8948,#8949,#8950,#8951,#8952,#8953,#8954,#8955,
#8956,#8957,#8958,#8959,#8960,#8961,#8962,#8963,#8964,#8965,#8966,#8967,
#8968,#8969,#8970,#8971,#8972,#8973,#8974,#8975,#8976,#8977,#8978,#8979,
#8980,#8981,#8982,#8983,#8984,#8985,#8986,#8987,#8988,#8989,#8990,#8991,
#8992,#8993,#8994,#8995,#8996,#8997,#8998,#8999,#9000,#9001,#9002,#9003,
#9004,#9005,#9006,#9007,#9008,#9009,#9010,#9011,#9012,#9013,#9014,#9015,
#9016,#9017,#9018,#9019),.UNSPECIFIED.,.F.,.F.,(4,3,3,3,3,3,3,3,3,3,3,3,
3,3,3,3,3,3,3,3,3,3,3,3,3,3,3,3,3,3,3,3,3,3,3,3,3,3,3,3,3,3,3,3,3,3,3,3,
3,3,3,3,3,3,3,3,3,3,3,3,3,3,3,4),(-142.321646828558,-142.218012990877,-142.114115387984,
-142.01008454749,-141.905772693495,-141.812683307227,-141.712999741214,
-141.613459393057,-141.513527273783,-141.414166568932,-141.314838804328,
-141.215513518209,-141.115135748373,-141.015665813125,-140.914834125996,
-140.814002438866,-140.714318872853,-140.614778524696,-140.514846405422,
-140.415485700571,-140.316157935968,-140.216832649849,-140.116454880013,
-140.016984944766,-139.916153257635,-139.815321570505,-139.715638004492,
-139.616097656335,-139.516165537061,-139.41680483221,-139.317477067607,
-139.218151781488,-139.117774011652,-139.018304076405,-138.917472389274,
-138.816640702144,-138.716957136131,-138.617416787974,-138.517484668701,
-138.41812396385,-138.318796199247,-138.219470913128,-138.119093143292,
-138.019623208045,-137.918791520915,-137.817959833784,-137.718276267771,
-137.618735919614,-137.51880380034,-137.419443095489,-137.320115330886,
-137.220790044767,-137.120412274931,-137.020942339684,-136.920110652553,
-136.819278965423,-136.720993989767,-136.622836098362,-136.524773061268,
-136.426772772098,-136.328765941481,-136.230762332266,-136.132657937408,
-136.038461521379),.UNSPECIFIED.);
#758=B_SPLINE_CURVE_WITH_KNOTS('',3,(#9021,#9022,#9023,#9024,#9025,#9026,
#9027,#9028,#9029,#9030,#9031),.UNSPECIFIED.,.F.,.F.,(4,1,1,1,1,1,1,1,4),
(-136.038461521379,-135.820598097062,-134.821917228701,-133.823236360341,
-132.82455549198,-131.825874623619,-130.827193755258,-129.828512886898,
-129.755276214199),.UNSPECIFIED.);
#759=B_SPLINE_CURVE_WITH_KNOTS('',3,(#9033,#9034,#9035,#9036,#9037,#9038,
#9039,#9040,#9041,#9042,#9043,#9044,#9045,#9046,#9047,#9048,#9049,#9050,
#9051,#9052,#9053,#9054,#9055,#9056,#9057,#9058,#9059,#9060,#9061,#9062,
#9063,#9064,#9065,#9066,#9067,#9068,#9069,#9070,#9071,#9072,#9073,#9074,
#9075,#9076,#9077,#9078,#9079,#9080,#9081,#9082,#9083,#9084,#9085,#9086,
#9087,#9088,#9089,#9090,#9091,#9092,#9093,#9094,#9095,#9096,#9097,#9098,
#9099,#9100,#9101,#9102,#9103,#9104,#9105,#9106,#9107,#9108,#9109,#9110,
#9111,#9112,#9113,#9114,#9115,#9116,#9117,#9118,#9119,#9120,#9121,#9122,
#9123,#9124,#9125,#9126,#9127,#9128,#9129,#9130,#9131,#9132,#9133,#9134,
#9135,#9136,#9137,#9138,#9139,#9140,#9141,#9142,#9143,#9144,#9145,#9146,
#9147,#9148,#9149,#9150,#9151,#9152,#9153,#9154,#9155,#9156,#9157,#9158,
#9159,#9160,#9161,#9162,#9163,#9164,#9165,#9166,#9167,#9168,#9169,#9170,
#9171,#9172,#9173,#9174,#9175,#9176,#9177,#9178,#9179,#9180,#9181,#9182,
#9183,#9184,#9185,#9186,#9187,#9188,#9189,#9190,#9191,#9192,#9193,#9194,
#9195,#9196,#9197,#9198,#9199,#9200,#9201,#9202,#9203,#9204,#9205,#9206,
#9207,#9208,#9209,#9210,#9211,#9212,#9213,#9214,#9215,#9216,#9217,#9218,
#9219,#9220,#9221,#9222,#9223,#9224,#9225),.UNSPECIFIED.,.F.,.F.,(4,3,3,
3,3,3,3,3,3,3,3,3,3,3,3,3,3,3,3,3,3,3,3,3,3,3,3,3,3,3,3,3,3,3,3,3,3,3,3,
3,3,3,3,3,3,3,3,3,3,3,3,3,3,3,3,3,3,3,3,3,3,3,3,3,4),(-129.755276214199,
-129.656647030661,-129.553295154146,-129.45490538759,-129.356567260123,
-129.25824908595,-129.159919208572,-129.061485240347,-128.962990381182,
-128.864336282513,-128.829832018537,-128.730148452524,-128.630608104367,
-128.530675985093,-128.431315280243,-128.331987515639,-128.23266222952,
-128.132284459684,-128.032814524437,-127.931982837306,-127.831151150176,
-127.731467584163,-127.631927236006,-127.531995116732,-127.432634411881,
-127.333306647277,-127.233981361158,-127.133603591322,-127.034133656075,
-126.933301968945,-126.832470281815,-126.732786715803,-126.633246367646,
-126.533314248372,-126.433953543522,-126.334625778918,-126.2353004928,-126.134922722964,
-126.035452787717,-125.934621100586,-125.833789413455,-125.734105847442,
-125.634565499285,-125.534633380011,-125.43527267516,-125.335944910557,
-125.236619624438,-125.136241854602,-125.036771919355,-124.935940232224,
-124.835108545094,-124.735424979081,-124.635884630923,-124.53595251165,
-124.436591806799,-124.337264042195,-124.237938756076,-124.13756098624,
-124.038091050993,-123.937259363863,-123.836427676733,-123.722636290486,
-123.609316906763,-123.496796562164,-123.472090907255),.UNSPECIFIED.);
#760=B_SPLINE_CURVE_WITH_KNOTS('',3,(#9227,#9228,#9229,#9230,#9231,#9232,
#9233,#9234,#9235,#9236,#9237,#9238,#9239,#9240,#9241,#9242,#9243,#9244,
#9245,#9246,#9247,#9248,#9249,#9250,#9251,#9252,#9253,#9254,#9255,#9256,
#9257,#9258,#9259,#9260,#9261,#9262,#9263,#9264,#9265,#9266,#9267,#9268,
#9269,#9270,#9271,#9272,#9273,#9274,#9275,#9276,#9277,#9278,#9279,#9280,
#9281,#9282,#9283,#9284,#9285,#9286,#9287,#9288,#9289,#9290,#9291,#9292,
#9293,#9294,#9295,#9296,#9297,#9298,#9299,#9300,#9301,#9302,#9303,#9304,
#9305,#9306,#9307,#9308,#9309,#9310,#9311,#9312,#9313,#9314,#9315,#9316,
#9317,#9318,#9319,#9320,#9321,#9322,#9323,#9324,#9325,#9326,#9327,#9328,
#9329,#9330,#9331,#9332,#9333,#9334,#9335,#9336,#9337,#9338,#9339,#9340,
#9341,#9342,#9343,#9344,#9345,#9346,#9347,#9348,#9349,#9350,#9351,#9352,
#9353,#9354,#9355,#9356,#9357,#9358,#9359,#9360,#9361,#9362,#9363,#9364,
#9365,#9366,#9367,#9368,#9369,#9370,#9371,#9372,#9373,#9374,#9375,#9376,
#9377,#9378,#9379,#9380,#9381,#9382,#9383,#9384,#9385,#9386,#9387,#9388,
#9389,#9390,#9391,#9392,#9393,#9394,#9395,#9396,#9397,#9398,#9399,#9400,
#9401,#9402,#9403,#9404,#9405,#9406,#9407,#9408,#9409,#9410,#9411,#9412,
#9413,#9414,#9415,#9416,#9417,#9418,#9419),.UNSPECIFIED.,.F.,.F.,(4,3,3,
3,3,3,3,3,3,3,3,3,3,3,3,3,3,3,3,3,3,3,3,3,3,3,3,3,3,3,3,3,3,3,3,3,3,3,3,
3,3,3,3,3,3,3,3,3,3,3,3,3,3,3,3,3,3,3,3,3,3,3,3,3,4),(-123.47209090702,
-123.372238927569,-123.272382020996,-123.172490797704,-123.072468036,-122.972368751522,
-122.872092706752,-122.837746808372,-122.73806324236,-122.638522894203,
-122.538590774929,-122.439230070079,-122.339902305476,-122.240577019357,
-122.140199249521,-122.040729314274,-121.939897627143,-121.839065940012,
-121.739382373999,-121.639842025842,-121.539909906568,-121.440549201717,
-121.341221437114,-121.241896150995,-121.141518381159,-121.042048445912,
-120.941216758782,-120.840385071651,-120.740701505638,-120.641161157481,
-120.541229038207,-120.441868333356,-120.342540568752,-120.243215282633,
-120.142837512797,-120.04336757755,-119.94253589042,-119.84170420329,-119.742020637277,
-119.64248028912,-119.542548169846,-119.443187464996,-119.343859700392,
-119.244534414273,-119.144156644437,-119.04468670919,-118.943855022059,
-118.843023334929,-118.743339768917,-118.64379942076,-118.543867301486,
-118.444506596635,-118.345178832032,-118.245853545913,-118.145475776077,
-118.04600584083,-117.9451741537,-117.844342466569,-117.744526295241,-117.644852015344,
-117.545289197132,-117.445806010149,-117.3463701507,-117.246927715914,-117.18890559984),
 .UNSPECIFIED.);
#761=B_SPLINE_CURVE_WITH_KNOTS('',3,(#9421,#9422,#9423,#9424,#9425,#9426,
#9427,#9428,#9429,#9430,#9431,#9432,#9433,#9434,#9435,#9436,#9437,#9438,
#9439,#9440,#9441,#9442,#9443,#9444,#9445,#9446,#9447,#9448,#9449,#9450,
#9451,#9452,#9453,#9454,#9455,#9456,#9457,#9458,#9459,#9460,#9461,#9462,
#9463,#9464,#9465,#9466,#9467,#9468,#9469,#9470,#9471,#9472,#9473,#9474,
#9475,#9476,#9477,#9478,#9479,#9480,#9481,#9482,#9483,#9484,#9485,#9486,
#9487,#9488,#9489,#9490,#9491,#9492,#9493,#9494,#9495,#9496,#9497,#9498,
#9499,#9500,#9501,#9502,#9503,#9504,#9505,#9506,#9507,#9508,#9509,#9510,
#9511,#9512,#9513,#9514,#9515,#9516,#9517,#9518,#9519,#9520,#9521,#9522,
#9523,#9524,#9525,#9526,#9527,#9528,#9529,#9530,#9531,#9532,#9533,#9534,
#9535,#9536,#9537,#9538,#9539,#9540,#9541,#9542,#9543,#9544,#9545,#9546,
#9547,#9548,#9549,#9550,#9551,#9552,#9553,#9554,#9555,#9556,#9557,#9558,
#9559,#9560,#9561,#9562,#9563,#9564,#9565,#9566,#9567,#9568,#9569,#9570,
#9571,#9572,#9573,#9574,#9575,#9576,#9577,#9578,#9579,#9580,#9581,#9582,
#9583,#9584,#9585,#9586,#9587,#9588,#9589,#9590,#9591,#9592,#9593,#9594,
#9595,#9596,#9597,#9598,#9599,#9600,#9601,#9602,#9603,#9604,#9605,#9606,
#9607,#9608,#9609,#9610),.UNSPECIFIED.,.F.,.F.,(4,3,3,3,3,3,3,3,3,3,3,3,
3,3,3,3,3,3,3,3,3,3,3,3,3,3,3,3,3,3,3,3,3,3,3,3,3,3,3,3,3,3,3,3,3,3,3,3,
3,3,3,3,3,3,3,3,3,3,3,3,3,3,3,4),(-117.188905599613,-117.074247201759,-116.958487635636,
-116.845661598208,-116.745978032195,-116.646437684038,-116.546505564764,
-116.447144859913,-116.347817095309,-116.24849180919,-116.148114039354,
-116.048644104107,-115.947812416977,-115.846980729847,-115.747297163834,
-115.647756815677,-115.547824696403,-115.448463991552,-115.349136226949,
-115.24981094083,-115.149433170994,-115.049963235746,-114.949131548616,
-114.848299861486,-114.748616295473,-114.649075947317,-114.549143828043,
-114.449783123192,-114.350455358589,-114.251130072471,-114.150752302634,
-114.051282367388,-113.950450680257,-113.849618993126,-113.749935427113,
-113.650395078956,-113.550462959682,-113.451102254832,-113.351774490228,
-113.252449204109,-113.152071434273,-113.052601499026,-112.951769811895,
-112.850938124765,-112.751254558752,-112.651714210595,-112.551782091321,
-112.45242138647,-112.353093621866,-112.253768335747,-112.153390565911,
-112.053920630664,-111.953088943534,-111.852257256404,-111.753361661131,
-111.654608517859,-111.555968937272,-111.457390389855,-111.358841414297,
-111.260290588098,-111.16164445216,-111.062946578368,-110.964086828485,
-110.905720292661),.UNSPECIFIED.);
#762=B_SPLINE_CURVE_WITH_KNOTS('',3,(#9612,#9613,#9614,#9615,#9616,#9617,
#9618,#9619,#9620,#9621,#9622,#9623),.UNSPECIFIED.,.F.,.F.,(4,2,1,1,1,1,
1,1,4),(-110.905720292661,-110.853576388043,-109.854895519683,-108.856214651322,
-107.857533782961,-106.8588529146,-105.86017204624,-104.861491177879,-104.622534985481),
 .UNSPECIFIED.);
#763=B_SPLINE_CURVE_WITH_KNOTS('',3,(#9625,#9626,#9627,#9628,#9629,#9630,
#9631,#9632,#9633,#9634),.UNSPECIFIED.,.F.,.F.,(4,1,1,1,1,1,1,4),(-104.622534985481,
-103.862810309518,-102.864129441157,-101.865448572797,-100.866767704436,
-99.8680868360751,-98.8694059677144,-98.3393496783013),.UNSPECIFIED.);
#764=B_SPLINE_CURVE_WITH_KNOTS('',3,(#9636,#9637,#9638,#9639,#9640,#9641,
#9642,#9643,#9644,#9645,#9646,#9647,#9648,#9649,#9650,#9651,#9652,#9653,
#9654,#9655,#9656,#9657,#9658,#9659,#9660,#9661,#9662,#9663,#9664,#9665,
#9666,#9667,#9668,#9669,#9670,#9671,#9672,#9673,#9674,#9675,#9676,#9677,
#9678,#9679,#9680,#9681,#9682,#9683,#9684,#9685,#9686,#9687,#9688,#9689,
#9690,#9691,#9692,#9693,#9694,#9695,#9696,#9697,#9698,#9699,#9700,#9701,
#9702,#9703,#9704,#9705,#9706,#9707,#9708,#9709,#9710,#9711,#9712,#9713,
#9714,#9715,#9716,#9717,#9718,#9719,#9720,#9721,#9722,#9723,#9724,#9725,
#9726,#9727,#9728,#9729,#9730,#9731,#9732,#9733,#9734,#9735,#9736,#9737,
#9738,#9739,#9740,#9741,#9742,#9743,#9744,#9745,#9746,#9747,#9748,#9749,
#9750,#9751,#9752,#9753,#9754,#9755,#9756,#9757,#9758,#9759,#9760,#9761,
#9762,#9763,#9764,#9765,#9766,#9767,#9768,#9769,#9770,#9771,#9772,#9773,
#9774,#9775,#9776,#9777,#9778,#9779,#9780,#9781,#9782,#9783,#9784,#9785,
#9786,#9787,#9788,#9789,#9790,#9791,#9792,#9793,#9794,#9795,#9796,#9797,
#9798,#9799,#9800,#9801,#9802,#9803,#9804,#9805,#9806,#9807,#9808,#9809,
#9810,#9811,#9812,#9813,#9814,#9815,#9816,#9817,#9818,#9819,#9820,#9821,
#9822,#9823,#9824,#9825,#9826,#9827,#9828),.UNSPECIFIED.,.F.,.F.,(4,3,3,
3,3,3,3,3,3,3,3,3,3,3,3,3,3,3,3,3,3,3,3,3,3,3,3,3,3,3,3,3,3,3,3,3,3,3,3,
3,3,3,3,3,3,3,3,3,3,3,3,3,3,3,3,3,3,3,3,3,3,3,3,3,4),(-98.3393495114471,
-98.233881669341,-98.1280517505152,-98.0220294207556,-97.9156982804113,
-97.8707250993536,-97.7710415333408,-97.6715011851837,-97.5715690659099,
-97.4722083610592,-97.3728805964559,-97.2735553103369,-97.1731775405009,
-97.0737076052538,-96.9728759181233,-96.8720442309929,-96.7723606649801,
-96.6728203168229,-96.5728881975491,-96.4735274926984,-96.374199728095,
-96.2748744419759,-96.17449667214,-96.0750267368928,-95.9741950497625,-95.8733633626321,
-95.7736797966193,-95.6741394484622,-95.5742073291884,-95.4748466243377,
-95.3755188597344,-95.2761935736154,-95.1758158037794,-95.0763458685322,
-94.9755141814018,-94.8746824942714,-94.7749989282586,-94.6754585801015,
-94.5755264608276,-94.476165755977,-94.3768379913736,-94.2775127052546,
-94.1771349354186,-94.0776650001714,-93.976833313041,-93.8760016259106,
-93.7763180598978,-93.6767777117407,-93.5768455924669,-93.4774848876162,
-93.3781571230129,-93.2788318368939,-93.1784540670579,-93.0789841318107,
-92.9781524446803,-92.8773207575499,-92.7746762092464,-92.6766447659007,
-92.5787048057558,-92.4808241264331,-92.3829706052476,-92.2850696713238,
-92.1871405423995,-92.0890995979721,-92.0561643711217),.UNSPECIFIED.);
#765=B_SPLINE_CURVE_WITH_KNOTS('',3,(#9830,#9831,#9832,#9833,#9834,#9835,
#9836,#9837,#9838,#9839,#9840),.UNSPECIFIED.,.F.,.F.,(4,1,1,1,1,1,1,1,4),
(-92.0561643711217,-91.8786398891891,-90.8799590208284,-89.8812781524676,
-88.8825972841069,-87.8839164157461,-86.8852355473853,-85.8865546790246,
-85.7729790639421),.UNSPECIFIED.);
#766=B_SPLINE_CURVE_WITH_KNOTS('',3,(#9842,#9843,#9844,#9845,#9846,#9847,
#9848,#9849,#9850,#9851,#9852,#9853,#9854,#9855,#9856,#9857,#9858,#9859,
#9860,#9861,#9862,#9863,#9864,#9865,#9866,#9867,#9868,#9869,#9870,#9871,
#9872,#9873,#9874,#9875,#9876,#9877,#9878,#9879,#9880,#9881,#9882,#9883,
#9884,#9885,#9886,#9887,#9888,#9889,#9890,#9891,#9892,#9893,#9894,#9895,
#9896,#9897,#9898,#9899,#9900,#9901,#9902,#9903,#9904,#9905,#9906,#9907,
#9908,#9909,#9910,#9911,#9912,#9913,#9914,#9915,#9916,#9917,#9918,#9919,
#9920,#9921,#9922,#9923,#9924,#9925,#9926,#9927,#9928,#9929,#9930,#9931,
#9932,#9933,#9934,#9935,#9936,#9937,#9938,#9939,#9940,#9941,#9942,#9943,
#9944,#9945,#9946,#9947,#9948,#9949,#9950,#9951,#9952,#9953,#9954,#9955,
#9956,#9957,#9958,#9959,#9960,#9961,#9962,#9963,#9964,#9965,#9966,#9967,
#9968,#9969,#9970,#9971,#9972,#9973,#9974,#9975,#9976,#9977,#9978,#9979,
#9980,#9981,#9982,#9983,#9984,#9985,#9986,#9987,#9988,#9989,#9990,#9991,
#9992,#9993,#9994,#9995,#9996,#9997,#9998,#9999,#10000,#10001,#10002,#10003,
#10004,#10005,#10006,#10007,#10008,#10009,#10010,#10011,#10012,#10013,#10014,
#10015,#10016,#10017,#10018,#10019,#10020,#10021,#10022,#10023,#10024,#10025,
#10026,#10027,#10028,#10029,#10030,#10031),.UNSPECIFIED.,.F.,.F.,(4,3,3,
3,3,3,3,3,3,3,3,3,3,3,3,3,3,3,3,3,3,3,3,3,3,3,3,3,3,3,3,3,3,3,3,3,3,3,3,
3,3,3,3,3,3,3,3,3,3,3,3,3,3,3,3,3,3,3,3,3,3,3,3,4),(-85.7729790639421,-85.6747012370361,
-85.5763478087396,-85.4782825827934,-85.3802610142147,-85.2822511346314,
-85.1836568036395,-85.0855181919729,-84.9866960013183,-84.8878738106638,
-84.788190244651,-84.6886498964939,-84.5887177772201,-84.4893570723695,
-84.3900293077662,-84.2907040216472,-84.1903262518112,-84.090856316564,
-83.9900246294335,-83.8891929423031,-83.7895093762904,-83.6899690281336,
-83.5900369088597,-83.4906762040089,-83.3913484394057,-83.2920231532865,
-83.1916453834505,-83.0921754482033,-82.9913437610728,-82.8905120739423,
-82.7908285079295,-82.6912881597726,-82.5913560404987,-82.491995335648,
-82.3926675710447,-82.2933422849257,-82.1929645150897,-82.0934945798426,
-81.9926628927121,-81.8918312055816,-81.7921476395688,-81.6926072914119,
-81.592675172138,-81.4933144672874,-81.393986702684,-81.2946614165649,-81.1942836467289,
-81.0948137114817,-80.9939820243513,-80.8931503372209,-80.7934667712081,
-80.6939264230509,-80.5939943037771,-80.4946335989264,-80.3953058343231,
-80.2959805482041,-80.1956027783681,-80.096132843121,-79.9953011559905,
-79.8944694688601,-79.7841166760362,-79.6740971377985,-79.5646466108232,
-79.4897941881386),.UNSPECIFIED.);
#767=B_SPLINE_CURVE_WITH_KNOTS('',3,(#10033,#10034,#10035,#10036,#10037,
#10038,#10039,#10040,#10041,#10042),.UNSPECIFIED.,.F.,.F.,(4,1,1,1,1,1,
1,4),(-79.4897937567626,-78.8957886004994,-77.8971077321386,-76.8984268637779,
-75.8997459954171,-74.9010651270563,-73.9023842586956,-73.2066084495829),
 .UNSPECIFIED.);
#768=B_SPLINE_CURVE_WITH_KNOTS('',3,(#10044,#10045,#10046,#10047,#10048,
#10049,#10050,#10051,#10052,#10053,#10054,#10055,#10056,#10057,#10058,#10059,
#10060,#10061,#10062,#10063,#10064,#10065,#10066,#10067,#10068,#10069,#10070,
#10071,#10072,#10073,#10074,#10075,#10076,#10077,#10078,#10079,#10080,#10081,
#10082,#10083,#10084,#10085,#10086,#10087,#10088,#10089,#10090,#10091,#10092,
#10093,#10094,#10095,#10096,#10097,#10098,#10099,#10100,#10101,#10102,#10103,
#10104,#10105,#10106,#10107,#10108,#10109,#10110,#10111,#10112,#10113,#10114,
#10115,#10116,#10117,#10118,#10119,#10120,#10121,#10122,#10123,#10124,#10125,
#10126,#10127,#10128,#10129,#10130,#10131,#10132,#10133,#10134,#10135,#10136,
#10137,#10138,#10139,#10140,#10141,#10142,#10143,#10144,#10145,#10146,#10147,
#10148,#10149,#10150,#10151,#10152,#10153,#10154,#10155,#10156,#10157,#10158,
#10159,#10160,#10161,#10162,#10163,#10164,#10165,#10166,#10167,#10168,#10169,
#10170,#10171,#10172,#10173,#10174,#10175,#10176,#10177,#10178,#10179,#10180,
#10181,#10182,#10183,#10184,#10185,#10186,#10187,#10188,#10189,#10190,#10191,
#10192,#10193,#10194,#10195,#10196,#10197,#10198,#10199,#10200,#10201,#10202,
#10203,#10204,#10205,#10206,#10207,#10208,#10209,#10210,#10211,#10212,#10213,
#10214,#10215,#10216,#10217,#10218,#10219,#10220,#10221,#10222,#10223,#10224,
#10225,#10226,#10227,#10228,#10229,#10230,#10231,#10232,#10233),
 .UNSPECIFIED.,.F.,.F.,(4,3,3,3,3,3,3,3,3,3,3,3,3,3,3,3,3,3,3,3,3,3,3,3,
3,3,3,3,3,3,3,3,3,3,3,3,3,3,3,3,3,3,3,3,3,3,3,3,3,3,3,3,3,3,3,3,3,3,3,3,
3,3,3,4),(-73.2066082616887,-73.0873800102398,-72.9665362689588,-72.9037033903348,
-72.804019824322,-72.7044794761649,-72.6045473568911,-72.5051866520404,
-72.4058588874371,-72.306533601318,-72.2061558314821,-72.1066858962349,
-72.0058542091045,-71.9050225219741,-71.8053389559613,-71.7057986078042,
-71.6058664885303,-71.5065057836796,-71.4071780190763,-71.3078527329571,
-71.2074749631212,-71.108005027874,-71.0071733407436,-70.9063416536133,
-70.8066580876005,-70.7071177394434,-70.6071856201696,-70.5078249153189,
-70.4084971507156,-70.3091718645965,-70.2087940947605,-70.1093241595134,
-70.008492472383,-69.9076607852526,-69.8079772192398,-69.7084368710827,
-69.6085047518089,-69.5091440469582,-69.4098162823549,-69.3104909962358,
-69.2101132263998,-69.1106432911527,-69.0098116040222,-68.9089799168918,
-68.809296350879,-68.7097560027219,-68.609823883448,-68.5104631785974,-68.4111354139941,
-68.311810127875,-68.211432358039,-68.1119624227919,-68.0111307356615,-67.9102990485311,
-67.8108213082292,-67.7114866269179,-67.6122670665479,-67.5131103926434,
-67.4139858279942,-67.314862635178,-67.2156413232076,-67.116372598946,-67.0169246775773,
-66.9234231424034),.UNSPECIFIED.);
#769=B_SPLINE_CURVE_WITH_KNOTS('',3,(#10235,#10236,#10237,#10238,#10239,
#10240,#10241,#10242,#10243,#10244,#10245,#10246),.UNSPECIFIED.,.F.,.F.,
(4,2,1,1,1,1,1,1,4),(-66.9234231424034,-66.9116181801703,-65.9129373118096,
-64.9142564434488,-63.9155755750881,-62.9168947067273,-61.9182138383666,
-60.9195329700058,-60.6402420696886),.UNSPECIFIED.);
#770=B_SPLINE_CURVE_WITH_KNOTS('',3,(#10248,#10249,#10250,#10251,#10252,
#10253,#10254,#10255,#10256,#10257,#10258,#10259,#10260,#10261,#10262,#10263,
#10264,#10265,#10266,#10267,#10268,#10269,#10270,#10271,#10272,#10273,#10274,
#10275,#10276,#10277,#10278,#10279,#10280,#10281,#10282,#10283,#10284,#10285,
#10286,#10287,#10288,#10289,#10290,#10291,#10292,#10293,#10294,#10295,#10296,
#10297,#10298,#10299,#10300,#10301,#10302,#10303,#10304,#10305,#10306,#10307,
#10308,#10309,#10310,#10311,#10312,#10313,#10314,#10315,#10316,#10317,#10318,
#10319,#10320,#10321,#10322,#10323,#10324,#10325,#10326,#10327,#10328,#10329,
#10330,#10331,#10332,#10333,#10334,#10335,#10336,#10337,#10338,#10339,#10340,
#10341,#10342,#10343,#10344,#10345,#10346,#10347,#10348,#10349,#10350,#10351,
#10352,#10353,#10354,#10355,#10356,#10357,#10358,#10359,#10360,#10361,#10362,
#10363,#10364,#10365,#10366,#10367,#10368,#10369,#10370,#10371,#10372,#10373,
#10374,#10375,#10376,#10377,#10378,#10379,#10380,#10381,#10382,#10383,#10384,
#10385,#10386,#10387,#10388,#10389,#10390,#10391,#10392,#10393,#10394,#10395,
#10396,#10397,#10398,#10399,#10400,#10401,#10402,#10403,#10404,#10405,#10406,
#10407,#10408,#10409,#10410,#10411,#10412,#10413,#10414,#10415,#10416,#10417,
#10418,#10419,#10420,#10421,#10422,#10423,#10424,#10425,#10426,#10427,#10428,
#10429,#10430,#10431,#10432,#10433,#10434,#10435,#10436,#10437,#10438,#10439,
#10440),.UNSPECIFIED.,.F.,.F.,(4,3,3,3,3,3,3,3,3,3,3,3,3,3,3,3,3,3,3,3,
3,3,3,3,3,3,3,3,3,3,3,3,3,3,3,3,3,3,3,3,3,3,3,3,3,3,3,3,3,3,3,3,3,3,3,3,
3,3,3,3,3,3,3,3,4),(-60.6402378352238,-60.541696652544,-60.4432021032873,
-60.3447227024354,-60.2462269890419,-60.1476223960021,-60.0489531987877,
-59.9501235071943,-59.9208521016451,-59.8211685356324,-59.7216281874753,
-59.6216960682015,-59.5223353633507,-59.4230075987475,-59.3236823126283,
-59.2233045427923,-59.1238346075451,-59.0230029204147,-58.9221712332843,
-58.8224876672716,-58.7229473191144,-58.6230151998405,-58.5236544949899,
-58.4243267303866,-58.3250014442675,-58.2246236744316,-58.1251537391845,
-58.024322052054,-57.9234903649236,-57.8238067989108,-57.7242664507537,
-57.6243343314799,-57.5249736266291,-57.4256458620259,-57.3263205759069,
-57.2259428060708,-57.1264728708238,-57.0256411836933,-56.9248094965628,
-56.8251259305499,-56.7255855823927,-56.6256534631189,-56.5262927582682,
-56.4269649936648,-56.3276397075457,-56.2272619377098,-56.1277920024627,
-56.0269603153324,-55.9261286282021,-55.8264450621894,-55.7269047140322,
-55.6269725947583,-55.5276118899076,-55.4282841253044,-55.3289588391855,
-55.2285810693494,-55.1291111341022,-55.0282794469718,-54.9274477598413,
-54.8254312965464,-54.7235829168215,-54.6219114837855,-54.5203441562718,
-54.4188669816396,-54.3570525280442),.UNSPECIFIED.);
#771=B_SPLINE_CURVE_WITH_KNOTS('',3,(#10442,#10443,#10444,#10445,#10446,
#10447,#10448,#10449,#10450,#10451),.UNSPECIFIED.,.F.,.F.,(4,1,1,1,1,1,
1,4),(-54.3570471904822,-53.9287668914806,-52.9300860231198,-51.9314051547591,
-50.9327242863983,-49.9340434180376,-48.9353625496768,-48.0738672208646),
 .UNSPECIFIED.);
#772=B_SPLINE_CURVE_WITH_KNOTS('',3,(#10453,#10454,#10455,#10456,#10457,
#10458,#10459,#10460,#10461,#10462,#10463),.UNSPECIFIED.,.F.,.F.,(4,1,1,
1,1,1,1,1,4),(-48.0738672208646,-47.9366816813161,-46.9380008129553,-45.9393199445946,
-44.9406390762338,-43.941958207873,-42.9432773395123,-41.9445964711515,
-41.790681913685),.UNSPECIFIED.);
#773=B_SPLINE_CURVE_WITH_KNOTS('',3,(#10465,#10466,#10467,#10468,#10469,
#10470,#10471,#10472,#10473,#10474),.UNSPECIFIED.,.F.,.F.,(4,1,1,1,1,1,
1,4),(-41.790681913685,-40.9459156027908,-39.94723473443,-38.9485538660693,
-37.9498729977085,-36.9511921293478,-35.952511260987,-35.5074966065054),
 .UNSPECIFIED.);
#774=B_SPLINE_CURVE_WITH_KNOTS('',3,(#10476,#10477,#10478,#10479,#10480,
#10481,#10482,#10483,#10484,#10485),.UNSPECIFIED.,.F.,.F.,(4,1,1,1,1,1,
1,4),(-35.5074966065054,-34.9538303926263,-33.9551495242656,-32.9564686559048,
-31.957787787544,-30.9591069191833,-29.9604260508225,-29.2243112993258),
 .UNSPECIFIED.);
#775=B_SPLINE_CURVE_WITH_KNOTS('',3,(#10487,#10488,#10489,#10490,#10491,
#10492,#10493,#10494,#10495,#10496,#10497,#10498,#10499,#10500,#10501,#10502,
#10503,#10504,#10505,#10506,#10507,#10508,#10509,#10510,#10511,#10512,#10513,
#10514,#10515,#10516,#10517,#10518,#10519,#10520,#10521,#10522,#10523,#10524,
#10525,#10526,#10527,#10528,#10529,#10530,#10531,#10532,#10533,#10534,#10535,
#10536,#10537,#10538,#10539,#10540,#10541,#10542,#10543,#10544,#10545,#10546,
#10547,#10548,#10549,#10550,#10551,#10552,#10553,#10554,#10555,#10556,#10557,
#10558,#10559,#10560,#10561,#10562,#10563,#10564,#10565,#10566,#10567,#10568,
#10569,#10570,#10571,#10572,#10573,#10574,#10575,#10576,#10577,#10578,#10579,
#10580,#10581,#10582,#10583,#10584,#10585,#10586,#10587,#10588,#10589,#10590,
#10591,#10592,#10593,#10594,#10595,#10596,#10597,#10598,#10599,#10600,#10601,
#10602,#10603,#10604,#10605,#10606,#10607,#10608,#10609,#10610,#10611,#10612,
#10613,#10614,#10615,#10616,#10617,#10618,#10619,#10620,#10621,#10622,#10623,
#10624,#10625,#10626,#10627,#10628,#10629,#10630,#10631,#10632,#10633,#10634,
#10635,#10636,#10637,#10638,#10639,#10640,#10641,#10642,#10643,#10644,#10645,
#10646,#10647,#10648,#10649,#10650,#10651,#10652,#10653,#10654,#10655,#10656,
#10657,#10658,#10659,#10660,#10661,#10662,#10663,#10664,#10665,#10666,#10667,
#10668,#10669,#10670,#10671,#10672,#10673,#10674,#10675,#10676),
 .UNSPECIFIED.,.F.,.F.,(4,3,3,3,3,3,3,3,3,3,3,3,3,3,3,3,3,3,3,3,3,3,3,3,
3,3,3,3,3,3,3,3,3,3,3,3,3,3,3,3,3,3,3,3,3,3,3,3,3,3,3,3,3,3,3,3,3,3,3,3,
3,3,3,4),(-29.2243111180069,-29.0930281502344,-28.9617451824618,-28.8620616164645,
-28.7625212683228,-28.6625891490451,-28.5632284442096,-28.4639006796212,
-28.364575393517,-28.264197623663,-28.1647276884302,-28.0638960012656,-27.963064314101,
-27.8633807481083,-27.7638403999717,-27.6639082806927,-27.5645475758629,
-27.4652198112804,-27.3658945251824,-27.2655167553219,-27.1660468200957,
-27.065215132918,-26.9643834457403,-26.8646998796295,-26.7651595313741,
-26.6652274121248,-26.565866707176,-26.4665389424749,-26.3672136562584,
-26.2668358865386,-26.167365951196,-26.0665342642878,-25.9657025773795,
-25.8660190114961,-25.7664786634679,-25.6665465441617,-25.5671858394381,
-25.4678580749609,-25.3685327889668,-25.2681550189798,-25.1686850838535,
-25.0678533964362,-24.9670217090188,-24.8673381430953,-24.7677977950291,
-24.6678656757327,-24.5685049709762,-24.4691772064682,-24.3698519204453,
-24.2694741504985,-24.1700042153487,-24.0691725280033,-23.968340840658,
-23.8686572739908,-23.7691169251773,-23.6691848060673,-23.5698241005602,
-23.4704963353019,-23.3711710485301,-23.2707932794719,-23.1713233435843,
-23.0704916579408,-22.9696599722973,-22.9411259921462),.UNSPECIFIED.);
#776=B_SPLINE_CURVE_WITH_KNOTS('',3,(#10678,#10679,#10680,#10681,#10682,
#10683,#10684,#10685,#10686,#10687,#10688,#10689,#10690,#10691,#10692,#10693,
#10694,#10695,#10696,#10697,#10698,#10699,#10700,#10701,#10702,#10703,#10704,
#10705,#10706,#10707,#10708,#10709,#10710,#10711,#10712,#10713,#10714,#10715,
#10716,#10717,#10718,#10719,#10720,#10721,#10722,#10723,#10724,#10725,#10726,
#10727,#10728,#10729,#10730,#10731,#10732,#10733,#10734,#10735,#10736,#10737,
#10738,#10739,#10740,#10741,#10742,#10743,#10744,#10745,#10746,#10747,#10748,
#10749,#10750,#10751,#10752,#10753,#10754,#10755,#10756,#10757,#10758,#10759,
#10760,#10761,#10762,#10763,#10764,#10765,#10766,#10767,#10768,#10769,#10770,
#10771,#10772,#10773,#10774,#10775,#10776,#10777,#10778,#10779,#10780,#10781,
#10782,#10783,#10784,#10785,#10786,#10787,#10788,#10789,#10790,#10791,#10792,
#10793,#10794,#10795,#10796,#10797,#10798,#10799,#10800,#10801,#10802,#10803,
#10804,#10805,#10806,#10807,#10808,#10809,#10810,#10811,#10812,#10813,#10814,
#10815,#10816,#10817,#10818,#10819,#10820,#10821,#10822,#10823,#10824,#10825,
#10826,#10827,#10828,#10829,#10830,#10831,#10832,#10833,#10834,#10835,#10836,
#10837,#10838,#10839,#10840,#10841,#10842,#10843,#10844,#10845,#10846,#10847,
#10848,#10849,#10850,#10851,#10852,#10853,#10854,#10855,#10856,#10857,#10858,
#10859,#10860,#10861,#10862,#10863,#10864,#10865,#10866,#10867),
 .UNSPECIFIED.,.F.,.F.,(4,3,3,3,3,3,3,3,3,3,3,3,3,3,3,3,3,3,3,3,3,3,3,3,
3,3,3,3,3,3,3,3,3,3,3,3,3,3,3,3,3,3,3,3,3,3,3,3,3,3,3,3,3,3,3,3,3,3,3,3,
3,3,3,4),(-22.9411259917379,-22.8419179935918,-22.7428514984844,-22.6438973639292,
-22.5450040344622,-22.4461404084451,-22.3472754222286,-22.2483111277133,
-22.1492963564552,-22.0501073736359,-21.9709791039365,-21.8712955381832,
-21.7717551902968,-21.6718230709567,-21.5724623664015,-21.4731346021024,
-21.3738093162956,-21.2734315461156,-21.1739616111974,-21.0731299233866,
-20.9722982355758,-20.8726146652961,-20.7730743128561,-20.6731421946509,
-20.5737814855096,-20.4744537166221,-20.3751284262311,-20.2747506614771,
-20.1752807220312,-20.0744490446231,-19.973617367215,-19.8739338090674,
-19.7743934687681,-19.6744613475288,-19.5751006504616,-19.4757728935969,
-19.3764476151617,-19.2760698360849,-19.17659990831,-19.0757682035822,-18.9749364988543,
-18.8752529321135,-18.7757125833021,-18.6757804642011,-18.5764197588777,
-18.4770919938704,-18.3777667074162,-18.2773889381855,-18.1779190027736,
-18.0770873166336,-17.9762556304935,-17.8765720373954,-17.777031662028,
-17.6770995495411,-17.5777388173754,-17.4784110254777,-17.3790857121216,
-17.2787079746244,-17.1792380125578,-17.0784063873453,-16.9775747621328,
-16.8588404756105,-16.7414263370442,-16.6579409003871),.UNSPECIFIED.);
#777=B_SPLINE_CURVE_WITH_KNOTS('',3,(#10869,#10870,#10871,#10872,#10873,
#10874,#10875,#10876,#10877,#10878),.UNSPECIFIED.,.F.,.F.,(4,1,1,1,1,1,
1,4),(-16.6579406849666,-15.978893893772,-14.9802130254113,-13.9815321570505,
-12.9828512886898,-11.984170420329,-10.9854895519683,-10.3747553777871),
 .UNSPECIFIED.);
#778=B_SPLINE_CURVE_WITH_KNOTS('',3,(#10879,#10880,#10881,#10882,#10883,
#10884,#10885,#10886,#10887,#10888),.UNSPECIFIED.,.F.,.F.,(4,1,1,1,1,1,
1,4),(-10.3747553777871,-9.98680868360752,-8.98812781524676,-7.98944694688601,
-6.99076607852526,-5.99208521016451,-4.99340434180376,-4.09157007060746),
 .UNSPECIFIED.);
#779=B_SPLINE_CURVE_WITH_KNOTS('',3,(#10892,#10893,#10894,#10895,#10896,
#10897,#10898,#10899,#10900,#10901,#10902,#10903,#10904,#10905,#10906,#10907,
#10908,#10909,#10910,#10911,#10912,#10913,#10914,#10915,#10916,#10917,#10918,
#10919,#10920,#10921,#10922,#10923,#10924,#10925,#10926,#10927,#10928,#10929,
#10930,#10931,#10932,#10933,#10934,#10935,#10936,#10937,#10938,#10939,#10940,
#10941,#10942,#10943,#10944,#10945,#10946,#10947,#10948,#10949,#10950,#10951,
#10952,#10953,#10954,#10955,#10956,#10957,#10958,#10959,#10960,#10961,#10962,
#10963,#10964,#10965,#10966,#10967,#10968,#10969,#10970,#10971,#10972,#10973,
#10974,#10975,#10976,#10977,#10978,#10979,#10980,#10981,#10982,#10983,#10984,
#10985,#10986,#10987,#10988,#10989,#10990,#10991,#10992,#10993,#10994,#10995,
#10996,#10997,#10998,#10999,#11000,#11001,#11002,#11003,#11004,#11005,#11006,
#11007,#11008,#11009,#11010,#11011,#11012,#11013,#11014,#11015,#11016,#11017,
#11018,#11019,#11020,#11021,#11022,#11023,#11024,#11025,#11026,#11027,#11028,
#11029,#11030,#11031,#11032,#11033,#11034,#11035,#11036,#11037,#11038,#11039,
#11040,#11041,#11042,#11043,#11044,#11045,#11046,#11047,#11048,#11049,#11050,
#11051,#11052,#11053,#11054,#11055,#11056,#11057,#11058,#11059,#11060,#11061,
#11062,#11063,#11064,#11065,#11066,#11067,#11068,#11069,#11070,#11071,#11072,
#11073,#11074,#11075,#11076,#11077,#11078,#11079,#11080,#11081,#11082,#11083,
#11084,#11085,#11086,#11087,#11088,#11089,#11090,#11091,#11092,#11093,#11094,
#11095,#11096,#11097,#11098,#11099,#11100,#11101,#11102,#11103,#11104,#11105,
#11106,#11107,#11108,#11109,#11110,#11111,#11112,#11113,#11114,#11115,#11116,
#11117,#11118,#11119,#11120,#11121,#11122,#11123,#11124,#11125,#11126,#11127,
#11128,#11129,#11130,#11131,#11132,#11133,#11134,#11135,#11136,#11137,#11138,
#11139,#11140,#11141,#11142,#11143,#11144,#11145,#11146,#11147,#11148,#11149,
#11150,#11151,#11152,#11153,#11154,#11155,#11156,#11157,#11158,#11159,#11160,
#11161,#11162,#11163,#11164,#11165,#11166,#11167,#11168,#11169,#11170,#11171,
#11172,#11173,#11174,#11175,#11176,#11177,#11178,#11179,#11180,#11181,#11182,
#11183,#11184,#11185,#11186,#11187,#11188,#11189,#11190,#11191,#11192,#11193,
#11194,#11195,#11196,#11197,#11198,#11199,#11200,#11201,#11202,#11203,#11204,
#11205,#11206,#11207,#11208,#11209,#11210,#11211,#11212,#11213,#11214,#11215,
#11216,#11217,#11218,#11219,#11220,#11221,#11222,#11223,#11224,#11225,#11226,
#11227,#11228,#11229,#11230,#11231,#11232,#11233,#11234,#11235,#11236,#11237,
#11238,#11239,#11240,#11241,#11242,#11243,#11244,#11245,#11246,#11247,#11248,
#11249,#11250,#11251,#11252,#11253,#11254,#11255,#11256,#11257,#11258,#11259,
#11260,#11261,#11262,#11263,#11264,#11265,#11266,#11267,#11268,#11269,#11270,
#11271,#11272,#11273,#11274,#11275,#11276,#11277,#11278,#11279,#11280,#11281,
#11282,#11283,#11284,#11285,#11286,#11287,#11288,#11289,#11290,#11291,#11292,
#11293,#11294,#11295,#11296,#11297,#11298,#11299,#11300,#11301,#11302,#11303,
#11304,#11305,#11306,#11307,#11308,#11309,#11310,#11311,#11312,#11313,#11314,
#11315,#11316,#11317,#11318,#11319,#11320,#11321,#11322,#11323,#11324,#11325,
#11326,#11327,#11328,#11329,#11330,#11331,#11332,#11333,#11334,#11335,#11336,
#11337,#11338,#11339,#11340,#11341,#11342,#11343,#11344,#11345,#11346,#11347,
#11348,#11349,#11350,#11351,#11352,#11353,#11354,#11355,#11356,#11357,#11358,
#11359,#11360,#11361,#11362,#11363,#11364,#11365,#11366,#11367,#11368,#11369,
#11370,#11371,#11372,#11373,#11374,#11375,#11376,#11377,#11378,#11379,#11380,
#11381,#11382,#11383,#11384,#11385,#11386,#11387,#11388,#11389,#11390,#11391,
#11392,#11393,#11394,#11395,#11396,#11397,#11398,#11399,#11400,#11401,#11402,
#11403,#11404,#11405,#11406,#11407,#11408,#11409,#11410,#11411,#11412,#11413,
#11414,#11415,#11416,#11417,#11418,#11419,#11420,#11421,#11422,#11423,#11424,
#11425,#11426,#11427,#11428,#11429,#11430,#11431,#11432,#11433,#11434,#11435,
#11436,#11437,#11438,#11439,#11440,#11441,#11442,#11443,#11444,#11445,#11446,
#11447,#11448,#11449,#11450,#11451,#11452,#11453,#11454,#11455,#11456,#11457,
#11458,#11459,#11460,#11461,#11462,#11463,#11464,#11465,#11466,#11467,#11468,
#11469,#11470,#11471,#11472,#11473,#11474,#11475,#11476,#11477,#11478,#11479,
#11480,#11481,#11482,#11483,#11484,#11485,#11486,#11487,#11488,#11489),
 .UNSPECIFIED.,.F.,.F.,(4,2,2,2,2,2,2,2,2,2,2,2,2,2,2,2,2,2,2,2,2,2,2,2,
2,2,2,2,2,2,2,2,2,2,2,2,2,2,2,2,2,2,2,2,2,2,2,2,2,2,2,2,2,2,2,2,2,2,2,2,
2,2,2,2,2,2,2,2,2,2,2,2,2,2,2,2,2,2,2,2,2,2,2,2,2,2,2,2,2,2,2,2,2,2,2,2,
2,2,2,2,2,2,2,2,2,2,2,2,2,2,2,2,2,2,2,2,2,2,2,2,2,2,2,2,2,2,2,2,2,2,2,2,
2,2,2,2,2,2,2,2,2,2,2,2,2,2,2,2,2,2,2,2,2,2,2,2,2,2,2,2,2,2,2,2,2,2,2,2,
2,2,2,2,2,2,2,2,2,2,2,2,2,2,2,2,2,2,2,2,2,2,2,2,2,2,2,2,2,2,2,2,2,2,2,2,
2,2,2,2,2,2,2,2,2,2,2,2,2,2,2,2,2,2,2,2,2,2,2,2,2,2,2,2,2,2,2,2,2,2,2,2,
2,2,2,2,2,2,2,2,2,2,2,2,2,2,2,2,2,2,2,2,2,2,2,2,2,2,2,2,2,2,2,2,2,2,2,2,
2,2,2,2,2,2,2,2,2,2,2,2,2,2,2,2,2,2,2,2,2,2,4),(-2.32112203948973,-2.29034393663197,
-2.28647054352913,-2.28422159465382,-2.28264621329015,-2.28129251248404,
-2.2798401725342,-2.27797922378873,-2.27414412793826,-2.24389445016459,
-2.23036041817568,-2.21877297144587,-2.19059563289267,-2.18397206757087,
-2.18236890586133,-2.1814446293015,-2.18063469572578,-2.17959657842402,
-2.17745231764752,-2.16249553676311,-2.15720436896209,-2.13409044791361,
-2.10492105159793,-2.09324393439829,-2.08578149162186,-2.08336647075221,
-2.08200977518731,-2.08056223814677,-2.07874568768348,-2.07591690870325,
-2.06216288475466,-2.02167619677099,-1.99885813177772,-1.98966470636612,
-1.98435750324089,-1.98287944902174,-1.98198299658212,-1.98116654411944,
-1.98009601980632,-1.97781022307268,-1.9556209163649,-1.91250819660216,
-1.896322988853,-1.89003867888934,-1.88686054005509,-1.88420936482288,-1.88260958474796,
-1.88260750957859,-1.88260542812914,-1.88260334034155,-1.88260124622188,
-1.88259914573118,-1.88259703882885,-1.88259492552241,-1.88259280579806,
-1.88259067960941,-1.8825885469179,-1.88258640773099,-1.8825842620395,-1.88258210978222,
-1.88257995095738,-1.88257778553047,-1.88257561345168,-1.88257343471771,
-1.88257124931054,-1.88256905720309,-1.88256685835465,-1.88256465277214,
-1.88256244040908,-1.88256022124152,-1.88255799524241,-1.88255576240921,
-1.88255352269834,-1.88255127607508,-1.88254902253767,-1.88254676205236,
-1.88254449456044,-1.88254222008303,-1.88253993858481,-1.88253765002649,
-1.88253535437622,-1.88253305162833,-1.88253074174567,-1.88252842470268,
-1.8825261004789,-1.88252376903928,-1.88252143034712,-1.88251908436322,
-1.88251673110272,-1.88251437051583,-1.88251200258282,-1.88105849206935,
-1.87918855363602,-1.8753079328154,-1.84199111305543,-1.79289445508601,
-1.78526898762658,-1.78360264016469,-1.7826643572385,-1.78185621304291,
-1.78083847894255,-1.77886097613549,-1.76734971010007,-1.7421072132408,
-1.71187800519132,-1.69648907289517,-1.68729952727244,-1.68468700078164,
-1.68308575675656,-1.68163242979374,-1.67976308839528,-1.67588502211101,
-1.64275767203379,-1.59111607184786,-1.58552423136097,-1.58401893418032,
-1.58311639154152,-1.5823017367306,-1.58124330229314,-1.57893522530068,
-1.54421524856088,-1.51343883794952,-1.49735558552034,-1.48786705057944,
-1.4852245842756,-1.48361635959058,-1.48216407750241,-1.48030633016285,
-1.47648896168293,-1.44724726348877,-1.40472291912577,-1.39264370799567,
-1.38620522537503,-1.38462601371873,-1.38370677564465,-1.38289522322511,
-1.38184718680793,-1.37965554971408,-1.36331899094411,-1.31299151126481,
-1.29758514579751,-1.28838707638612,-1.2857725086439,-1.28417007496942,
-1.28271570394366,-1.28084506438132,-1.27696444119723,-1.24380312066774,
-1.19210564194618,-1.18657044295578,-1.18507006555024,-1.18416839465968,
-1.18335385406514,-1.18229405005337,-1.18051753815884,-1.16955082681112,
-1.16583493137157,-1.16119078516264,-1.12867971029247,-1.09103808395885,
-1.08713451033408,-1.08526088670644,-1.08380779044098,-1.08221039590717,
-1.0796122544168,-1.07055542696725,-1.0554665161363,-1.02544862332573,-0.988354041188919,
-0.986085814933734,-0.985035302940362,-0.984222042823835,-0.983315609292496,
-0.981793092288234,-0.976014536868777,-0.965662526197371,-0.938251863044715,
-0.891241316006559,-0.887469346613765,-0.88561996084362,-0.884167945054924,
-0.882553556857021,-0.879886048342114,-0.870145871165747,-0.853463515559964,
-0.822174880962791,-0.799484854265853,-0.788392709688315,-0.786607075987028,
-0.785543216418512,-0.784725907054903,-0.783820717399649,-0.782315814134777,
-0.776777517662026,-0.724753861172956,-0.692328027221089,-0.688454517676588,
-0.686582758152494,-0.685125452621556,-0.683517674783842,-0.680889565624703,
-0.671593688673812,-0.655974978735857,-0.625550588075654,-0.589616689867446,
-0.587553822922564,-0.586514065174554,-0.585753705255509,-0.584927288654787,
-0.583758069847875,-0.580851625180863,-0.544798429028698,-0.495932938030075,
-0.48963617077389,-0.487299944797091,-0.485920229628196,-0.484472590203036,
-0.482581777065521,-0.478551708701874,-0.443076827043676,-0.392367432511269,
-0.38822006290789,-0.386851881929456,-0.385988065153033,-0.385186070114668,
-0.384116666053907,-0.381743325347215,-0.378556751791188,-0.343450692637509,
-0.296015116137967,-0.289630282076299,-0.287261995042367,-0.28586407449693,
-0.284397794165779,-0.282483310422913,-0.27840477818196,-0.242398704891009,
-0.216755431214847,-0.190185124254524,-0.187866684088788,-0.186779718505182,
-0.185960650056648,-0.185955646327147,-0.185950774289003,-0.185946029927201,
-0.185941409397797,-0.185936908958964,-0.185932525012532,-0.185928254131056,
-0.185924092969507,-0.185920038301805,-0.185916087018049,-0.185912236117139,
-0.185908482706886,-0.185904823974739,-0.185901257224124,-0.185897779842561,
-0.18589490738148,-0.185892056307941,-0.185889222382127,-0.18588640542643,
-0.185883605320891,-0.185880821922682,-0.185878055068841,-0.18587530461481,
-0.185872570404359,-0.185869852291084,-0.18586715016686,-0.185864463892584,
-0.185861793324586,-0.185859138304044,-0.185856498723685,-0.185853874448655,
-0.185851265330031,-0.185848671268029,-0.185846092112797,-0.185843527743315,
-0.185840978034615,-0.18583844285917,-0.185835922097251,-0.18583341562781,
-0.185830918207774,-0.185828424477525,-0.185825944384559,-0.185823477799486,
-0.184885653291375,-0.1832401140909,-0.176379272645583,-0.16322878190832,
-0.12481775085509,-0.0955331156990872,-0.0916842850318327,-0.0897999504486535,
-0.0883215131433462,-0.0866786520257004,-0.0839658324994265,-0.0740714962628944,
-0.0571530413364035,-0.0033609016908596),.UNSPECIFIED.);
#780=B_SPLINE_CURVE_WITH_KNOTS('',3,(#11493,#11494,#11495,#11496,#11497,
#11498,#11499,#11500,#11501,#11502,#11503,#11504,#11505,#11506,#11507,#11508,
#11509,#11510,#11511,#11512,#11513,#11514,#11515,#11516,#11517,#11518,#11519,
#11520,#11521,#11522,#11523,#11524,#11525,#11526,#11527,#11528,#11529,#11530,
#11531,#11532,#11533,#11534,#11535,#11536,#11537,#11538,#11539,#11540,#11541,
#11542,#11543,#11544,#11545,#11546,#11547,#11548,#11549,#11550,#11551,#11552,
#11553,#11554,#11555,#11556,#11557,#11558,#11559,#11560,#11561,#11562,#11563,
#11564,#11565,#11566,#11567,#11568,#11569,#11570,#11571,#11572,#11573,#11574,
#11575,#11576,#11577,#11578,#11579,#11580,#11581,#11582,#11583,#11584,#11585,
#11586,#11587,#11588,#11589,#11590,#11591,#11592,#11593,#11594,#11595,#11596,
#11597,#11598,#11599,#11600,#11601,#11602,#11603,#11604,#11605,#11606,#11607,
#11608,#11609,#11610,#11611,#11612,#11613,#11614,#11615,#11616),
 .UNSPECIFIED.,.F.,.F.,(4,3,3,3,3,3,3,3,3,3,3,3,3,3,3,3,3,3,3,3,3,3,3,3,
3,3,3,3,3,3,3,3,3,3,3,3,3,3,3,3,3,4),(11.6163931973419,11.7238022892394,
11.8352112612973,11.942542704643,12.0498762579441,12.1572406721673,12.2646647271014,
12.3722554126795,12.4799425122239,12.5878292808977,12.6150740657025,12.7189450740463,
12.8226420757906,12.9261962507554,13.0296728657244,13.1331089565476,13.2365415004203,
13.3400790736674,13.4436725429885,13.5474529273096,13.6137549340633,13.7188586017124,
13.8238046664922,13.9286265972958,14.0333820339704,14.1381063103255,14.2428347153535,
14.3476713207162,14.4525677883591,14.5576434493371,14.612435802424,14.7175655496114,
14.8225415113328,14.9273988904908,15.0321931999677,15.1369597244014,15.241733707136,
15.3466206723545,15.4515702920288,15.5567029266591,15.6111166707848,15.7079632679492),
 .UNSPECIFIED.);
#781=B_SPLINE_CURVE_WITH_KNOTS('',3,(#11618,#11619,#11620,#11621,#11622,
#11623,#11624,#11625,#11626,#11627,#11628,#11629,#11630,#11631,#11632,#11633,
#11634,#11635,#11636,#11637,#11638,#11639,#11640,#11641,#11642,#11643,#11644,
#11645,#11646,#11647,#11648,#11649,#11650,#11651,#11652,#11653,#11654,#11655,
#11656,#11657,#11658,#11659,#11660,#11661,#11662,#11663,#11664,#11665,#11666,
#11667,#11668,#11669,#11670,#11671,#11672,#11673,#11674,#11675,#11676,#11677,
#11678,#11679,#11680,#11681,#11682,#11683,#11684,#11685,#11686,#11687,#11688,
#11689,#11690,#11691,#11692,#11693,#11694,#11695,#11696,#11697,#11698,#11699,
#11700,#11701,#11702,#11703,#11704,#11705,#11706,#11707,#11708,#11709,#11710,
#11711,#11712,#11713,#11714,#11715,#11716,#11717,#11718,#11719,#11720,#11721,
#11722,#11723,#11724,#11725,#11726,#11727,#11728,#11729,#11730,#11731,#11732,
#11733,#11734,#11735,#11736,#11737,#11738,#11739,#11740,#11741,#11742,#11743,
#11744,#11745,#11746,#11747,#11748,#11749,#11750,#11751,#11752,#11753,#11754,
#11755,#11756,#11757,#11758,#11759,#11760,#11761,#11762,#11763,#11764,#11765,
#11766,#11767,#11768,#11769,#11770,#11771,#11772,#11773,#11774,#11775,#11776,
#11777,#11778,#11779,#11780,#11781,#11782,#11783,#11784,#11785,#11786,#11787,
#11788,#11789,#11790,#11791,#11792,#11793,#11794,#11795,#11796,#11797,#11798,
#11799,#11800,#11801,#11802,#11803,#11804,#11805,#11806,#11807),
 .UNSPECIFIED.,.F.,.F.,(4,3,3,3,3,3,3,3,3,3,3,3,3,3,3,3,3,3,3,3,3,3,3,3,
3,3,3,3,3,3,3,3,3,3,3,3,3,3,3,3,3,3,3,3,3,3,3,3,3,3,3,3,3,3,3,3,3,3,3,3,
3,3,3,4),(15.7079632682185,15.811428089593,15.914735438257,16.0179561585831,
16.1211276382724,16.2242871927754,16.3275428620763,16.4308476158766,16.5343372072669,
16.6097975391455,16.7147739380985,16.8195927266471,16.9242880341238,17.0289173338591,
17.1335161631907,17.2381200152761,17.3428343171023,17.4476095828744,17.5525670804081,
17.6084784075063,17.7134461555384,17.818256657873,17.9229442656087,18.0275662339299,
18.1321581124525,18.2367554070047,18.3414637991167,18.4462335142689,18.5511860860768,
18.607159275867,18.712084244627,18.8168511407928,18.9214941268238,19.0260708692261,
19.1306169849403,19.2351680465238,19.3398298056802,19.4445525908897,19.5494582685097,
19.6058401442278,19.7107917719691,19.8155856953168,19.9202561227395,20.0248605477511,
20.1294345458482,20.2340136483747,20.3387034974021,20.4434544424511,20.5483880880719,
20.6045210125885,20.7094692639051,20.8142598285881,20.9189269407677,21.0235280793812,
21.1280988250196,21.2326747141547,21.3373614318861,21.4421092875596,21.547039942974,
21.6032018809493,21.720775965361,21.8379258085655,21.9543756998941,21.9911485747582),
 .UNSPECIFIED.);
#782=B_SPLINE_CURVE_WITH_KNOTS('',3,(#11809,#11810,#11811,#11812,#11813,
#11814,#11815,#11816,#11817,#11818,#11819,#11820,#11821,#11822,#11823,#11824,
#11825,#11826,#11827,#11828,#11829,#11830,#11831,#11832,#11833,#11834,#11835,
#11836,#11837,#11838,#11839,#11840,#11841,#11842,#11843,#11844,#11845,#11846,
#11847,#11848,#11849,#11850,#11851,#11852,#11853,#11854,#11855,#11856,#11857,
#11858,#11859,#11860,#11861,#11862,#11863,#11864,#11865,#11866,#11867,#11868,
#11869,#11870,#11871,#11872,#11873,#11874,#11875,#11876,#11877,#11878,#11879,
#11880,#11881,#11882,#11883,#11884,#11885,#11886,#11887,#11888,#11889,#11890,
#11891,#11892,#11893,#11894,#11895,#11896,#11897,#11898,#11899,#11900,#11901,
#11902,#11903,#11904,#11905,#11906,#11907,#11908,#11909,#11910,#11911,#11912,
#11913,#11914,#11915,#11916,#11917,#11918,#11919,#11920,#11921,#11922,#11923,
#11924,#11925,#11926,#11927,#11928,#11929,#11930,#11931,#11932,#11933,#11934,
#11935,#11936,#11937,#11938,#11939,#11940,#11941,#11942,#11943,#11944,#11945,
#11946,#11947,#11948,#11949,#11950,#11951,#11952,#11953,#11954,#11955,#11956,
#11957,#11958,#11959,#11960,#11961,#11962,#11963,#11964,#11965,#11966,#11967,
#11968,#11969,#11970,#11971,#11972,#11973,#11974,#11975,#11976,#11977,#11978,
#11979,#11980,#11981,#11982,#11983,#11984,#11985,#11986,#11987,#11988,#11989,
#11990,#11991,#11992,#11993,#11994,#11995,#11996,#11997,#11998,#11999,#12000,
#12001,#12002,#12003,#12004,#12005,#12006,#12007,#12008,#12009,#12010,#12011,
#12012,#12013,#12014,#12015,#12016,#12017,#12018,#12019,#12020,#12021,#12022,
#12023,#12024,#12025,#12026,#12027,#12028,#12029,#12030,#12031,#12032,#12033,
#12034,#12035,#12036,#12037,#12038,#12039,#12040,#12041,#12042,#12043,#12044,
#12045,#12046,#12047,#12048,#12049,#12050,#12051,#12052,#12053,#12054,#12055,
#12056,#12057,#12058,#12059,#12060,#12061,#12062,#12063,#12064,#12065,#12066,
#12067,#12068,#12069,#12070,#12071,#12072,#12073,#12074,#12075,#12076,#12077,
#12078,#12079,#12080,#12081,#12082,#12083,#12084,#12085,#12086,#12087,#12088,
#12089,#12090,#12091,#12092,#12093,#12094,#12095,#12096,#12097,#12098,#12099,
#12100,#12101,#12102,#12103,#12104,#12105,#12106,#12107,#12108,#12109,#12110,
#12111,#12112,#12113,#12114,#12115,#12116,#12117,#12118,#12119,#12120,#12121,
#12122,#12123,#12124,#12125,#12126,#12127,#12128,#12129,#12130,#12131,#12132,
#12133,#12134,#12135,#12136,#12137,#12138,#12139,#12140,#12141,#12142,#12143,
#12144,#12145,#12146,#12147,#12148,#12149,#12150,#12151,#12152,#12153,#12154,
#12155,#12156,#12157,#12158,#12159,#12160,#12161,#12162,#12163,#12164,#12165,
#12166,#12167,#12168,#12169,#12170,#12171,#12172,#12173,#12174,#12175,#12176,
#12177,#12178,#12179,#12180,#12181,#12182,#12183,#12184,#12185,#12186,#12187,
#12188,#12189,#12190,#12191,#12192,#12193,#12194,#12195,#12196,#12197,#12198,
#12199,#12200,#12201,#12202,#12203,#12204,#12205,#12206,#12207,#12208,#12209,
#12210,#12211,#12212,#12213,#12214,#12215,#12216,#12217,#12218,#12219,#12220,
#12221,#12222,#12223,#12224,#12225,#12226,#12227,#12228,#12229,#12230,#12231,
#12232,#12233,#12234,#12235,#12236,#12237,#12238,#12239,#12240,#12241,#12242,
#12243,#12244,#12245,#12246,#12247,#12248,#12249,#12250,#12251,#12252,#12253,
#12254,#12255,#12256,#12257,#12258,#12259,#12260,#12261,#12262,#12263,#12264,
#12265,#12266,#12267,#12268,#12269,#12270,#12271,#12272,#12273,#12274,#12275,
#12276,#12277,#12278,#12279,#12280,#12281,#12282,#12283,#12284,#12285,#12286,
#12287,#12288,#12289,#12290,#12291,#12292,#12293,#12294,#12295,#12296,#12297,
#12298,#12299,#12300,#12301,#12302,#12303,#12304,#12305,#12306,#12307,#12308,
#12309,#12310,#12311,#12312,#12313,#12314,#12315,#12316,#12317,#12318,#12319,
#12320,#12321,#12322,#12323,#12324,#12325,#12326,#12327,#12328,#12329,#12330,
#12331,#12332,#12333,#12334,#12335,#12336,#12337,#12338,#12339,#12340,#12341,
#12342,#12343,#12344,#12345,#12346,#12347,#12348,#12349,#12350,#12351,#12352,
#12353,#12354,#12355,#12356,#12357,#12358,#12359,#12360,#12361,#12362,#12363,
#12364,#12365,#12366,#12367,#12368,#12369,#12370,#12371,#12372,#12373,#12374,
#12375,#12376,#12377,#12378,#12379,#12380,#12381,#12382,#12383,#12384,#12385,
#12386,#12387,#12388,#12389,#12390,#12391,#12392,#12393,#12394,#12395,#12396,
#12397,#12398,#12399,#12400,#12401,#12402,#12403,#12404,#12405,#12406,#12407,
#12408,#12409,#12410,#12411,#12412,#12413,#12414,#12415,#12416),
 .UNSPECIFIED.,.F.,.F.,(4,2,2,2,2,2,2,2,2,2,2,2,2,2,2,2,2,2,2,2,2,2,2,2,
2,2,2,2,2,2,2,2,2,2,2,2,2,2,2,2,2,2,2,2,2,2,2,2,2,2,2,2,2,2,2,2,2,2,2,2,
2,2,2,2,2,2,2,2,2,2,2,2,2,2,2,2,2,2,2,2,2,2,2,2,2,2,2,2,2,2,2,2,2,2,2,2,
2,2,2,2,2,2,2,2,2,2,2,2,2,2,2,2,2,2,2,2,2,2,2,2,2,2,2,2,2,2,2,2,2,2,2,2,
2,2,2,2,2,2,2,2,2,2,2,2,2,2,2,2,2,2,2,2,2,2,2,2,2,2,2,2,2,2,2,2,2,2,2,2,
2,2,2,2,2,2,2,2,2,2,2,2,2,2,2,2,2,2,2,2,2,2,2,2,2,2,2,2,2,2,2,2,2,2,2,2,
2,2,2,2,2,2,2,2,2,2,2,2,2,2,2,2,2,2,2,2,2,2,2,2,2,2,2,2,2,2,2,2,2,2,2,2,
2,2,2,2,2,2,2,2,2,2,2,2,2,2,2,2,2,2,2,2,2,2,2,2,2,2,2,2,2,2,2,2,2,2,2,2,
2,2,2,2,2,2,2,2,2,2,2,2,2,2,2,2,2,2,2,2,2,2,2,2,2,2,2,4),(-2.50805337380735,
-2.49230273170689,-2.48969515725638,-2.4879721309386,-2.48659029377073,
-2.48515126546709,-2.48348737884313,-2.48066032034544,-2.47014031804258,
-2.46131255950347,-2.40889689640937,-2.38973858595966,-2.38765995750145,
-2.38663577510663,-2.3859045573641,-2.38511438624379,-2.38371722160485,
-2.37960653916059,-2.37860162748433,-2.3222694492425,-2.30245221453362,
-2.29522363888922,-2.29170703733424,-2.28960480204464,-2.28770806645155,
-2.28627238891754,-2.28490219428901,-2.28264369422874,-2.27689552789189,
-2.22137667587684,-2.1916881195377,-2.18880591033304,-2.18763568819163,
-2.18680623008844,-2.1860455866488,-2.18500117444484,-2.18291596846972,
-2.14876053791525,-2.1178653742566,-2.10159810517336,-2.09529398652869,
-2.09210979879743,-2.08945125019766,-2.08785303254331,-2.08785093934229,
-2.0878488397909,-2.08784673385193,-2.08784462155868,-2.0878425028829,-2.0878403777653,
-2.08783824622176,-2.08783610820019,-2.08783396366588,-2.08783181260181,
-2.08782965498483,-2.08782749082695,-2.08782532007492,-2.08782314271334,
-2.08782095871419,-2.08781876805332,-2.08781657070027,-2.08781436666209,
-2.08781215587453,-2.08780993835682,-2.08780771406652,-2.08780548298024,
-2.08780324506971,-2.08780100030342,-2.08779874865347,-2.08779649013827,
-2.0877942246835,-2.08779195229483,-2.08778967297212,-2.08634066469234,
-2.08449390550047,-2.08072308135107,-2.03402038592985,-2.00653898731637,
-1.9961716280542,-1.9903904965275,-1.98886923505029,-1.98796392091759,-1.98715148560001,
-1.98610210483188,-1.98383736749652,-1.94695335185385,-1.91696677325285,
-1.90185087497643,-1.89278335120487,-1.89018523071595,-1.88858848222102,
-1.8871363836171,-1.88526461484418,-1.88136693562351,-1.84296374730564,
-1.79657849051826,-1.79115166780097,-1.78966324424563,-1.78876520308745,
-1.78795067234804,-1.78688713195961,-1.78509707432152,-1.77383818049552,
-1.74838851190093,-1.71819206758287,-1.70281662861806,-1.69363585299979,
-1.69102610016798,-1.68942661162368,-1.68797491332695,-1.68610771508234,
-1.6822342631551,-1.64915564899741,-1.5975695252565,-1.59198976269645,-1.5904866869202,
-1.58958526941551,-1.5887715230805,-1.58771408496146,-1.58540738824961,
-1.5508353436415,-1.52006751265106,-1.4981887322564,-1.49323177999542,-1.49116794194978,
-1.48968436913414,-1.48833729828806,-1.48654141881142,-1.48216442033558,
-1.44993549698197,-1.39834760789211,-1.39275742684445,-1.39125326555121,
-1.39035154043785,-1.38953774776987,-1.38848056358157,-1.38617565771471,
-1.35145634724781,-1.32073184702012,-1.30469208490277,-1.2952253147138,
-1.29258696752626,-1.29098084839678,-1.2895302075669,-1.28767419944753,
-1.28385912536044,-1.25453762319655,-1.1967637902322,-1.19312165145767,
-1.19179344163707,-1.19101672620502,-1.19019756487045,-1.18908724020945,
-1.18655667564878,-1.15717917947136,-1.1339161099299,-1.09807467424259,
-1.094175968587,-1.09230333233862,-1.09085039390555,-1.08925255355955,-1.08665227837795,
-1.07757348969028,-1.06243290354129,-1.03238989762332,-0.995502802853251,
-0.993236619013654,-0.992186568320054,-0.991373618131902,-0.990467727025134,
-0.988945494002023,-0.983160557136287,-0.97278766769267,-0.945274881694213,
-0.898600441098291,-0.894828999092631,-0.892981442106069,-0.891531580964151,
-0.889920331307093,-0.887259734936026,-0.877563991373871,-0.86098076644573,
-0.82980243985953,-0.808407164941538,-0.805752070845725,-0.795700104316496,
-0.79396993004971,-0.792923752278704,-0.792111359758195,-0.791203402432694,
-0.789671768476562,-0.783780927678264,-0.773138525470895,-0.744491827041945,
-0.741424236279186,-0.699520288687299,-0.695648557225166,-0.693781254131466,
-0.692329057180731,-0.690728596884312,-0.688116304638167,-0.678916926780116,
-0.663498563055043,-0.633233954902853,-0.597017005719636,-0.594963104977835,
-0.593926315465913,-0.5931673840357,-0.592335664456485,-0.591155058594924,
-0.588210865063239,-0.584013178187592,-0.572202787995784,-0.542638995593051,
-0.500258447646521,-0.496391265845604,-0.494524840414645,-0.493072738267317,
-0.491471786913485,-0.488857345596995,-0.479636611977521,-0.464168956172589,
-0.433864913736107,-0.397771946191372,-0.395711701123519,-0.394673302083384,
-0.393913951394184,-0.393100322575271,-0.391957752399258,-0.390661291750234,
-0.388385686170942,-0.370466231470168,-0.332351007882784,-0.300982830065597,
-0.297131949164991,-0.29526870170595,-0.293816971609142,-0.292214297166831,
-0.289592201290835,-0.280294570895473,-0.264648719319465,-0.232866047653858,
-0.198560638514461,-0.196276962117871,-0.195207397497434,-0.194414312381531,
-0.194411525380222,-0.194408761899535,-0.194406018888907,-0.194403296127436,
-0.19440059339051,-0.194397910449151,-0.194395247063212,-0.194392603040179,
-0.194389978160289,-0.194387372207587,-0.194384784989408,-0.194382216307084,
-0.194379665966285,-0.194377133762692,-0.194374619504514,-0.194372122989017,
-0.19436964403352,-0.194367182443886,-0.194364738048061,-0.194362310675196,
-0.194359900137987,-0.194357506291771,-0.19435512892716,-0.194352767874405,
-0.194350422980133,-0.194348094073647,-0.194345780996807,-0.194343483581033,
-0.194341201674791,-0.194338935147501,-0.194336683807319,-0.194334447512859,
-0.194332226142063,-0.194330019516081,-0.194327827484882,-0.194325649918364,
-0.19432348668219,-0.194321331401382,-0.19431917752624,-0.194317037259404,
-0.193412541854142,-0.19245195608457,-0.190997705163816,-0.188322135206659,
-0.163703582311514,-0.130284239582554,-0.127728967988652,-0.116358897600143,
-0.100614438954047,-0.0976565302774177,-0.0957990029368107,-0.0943452047780524,
-0.0927335711596283,-0.0900815323075606,-0.0805162837021464,-0.0642572066088759,
-0.035656491744088,-0.000592665341133465),.UNSPECIFIED.);
#783=B_SPLINE_CURVE_WITH_KNOTS('',3,(#12418,#12419,#12420,#12421,#12422,
#12423,#12424,#12425,#12426,#12427,#12428,#12429,#12430,#12431,#12432,#12433,
#12434,#12435,#12436,#12437,#12438,#12439,#12440,#12441,#12442,#12443,#12444,
#12445,#12446,#12447,#12448,#12449,#12450,#12451,#12452,#12453,#12454,#12455,
#12456,#12457,#12458,#12459,#12460,#12461,#12462,#12463,#12464,#12465,#12466,
#12467,#12468,#12469,#12470,#12471,#12472,#12473,#12474,#12475,#12476,#12477,
#12478,#12479,#12480,#12481,#12482,#12483,#12484,#12485,#12486,#12487,#12488,
#12489,#12490,#12491,#12492,#12493,#12494,#12495,#12496,#12497,#12498,#12499,
#12500,#12501,#12502,#12503,#12504,#12505,#12506,#12507,#12508,#12509,#12510,
#12511,#12512,#12513,#12514,#12515,#12516,#12517,#12518,#12519,#12520,#12521,
#12522,#12523,#12524,#12525,#12526,#12527,#12528,#12529,#12530,#12531,#12532,
#12533,#12534,#12535,#12536,#12537,#12538,#12539,#12540,#12541,#12542,#12543,
#12544,#12545,#12546,#12547,#12548,#12549,#12550,#12551,#12552,#12553,#12554,
#12555,#12556,#12557,#12558,#12559,#12560,#12561,#12562,#12563,#12564,#12565,
#12566,#12567,#12568,#12569,#12570,#12571,#12572,#12573,#12574,#12575,#12576,
#12577,#12578,#12579,#12580,#12581,#12582,#12583,#12584,#12585,#12586,#12587,
#12588,#12589,#12590,#12591,#12592,#12593,#12594,#12595,#12596,#12597,#12598,
#12599,#12600,#12601,#12602,#12603,#12604,#12605,#12606,#12607,#12608,#12609,
#12610,#12611,#12612,#12613,#12614,#12615,#12616,#12617,#12618,#12619,#12620,
#12621,#12622,#12623,#12624,#12625,#12626,#12627,#12628,#12629,#12630,#12631,
#12632,#12633,#12634,#12635,#12636,#12637,#12638,#12639,#12640,#12641,#12642,
#12643,#12644,#12645,#12646,#12647,#12648,#12649,#12650,#12651,#12652,#12653,
#12654,#12655,#12656,#12657,#12658,#12659,#12660,#12661,#12662,#12663,#12664,
#12665,#12666,#12667,#12668,#12669,#12670,#12671,#12672,#12673,#12674,#12675,
#12676,#12677,#12678,#12679,#12680,#12681,#12682,#12683,#12684,#12685,#12686,
#12687,#12688,#12689,#12690,#12691,#12692,#12693,#12694,#12695,#12696,#12697,
#12698,#12699,#12700,#12701,#12702,#12703,#12704,#12705,#12706,#12707,#12708,
#12709,#12710,#12711,#12712,#12713,#12714,#12715,#12716,#12717,#12718,#12719,
#12720,#12721,#12722,#12723,#12724,#12725,#12726,#12727,#12728,#12729,#12730,
#12731,#12732,#12733,#12734,#12735,#12736,#12737,#12738,#12739,#12740,#12741,
#12742,#12743,#12744,#12745,#12746,#12747,#12748,#12749,#12750,#12751,#12752,
#12753,#12754,#12755,#12756,#12757,#12758,#12759,#12760,#12761,#12762,#12763,
#12764,#12765,#12766,#12767,#12768,#12769,#12770,#12771,#12772,#12773,#12774,
#12775,#12776,#12777,#12778,#12779,#12780,#12781,#12782,#12783,#12784,#12785,
#12786,#12787,#12788,#12789,#12790,#12791,#12792,#12793,#12794,#12795,#12796,
#12797,#12798,#12799,#12800,#12801,#12802,#12803,#12804,#12805,#12806,#12807,
#12808,#12809,#12810,#12811,#12812,#12813,#12814,#12815,#12816,#12817,#12818,
#12819,#12820,#12821,#12822,#12823,#12824,#12825,#12826,#12827,#12828,#12829,
#12830,#12831,#12832,#12833,#12834,#12835,#12836,#12837,#12838,#12839,#12840,
#12841,#12842,#12843,#12844,#12845,#12846,#12847,#12848,#12849,#12850,#12851,
#12852,#12853,#12854,#12855,#12856,#12857,#12858,#12859,#12860,#12861,#12862,
#12863,#12864,#12865,#12866,#12867,#12868,#12869,#12870,#12871,#12872,#12873,
#12874,#12875,#12876,#12877,#12878,#12879,#12880,#12881,#12882,#12883,#12884,
#12885,#12886,#12887,#12888,#12889,#12890,#12891,#12892,#12893,#12894,#12895,
#12896,#12897,#12898,#12899,#12900,#12901,#12902,#12903,#12904,#12905,#12906,
#12907,#12908,#12909),.UNSPECIFIED.,.F.,.F.,(4,2,2,2,2,2,2,2,2,2,2,2,2,
2,2,2,2,2,2,2,2,2,2,2,2,2,2,2,2,2,2,2,2,2,2,2,2,2,2,2,2,2,2,2,2,2,2,2,2,
2,2,2,2,2,2,2,2,2,2,2,2,2,2,2,2,2,2,2,2,2,2,2,2,2,2,2,2,2,2,2,2,2,2,2,2,
2,2,2,2,2,2,2,2,2,2,2,2,2,2,2,2,2,2,2,2,2,2,2,2,2,2,2,2,2,2,2,2,2,2,2,2,
2,2,2,2,2,2,2,2,2,2,2,2,2,2,2,2,2,2,2,2,2,2,2,2,2,2,2,2,2,2,2,2,2,2,2,2,
2,2,2,2,2,2,2,2,2,2,2,2,2,2,2,2,2,2,2,2,2,2,2,2,2,2,2,2,2,2,2,2,2,2,2,2,
2,2,2,2,2,2,2,2,2,2,2,2,2,2,2,2,2,2,2,2,2,2,2,2,2,2,2,2,2,2,2,2,2,2,2,2,
2,2,2,2,2,2,2,2,2,2,2,2,2,2,2,2,4),(-2.51449948729211,-2.51245742096797,
-2.51061254852901,-2.50973662496859,-2.50897977983815,-2.50817611630024,
-2.50709184495005,-2.50464863086608,-2.49736079827815,-2.43600423275735,
-2.42198602286685,-2.41630664148812,-2.41202729179934,-2.41007973372854,
-2.408613371016,-2.40723399121773,-2.40494158741794,-2.39900458656281,-2.39759431139554,
-2.39608371647185,-2.33741201082973,-2.3201346327642,-2.31470662092676,
-2.31228686925975,-2.31093234574058,-2.31001298729218,-2.30913822866073,
-2.30834546992963,-2.30728046796092,-2.30494243833302,-2.27214770724904,
-2.2489473218388,-2.2409053178807,-2.22380423309859,-2.21388477089582,-2.21119889511119,
-2.20957950714353,-2.20812690054294,-2.20628210177226,-2.20336656711075,
-2.188303011828,-2.17682904014002,-2.14042730567403,-2.11553578670406,-2.11284518726927,
-2.11138506192809,-2.11042195172882,-2.10951632865074,-2.10872779131837,
-2.1076988358432,-2.10560607879394,-2.09209250198751,-2.04168953094803,
-2.02422138514964,-2.01415081277562,-2.01145108418384,-2.00982864728293,
-2.0083766715546,-2.00653724843925,-2.0029411636405,-1.98014760140986,-1.9623937442954,
-1.93217889705929,-1.91910968361099,-1.91230943946295,-1.91070047704902,
-1.90977394375718,-1.90896273309397,-1.90792389918225,-1.90578131939415,
-1.8909466574496,-1.88653169529326,-1.87007017003166,-1.83949140380663,
-1.82369833128006,-1.81433011517413,-1.81169688981154,-1.81008923901227,
-1.80863419047183,-1.80676833972365,-1.80291801865423,-1.77211249823417,
-1.73153198660517,-1.719117960203,-1.71255380938743,-1.71096315804416,-1.710040646829,
-1.70922871323626,-1.70818333293725,-1.70600772096888,-1.69023348051677,
-1.66959046461123,-1.63926779094241,-1.62380050377503,-1.61457250995358,
-1.61195305120826,-1.61034839914475,-1.60889252872627,-1.60702068407316,
-1.60314019668699,-1.56069512871391,-1.53108282145904,-1.5135959027296,
-1.51154519055792,-1.51052466477915,-1.50979201583859,-1.50899628348168,
-1.5075792224838,-1.50332150287926,-1.46624854650443,-1.4418704551102,-1.42483125028608,
-1.4149372029657,-1.41225354892351,-1.41063457481892,-1.40918174892876,
-1.40733586555799,-1.40441702975491,-1.38930231686929,-1.38794839531444,
-1.33062653857943,-1.3137654998109,-1.31172855433181,-1.31071072927696,
-1.30997832829005,-1.30918115719914,-1.30775731001858,-1.30344929266811,
-1.25785937239113,-1.2171369254388,-1.21323985352464,-1.21136463739186,
-1.20990820256701,-1.20830500822037,-1.20569262227685,-1.19653728443282,
-1.18123583028555,-1.15101685625293,-1.11432620337532,-1.1120473787042,
-1.11099331972636,-1.11017807622191,-1.10927051609357,-1.10774742299906,
-1.10198181890987,-1.09166875381194,-1.0643494610083,-1.01714225872614,
-1.01337196742147,-1.01152177631739,-1.01006838412468,-1.00845169892891,
-1.00577862394998,-0.995998920906617,-0.979232241927195,-0.947863776094077,
-0.924854128346121,-0.914056222225798,-0.912284831191914,-0.911225110715698,
-0.910409112867163,-0.909504661201476,-0.907995351107947,-0.90237923585557,
-0.850674115830689,-0.817525165090444,-0.813640757158348,-0.811768131788582,
-0.810312148537813,-0.808707872523479,-0.806090159442023,-0.796879927679856,
-0.781451411650063,-0.751132685824435,-0.72554856158458,-0.714307045544392,
-0.712514089626195,-0.71144809666393,-0.710631244395518,-0.70973014661502,
-0.708235640511882,-0.702775601862105,-0.655910395233093,-0.617792579854328,
-0.613882657375662,-0.612005119749211,-0.610548593944236,-0.608947025640125,
-0.606341171811046,-0.597247804078683,-0.582087632069768,-0.551985319982088,
-0.514967259461071,-0.512695679389054,-0.511643092190335,-0.510828161925047,
-0.509920045737665,-0.508394035767894,-0.502594301901003,-0.492194384507113,
-0.464603828324921,-0.417833286691694,-0.4140496236272,-0.412196956943016,
-0.410781845014496,-0.409212536105932,-0.40757390901953,-0.405173753278498,
-0.400927596133162,-0.366829982625952,-0.325468660259128,-0.314706051457623,
-0.31293654470393,-0.311877435620106,-0.311061596313918,-0.310156980416095,
-0.308646661181059,-0.30301854278585,-0.251322733646518,-0.218195080654549,
-0.214306874924167,-0.212433626118568,-0.211016648592563,-0.209458885398998,
-0.207835875541873,-0.20547345865871,-0.201321565531384,-0.192246616068802,
-0.164335151817066,-0.118213310571157,-0.113931715412101,-0.112511519595434,
-0.111715177432494,-0.110982729485826,-0.109963633725146,-0.107919864809402,
-0.0907426186945712,-0.0254247461540436,-0.0166005131250681,-0.0137791143661076,
-0.0121133850868176,-0.0106716918028777,-0.00928465068694093,-0.00755312402976869,
-0.00448544524035413,-0.000592059025150225),.UNSPECIFIED.);
#784=B_SPLINE_CURVE_WITH_KNOTS('',3,(#12911,#12912,#12913,#12914,#12915,
#12916,#12917,#12918,#12919,#12920,#12921,#12922,#12923,#12924,#12925,#12926,
#12927,#12928,#12929,#12930,#12931,#12932,#12933,#12934,#12935,#12936,#12937,
#12938,#12939,#12940,#12941,#12942,#12943,#12944,#12945,#12946,#12947,#12948,
#12949,#12950,#12951,#12952,#12953,#12954,#12955,#12956,#12957,#12958,#12959,
#12960,#12961,#12962,#12963,#12964,#12965,#12966,#12967,#12968,#12969,#12970,
#12971,#12972,#12973,#12974,#12975,#12976,#12977,#12978,#12979,#12980,#12981,
#12982,#12983,#12984,#12985,#12986,#12987,#12988,#12989,#12990,#12991,#12992,
#12993,#12994,#12995,#12996,#12997,#12998,#12999,#13000,#13001,#13002,#13003,
#13004,#13005,#13006,#13007,#13008,#13009,#13010,#13011,#13012,#13013,#13014,
#13015,#13016,#13017,#13018,#13019,#13020,#13021,#13022,#13023,#13024,#13025,
#13026,#13027,#13028,#13029,#13030,#13031,#13032,#13033,#13034,#13035,#13036,
#13037,#13038,#13039,#13040,#13041,#13042,#13043,#13044,#13045,#13046,#13047,
#13048,#13049,#13050,#13051,#13052,#13053,#13054,#13055,#13056,#13057,#13058,
#13059,#13060,#13061,#13062,#13063,#13064,#13065,#13066,#13067,#13068,#13069,
#13070,#13071,#13072,#13073,#13074,#13075,#13076,#13077,#13078,#13079,#13080,
#13081,#13082,#13083,#13084,#13085,#13086,#13087,#13088,#13089,#13090,#13091,
#13092,#13093,#13094,#13095,#13096,#13097,#13098,#13099,#13100,#13101,#13102,
#13103,#13104,#13105,#13106,#13107,#13108,#13109,#13110,#13111,#13112,#13113,
#13114,#13115,#13116,#13117,#13118,#13119,#13120,#13121,#13122,#13123,#13124,
#13125,#13126,#13127,#13128,#13129,#13130,#13131,#13132,#13133,#13134,#13135,
#13136,#13137,#13138,#13139,#13140,#13141,#13142,#13143,#13144,#13145,#13146,
#13147,#13148,#13149,#13150,#13151,#13152,#13153,#13154,#13155,#13156,#13157,
#13158,#13159,#13160,#13161,#13162,#13163,#13164,#13165,#13166,#13167,#13168,
#13169,#13170,#13171,#13172,#13173,#13174,#13175,#13176,#13177,#13178,#13179,
#13180,#13181,#13182,#13183,#13184,#13185,#13186,#13187,#13188,#13189,#13190,
#13191,#13192,#13193,#13194,#13195,#13196,#13197,#13198,#13199,#13200,#13201,
#13202,#13203,#13204,#13205,#13206,#13207,#13208,#13209,#13210,#13211,#13212,
#13213,#13214,#13215,#13216,#13217,#13218,#13219,#13220,#13221,#13222,#13223,
#13224,#13225,#13226,#13227,#13228,#13229,#13230,#13231,#13232,#13233,#13234,
#13235,#13236,#13237,#13238,#13239,#13240,#13241,#13242,#13243,#13244,#13245,
#13246,#13247,#13248,#13249,#13250,#13251,#13252,#13253,#13254,#13255,#13256,
#13257,#13258,#13259,#13260,#13261,#13262,#13263,#13264,#13265,#13266,#13267,
#13268,#13269,#13270,#13271,#13272,#13273,#13274,#13275,#13276,#13277,#13278,
#13279,#13280,#13281,#13282,#13283,#13284,#13285,#13286,#13287,#13288,#13289,
#13290,#13291,#13292,#13293,#13294,#13295,#13296,#13297,#13298,#13299,#13300,
#13301,#13302,#13303,#13304,#13305,#13306,#13307,#13308,#13309,#13310,#13311,
#13312,#13313,#13314,#13315,#13316,#13317,#13318,#13319,#13320,#13321,#13322,
#13323,#13324,#13325,#13326,#13327,#13328,#13329,#13330,#13331,#13332,#13333,
#13334,#13335,#13336,#13337,#13338,#13339,#13340,#13341,#13342,#13343,#13344,
#13345,#13346,#13347,#13348,#13349,#13350,#13351,#13352,#13353,#13354,#13355,
#13356,#13357,#13358,#13359,#13360,#13361,#13362,#13363,#13364,#13365,#13366,
#13367,#13368,#13369,#13370,#13371,#13372,#13373,#13374,#13375,#13376,#13377,
#13378,#13379,#13380,#13381,#13382,#13383,#13384,#13385,#13386,#13387,#13388,
#13389,#13390,#13391,#13392,#13393,#13394,#13395,#13396,#13397,#13398,#13399,
#13400,#13401,#13402,#13403,#13404,#13405,#13406,#13407,#13408,#13409,#13410,
#13411,#13412,#13413,#13414,#13415,#13416,#13417,#13418,#13419,#13420,#13421,
#13422,#13423,#13424,#13425,#13426,#13427,#13428,#13429,#13430,#13431,#13432,
#13433,#13434,#13435,#13436,#13437,#13438,#13439,#13440,#13441,#13442,#13443,
#13444,#13445,#13446,#13447,#13448,#13449,#13450,#13451,#13452,#13453,#13454,
#13455,#13456,#13457,#13458,#13459,#13460,#13461,#13462,#13463,#13464,#13465,
#13466,#13467,#13468,#13469,#13470),.UNSPECIFIED.,.F.,.F.,(4,2,2,2,2,2,
2,2,2,2,2,2,2,2,2,2,2,2,2,2,2,2,2,2,2,2,2,2,2,2,2,2,2,2,2,2,2,2,2,2,2,2,
2,2,2,2,2,2,2,2,2,2,2,2,2,2,2,2,2,2,2,2,2,2,2,2,2,2,2,2,2,2,2,2,2,2,2,2,
2,2,2,2,2,2,2,2,2,2,2,2,2,2,2,2,2,2,2,2,2,2,2,2,2,2,2,2,2,2,2,2,2,2,2,2,
2,2,2,2,2,2,2,2,2,2,2,2,2,2,2,2,2,2,2,2,2,2,2,2,2,2,2,2,2,2,2,2,2,2,2,2,
2,2,2,2,2,2,2,2,2,2,2,2,2,2,2,2,2,2,2,2,2,2,2,2,2,2,2,2,2,2,2,2,2,2,2,2,
2,2,2,2,2,2,2,2,2,2,2,2,2,2,2,2,2,2,2,2,2,2,2,2,2,2,2,2,2,2,2,2,2,2,2,2,
2,2,2,2,2,2,2,2,2,2,2,2,2,2,2,2,2,2,2,2,2,2,2,2,2,2,2,2,2,2,2,2,2,2,2,2,
2,2,2,2,2,2,2,2,2,2,2,2,2,2,2,2,2,2,2,2,2,4),(-2.5133074761937,-2.441555832099,
-2.43219700810938,-2.42681902880013,-2.42533266847067,-2.42443353536165,
-2.42361637074292,-2.42254718197082,-2.42018595794761,-2.39121580926245,
-2.34792394817552,-2.33617687934896,-2.3311727316177,-2.32847494043576,
-2.32671218564173,-2.32505389769471,-2.32504508548084,-2.32503600427534,
-2.32502664341511,-2.32501699170266,-2.32500703733442,-2.32499676787873,
-2.3249861702373,-2.32497523060133,-2.32496393437945,-2.32495226617438,
-2.32494020970075,-2.32492774773434,-2.32491486204446,-2.32490153330995,
-2.32488774103758,-2.32487346348351,-2.32485867755953,-2.32484335869554,
-2.32482748076776,-2.32481101594265,-2.32479393454356,-2.32477620491566,
-2.32475896654083,-2.32333589174628,-2.321460035164,-2.31755605394049,-2.27869596130949,
-2.24834868319983,-2.23447723940278,-2.22739641827667,-2.22576694247466,
-2.22483610999621,-2.22402591651849,-2.22299462874836,-2.22095770062709,
-2.20816111595958,-2.18700987266577,-2.17038681340108,-2.13515370387584,
-2.13083729755746,-2.12840938402946,-2.12675951424038,-2.12518127770065,
-2.12517870958474,-2.12517613590436,-2.12517355664914,-2.12517097178146,
-2.12516838128418,-2.12516578513021,-2.12516318329547,-2.12516057573989,
-2.12515796242268,-2.12515534335618,-2.12515271849187,-2.12515008778882,
-2.12514745123588,-2.1251448088156,-2.12514216049822,-2.12513950625008,
-2.12513684606595,-2.12371424003327,-2.12184859059502,-2.11799683870704,
-2.08741769049248,-2.04658044022541,-2.02847933353453,-2.02641649909527,
-2.02539381855083,-2.0246611862245,-2.02386704362522,-2.02245666682299,
-2.01824590338492,-1.97106640892096,-1.93225028719694,-1.92810637194275,
-1.92618446828063,-1.92472236551103,-1.92333580465476,-1.92100471279583,
-1.91482168646161,-1.86403239719211,-1.84401870749798,-1.83362464717951,
-1.82782852516163,-1.82630326547405,-1.82539556127737,-1.82458097320294,
-1.82352880023793,-1.82125799240373,-1.78426364310036,-1.7542030781551,
-1.73905350948089,-1.7299647701368,-1.7273600580679,-1.72575914844842,-1.72430319306596,
-1.7224263505851,-1.71851773239354,-1.68192145721908,-1.64834601727162,
-1.63516495038078,-1.62832568720609,-1.62671412288149,-1.62578720681989,
-1.62497637810595,-1.62393897560121,-1.6218025756197,-1.60712290464845,
-1.60029621715297,-1.56825310490145,-1.53276288128461,-1.52870911967694,
-1.5268042307376,-1.52534447490756,-1.52395216063469,-1.52159195091537,
-1.5152769185501,-1.46739197314248,-1.44466705664436,-1.43427444242065,
-1.42847876548993,-1.42695347049625,-1.42604571575525,-1.42523106202492,
-1.42417877761964,-1.42190762795816,-1.38498712089924,-1.35489793428018,
-1.33971446878164,-1.33061074931315,-1.32800439622865,-1.32640304449159,
-1.32494705989569,-1.3230707040528,-1.3191650099287,-1.28364898803709,-1.25677039865494,
-1.23018470300706,-1.22782787358406,-1.22675957218805,-1.2259426227575,
-1.22504321998997,-1.22355535097764,-1.21816054715107,-1.20876178144355,
-1.18509721528406,-1.13669402191702,-1.13312494064002,-1.12923221778222,
-1.127358446439,-1.12590284564956,-1.12430027831388,-1.12168825787642,-1.11252755743439,
-1.09721068951628,-1.06698895462862,-1.03037327834174,-1.02809531007372,
-1.02704174612925,-1.02622692881707,-1.02531989058121,-1.02379777713794,
-1.01803708377352,-1.0077341395947,-0.980443641753844,-0.933239695903948,
-0.929472018027414,-0.927622934675346,-0.926170332624233,-0.924554443662548,
-0.921882493388162,-0.912104790489056,-0.895339347707471,-0.863981650724361,
-0.840940515189588,-0.830204597071183,-0.828436943297607,-0.827378608380033,
-0.826563162586575,-0.825658762094295,-0.824148324395362,-0.818514387620214,
-0.808528388329783,-0.78239582334916,-0.737475832326166,-0.733044440688509,
-0.729953077599993,-0.728075807321763,-0.726615502143086,-0.725030305574051,
-0.722496127661981,-0.714079186548939,-0.700433685809388,-0.643888818912175,
-0.630666927842235,-0.62858656435679,-0.627560284633167,-0.626750416700883,
-0.625815883886836,-0.624170057721989,-0.616864155793498,-0.602337381510688,
-0.554123147982252,-0.551429760952961,-0.547762815398685,-0.532944965303936,
-0.530045318924305,-0.528205702807971,-0.526754093300621,-0.525132606144415,
-0.522435727593154,-0.51239039311322,-0.494978813004558,-0.445074893535946,
-0.442579302647778,-0.430843063091563,-0.428851742265716,-0.42783011462256,
-0.4270205994022,-0.426101552224707,-0.424502668789999,-0.422533668695574,
-0.418452908497334,-0.407126561129945,-0.364998365998589,-0.334249169226604,
-0.330400864980992,-0.328535712729009,-0.3270810829575,-0.325473766543612,
-0.322840797388725,-0.313470518026063,-0.297668595149222,-0.243952725511428,
-0.231176502133581,-0.22913996781967,-0.228108593270446,-0.227298187809366,
-0.226535598454271,-0.225123886017466,-0.220432093983249,-0.212635786302988,
-0.186615885237806,-0.138120559031465,-0.134904660180586,-0.130784213489283,
-0.128887130089909,-0.127423562048058,-0.12584687539658,-0.123352090594298,
-0.115292947584701,-0.102424886580751,-0.0586127148397013,-0.0515117662900704,
-0.04696108305432,-0.0316015194634914,-0.0294403804906191,-0.0283979769820426,
-0.0275865104888005,-0.026825222637773,-0.0259135837775704,-0.0245776869027071,
-0.0192352251262995,-0.000591822641302136),.UNSPECIFIED.);
#785=B_SPLINE_CURVE_WITH_KNOTS('',3,(#13472,#13473,#13474,#13475,#13476,
#13477,#13478,#13479,#13480,#13481,#13482,#13483,#13484,#13485,#13486,#13487,
#13488,#13489,#13490,#13491,#13492,#13493,#13494,#13495,#13496,#13497,#13498,
#13499,#13500,#13501,#13502,#13503,#13504,#13505,#13506,#13507,#13508,#13509,
#13510,#13511,#13512,#13513,#13514,#13515,#13516,#13517,#13518,#13519,#13520,
#13521,#13522,#13523,#13524,#13525,#13526,#13527,#13528,#13529,#13530,#13531,
#13532,#13533,#13534,#13535,#13536,#13537,#13538,#13539,#13540,#13541,#13542,
#13543,#13544,#13545,#13546,#13547,#13548,#13549,#13550,#13551,#13552,#13553,
#13554,#13555,#13556,#13557,#13558,#13559,#13560,#13561,#13562,#13563,#13564,
#13565,#13566,#13567,#13568,#13569,#13570,#13571,#13572,#13573,#13574,#13575,
#13576,#13577,#13578,#13579,#13580,#13581,#13582,#13583,#13584,#13585,#13586,
#13587,#13588,#13589,#13590,#13591,#13592,#13593,#13594,#13595,#13596,#13597,
#13598,#13599,#13600,#13601,#13602,#13603,#13604,#13605,#13606,#13607,#13608,
#13609,#13610,#13611,#13612,#13613,#13614,#13615,#13616,#13617,#13618,#13619,
#13620,#13621,#13622,#13623,#13624,#13625,#13626,#13627,#13628,#13629,#13630,
#13631,#13632,#13633,#13634,#13635,#13636,#13637,#13638,#13639,#13640,#13641,
#13642,#13643,#13644,#13645,#13646,#13647,#13648,#13649,#13650,#13651,#13652,
#13653,#13654,#13655,#13656,#13657,#13658,#13659,#13660,#13661),
 .UNSPECIFIED.,.F.,.F.,(4,3,3,3,3,3,3,3,3,3,3,3,3,3,3,3,3,3,3,3,3,3,3,3,
3,3,3,3,3,3,3,3,3,3,3,3,3,3,3,3,3,3,3,3,3,3,3,3,3,3,3,3,3,3,3,3,3,3,3,3,
3,3,3,4),(59.6902604186975,59.7979473347376,59.9011330896705,60.0042464287171,
60.1073248025605,60.2104056071731,60.31359111605,60.4168388149509,60.5202570165798,
60.5517557470186,60.6567015618828,60.7614896268816,60.8661541575229,60.9707526653145,
61.0753207347265,61.1798939060593,61.2845778611266,61.3893229245271,61.4942507709874,
61.5504366153793,61.6553824302435,61.7601704952422,61.8648350258835,61.9694335336753,
62.0740016030872,62.1785747744198,62.283258729487,62.3880037928878,62.4929316393481,
62.5491174837401,62.6540632986043,62.7588513636033,62.8635158942446,62.9681144020364,
63.0726824714484,63.1772556427811,63.2819395978483,63.3866846612489,63.4916125077092,
63.5477983521008,63.6527441669649,63.7575322319637,63.862196762605,63.9667952703968,
64.0713633398087,64.1759365111414,64.2806204662085,64.3853655296093,64.4902933760696,
64.5464792204616,64.6514250353258,64.7562131003246,64.8608776309659,64.9654761387577,
65.0700442081696,65.1746173795019,65.2793013345691,65.3840463979698,65.4889742444302,
65.5451600888223,65.6595690390446,65.7736658819306,65.8872569368679,65.9734457253859),
 .UNSPECIFIED.);
#786=B_SPLINE_CURVE_WITH_KNOTS('',3,(#13663,#13664,#13665,#13666,#13667,
#13668,#13669,#13670,#13671,#13672),.UNSPECIFIED.,.F.,.F.,(4,1,1,1,1,1,
1,4),(65.9734457253859,66.5438409571831,67.5425218255438,68.5412026939046,
69.5398835622653,70.5385644306261,71.5372452989868,72.2566310325655),
 .UNSPECIFIED.);
#787=B_SPLINE_CURVE_WITH_KNOTS('',3,(#13674,#13675,#13676,#13677,#13678,
#13679,#13680,#13681,#13682,#13683,#13684,#13685,#13686,#13687,#13688,#13689,
#13690,#13691,#13692,#13693,#13694,#13695,#13696,#13697,#13698,#13699,#13700,
#13701,#13702,#13703,#13704,#13705,#13706,#13707,#13708,#13709,#13710,#13711,
#13712,#13713,#13714,#13715,#13716,#13717,#13718,#13719,#13720,#13721,#13722,
#13723,#13724,#13725,#13726,#13727,#13728,#13729,#13730,#13731,#13732,#13733,
#13734,#13735,#13736,#13737,#13738,#13739,#13740,#13741,#13742,#13743,#13744,
#13745,#13746,#13747,#13748,#13749,#13750,#13751,#13752,#13753,#13754,#13755,
#13756,#13757,#13758,#13759,#13760,#13761,#13762,#13763,#13764,#13765,#13766,
#13767,#13768,#13769,#13770,#13771,#13772,#13773,#13774,#13775,#13776,#13777,
#13778,#13779,#13780,#13781,#13782,#13783,#13784,#13785,#13786,#13787,#13788,
#13789,#13790,#13791,#13792,#13793,#13794,#13795,#13796,#13797,#13798,#13799,
#13800,#13801,#13802,#13803,#13804,#13805,#13806,#13807,#13808,#13809,#13810,
#13811,#13812,#13813,#13814,#13815,#13816,#13817,#13818,#13819,#13820,#13821,
#13822,#13823,#13824,#13825,#13826,#13827,#13828,#13829,#13830,#13831,#13832,
#13833,#13834,#13835,#13836,#13837,#13838,#13839,#13840,#13841,#13842,#13843,
#13844,#13845,#13846,#13847,#13848,#13849,#13850,#13851,#13852,#13853,#13854,
#13855,#13856,#13857,#13858,#13859,#13860,#13861,#13862,#13863,#13864,#13865,
#13866,#13867,#13868,#13869,#13870,#13871,#13872,#13873,#13874,#13875,#13876,
#13877,#13878,#13879,#13880,#13881,#13882,#13883,#13884,#13885,#13886,#13887,
#13888,#13889,#13890,#13891,#13892,#13893,#13894,#13895,#13896,#13897,#13898,
#13899,#13900,#13901,#13902,#13903,#13904,#13905,#13906,#13907,#13908,#13909,
#13910,#13911,#13912,#13913,#13914,#13915,#13916,#13917,#13918,#13919,#13920,
#13921,#13922,#13923,#13924,#13925,#13926,#13927,#13928,#13929,#13930,#13931,
#13932,#13933,#13934,#13935,#13936,#13937,#13938,#13939,#13940,#13941,#13942,
#13943,#13944,#13945,#13946,#13947,#13948,#13949,#13950,#13951,#13952,#13953,
#13954,#13955,#13956,#13957,#13958,#13959,#13960,#13961,#13962,#13963,#13964,
#13965,#13966,#13967,#13968,#13969,#13970,#13971,#13972,#13973,#13974,#13975,
#13976,#13977,#13978,#13979,#13980,#13981,#13982,#13983,#13984,#13985,#13986,
#13987,#13988,#13989,#13990,#13991,#13992,#13993,#13994,#13995,#13996,#13997,
#13998,#13999,#14000,#14001,#14002,#14003,#14004,#14005,#14006,#14007,#14008,
#14009,#14010,#14011,#14012,#14013,#14014,#14015,#14016,#14017,#14018,#14019,
#14020,#14021,#14022,#14023,#14024,#14025,#14026,#14027,#14028,#14029,#14030,
#14031,#14032,#14033,#14034,#14035,#14036,#14037,#14038,#14039,#14040,#14041,
#14042,#14043,#14044,#14045,#14046,#14047,#14048,#14049,#14050,#14051,#14052,
#14053,#14054,#14055,#14056,#14057,#14058,#14059,#14060,#14061,#14062,#14063,
#14064,#14065,#14066,#14067,#14068,#14069,#14070,#14071,#14072,#14073,#14074,
#14075,#14076,#14077,#14078,#14079,#14080,#14081,#14082,#14083,#14084,#14085,
#14086,#14087,#14088,#14089,#14090,#14091,#14092,#14093,#14094,#14095,#14096,
#14097,#14098,#14099,#14100,#14101,#14102,#14103,#14104,#14105,#14106,#14107,
#14108,#14109,#14110,#14111,#14112,#14113,#14114,#14115,#14116,#14117,#14118,
#14119,#14120,#14121,#14122,#14123,#14124,#14125,#14126,#14127,#14128,#14129,
#14130,#14131,#14132,#14133,#14134,#14135,#14136,#14137,#14138,#14139,#14140,
#14141,#14142,#14143,#14144,#14145,#14146,#14147,#14148,#14149,#14150,#14151,
#14152,#14153,#14154,#14155,#14156,#14157,#14158,#14159,#14160,#14161,#14162,
#14163,#14164,#14165,#14166,#14167,#14168,#14169,#14170,#14171,#14172,#14173),
 .UNSPECIFIED.,.F.,.F.,(4,2,2,2,2,2,2,2,2,2,2,2,2,2,2,2,2,2,2,2,2,2,2,2,
2,2,2,2,2,2,2,2,2,2,2,2,2,2,2,2,2,2,2,2,2,2,2,2,2,2,2,2,2,2,2,2,2,2,2,2,
2,2,2,2,2,2,2,2,2,2,2,2,2,2,2,2,2,2,2,2,2,2,2,2,2,2,2,2,2,2,2,2,2,2,2,2,
2,2,2,2,2,2,2,2,2,2,2,2,2,2,2,2,2,2,2,2,2,2,2,2,2,2,2,2,2,2,2,2,2,2,2,2,
2,2,2,2,2,2,2,2,2,2,2,2,2,2,2,2,2,2,2,2,2,2,2,2,2,2,2,2,2,2,2,2,2,2,2,2,
2,2,2,2,2,2,2,2,2,2,2,2,2,2,2,2,2,2,2,2,2,2,2,2,2,2,2,2,2,2,2,2,2,2,2,2,
2,2,2,2,2,2,2,2,2,2,2,2,2,2,2,2,2,2,2,2,2,2,2,2,2,2,2,2,2,2,2,2,2,2,2,2,
2,2,2,2,2,2,2,2,2,4),(-2.51331156719081,-2.46641556758931,-2.46237904032085,
-2.46042563756789,-2.45881987310794,-2.45789427341653,-2.45708329463419,
-2.45604398670242,-2.45389777857934,-2.43894518859822,-2.43352847324749,
-2.40708343247289,-2.38941412313501,-2.36694790405523,-2.36151719932127,
-2.3598606942312,-2.3582531174483,-2.35679876334723,-2.35493467563917,-2.35109111486464,
-2.32060805612252,-2.27621475136901,-2.26622847779929,-2.26061502890027,
-2.259093966513,-2.25818716021471,-2.25737227547749,-2.2563182702099,-2.25456545830247,
-2.24412581558946,-2.22170834771183,-2.18266364631991,-2.1703023514551,
-2.16511165265753,-2.16117080919431,-2.15928890521519,-2.15782689483504,
-2.15643955241997,-2.15410504959083,-2.1479043734363,-2.0973997782872,-2.07514456769658,
-2.06171459215125,-2.05973469102586,-2.05872883105891,-2.05792039886308,
-2.05697057770122,-2.05530112896679,-2.04852835706711,-1.98860779668247,
-1.97253934036405,-1.96305446153229,-1.96041051487245,-1.95880087305802,
-1.95734697669968,-1.95548670100387,-1.95166249094168,-1.90665504440521,
-1.88103280253598,-1.86807569803831,-1.86131617571103,-1.85971069830028,
-1.85878512771997,-1.8579740864549,-1.8569345825541,-1.85478757081168,-1.83981538124798,
-1.83423455787463,-1.79045309802062,-1.77336333953354,-1.76344968537372,
-1.76076504418596,-1.75914633356407,-1.75769429182097,-1.75585015212371,
-1.75210725958851,-1.74816788493183,-1.70361448423478,-1.67718542300212,
-1.66712468931043,-1.66146121594546,-1.6599479994821,-1.65904295524339,
-1.65822763355114,-1.65717039836451,-1.65540657665882,-1.64474824866497,
-1.64145682681466,-1.63635839707221,-1.61395774454113,-1.59706509127848,
-1.566707906706,-1.5622468266814,-1.56026627455423,-1.55879476935091,-1.55742473853623,
-1.55518060537167,-1.54953867289628,-1.48717258645446,-1.47016765452698,
-1.46206009734913,-1.46036069633657,-1.45941433883957,-1.4586055462611,
-1.45759504801634,-1.45602339207198,-1.44858983195532,-1.38694716935676,
-1.37249569056866,-1.36371452712017,-1.36114128062148,-1.35954726872352,
-1.35808930585529,-1.35622942257207,-1.35230491859648,-1.34864462726753,
-1.30464428965609,-1.26674506242754,-1.26344460977994,-1.26100486489638,
-1.25990954822187,-1.25909129735208,-1.25830725721525,-1.25694784501452,
-1.2527386236874,-1.22546839577746,-1.20378342813574,-1.16630248360066,
-1.16239257677004,-1.16051530777154,-1.15905910603019,-1.15745801060603,
-1.15485318803356,-1.14576604436613,-1.13061877894284,-1.10053114181583,
-1.06350040417531,-1.06122923517285,-1.06017687411129,-1.05936213459069,
-1.0584542481412,-1.05692866193142,-1.05113097885456,-1.04073523124816,
-1.01316179138208,-0.966384573395418,-0.962604821082921,-0.960753193482881,
-0.959300138148154,-0.957685338947238,-0.955018881811901,-0.94530178524887,
-0.928682041508377,-0.897435031373139,-0.875992205806229,-0.873337140315538,
-0.863258113587079,-0.861523868269612,-0.860475308793578,-0.859661116116092,
-0.858751201284992,-0.857216385170257,-0.851314738889617,-0.840654444771424,
-0.811961187897934,-0.810530397832079,-0.76681330059254,-0.762963629376737,
-0.761098224977234,-0.759643582918983,-0.75803644063079,-0.755404184086842,
-0.746040895799794,-0.730255183249775,-0.699660104992737,-0.664157430385115,
-0.661857069063419,-0.660799254031398,-0.65998380233488,-0.659078952266976,
-0.657566803858033,-0.651915658727571,-0.641887329398766,-0.615587649109692,
-0.570886879362118,-0.566401999564037,-0.56333936565416,-0.561470504887896,
-0.560011284694438,-0.558421756403332,-0.555868620949217,-0.547277624767821,
-0.533248568793334,-0.475369572012022,-0.463930956043464,-0.461954964218194,
-0.460936588064829,-0.460127248860624,-0.459186826604164,-0.457514570786302,
-0.449826126491585,-0.400411181547559,-0.367378126123984,-0.363496445871771,
-0.361624667035728,-0.360169133106218,-0.360166511435948,-0.360163895769302,
-0.360161286085973,-0.360158682405084,-0.360156084702595,-0.360153492950245,
-0.360150907113693,-0.360148327164743,-0.360145753099508,-0.358566835811915,
-0.356035654034639,-0.353017304955375,-0.347168365265727,-0.33255593713871,
-0.296581038777048,-0.276043764867396,-0.264233067965491,-0.262237716374046,
-0.261215184427658,-0.260405553475419,-0.259468210527326,-0.257809873516144,
-0.250326147616493,-0.23526871741068,-0.191584259048881,-0.182915678781613,
-0.166765508304984,-0.16378394871383,-0.161919233093932,-0.160464576525571,
-0.159108843420455,-0.157531528050288,-0.152933698999367,-0.132262473361209,
-0.11452803702179,-0.0677013431936985,-0.0634452588229367,-0.0620286008629612,
-0.061233060217987,-0.0605005625719637,-0.0594802164029013,-0.0574297403832107,
-0.0399344391945697,-0.000592787767141576),.UNSPECIFIED.);
#788=B_SPLINE_CURVE_WITH_KNOTS('',3,(#14175,#14176,#14177,#14178,#14179,
#14180,#14181,#14182,#14183,#14184,#14185,#14186,#14187,#14188,#14189,#14190,
#14191,#14192,#14193,#14194,#14195,#14196,#14197,#14198,#14199,#14200,#14201,
#14202,#14203,#14204,#14205,#14206,#14207,#14208,#14209,#14210,#14211,#14212,
#14213,#14214,#14215,#14216,#14217,#14218,#14219,#14220,#14221,#14222,#14223,
#14224,#14225,#14226,#14227,#14228,#14229,#14230,#14231,#14232,#14233,#14234,
#14235,#14236,#14237,#14238,#14239,#14240,#14241,#14242,#14243,#14244,#14245,
#14246,#14247,#14248,#14249,#14250,#14251,#14252,#14253,#14254,#14255,#14256,
#14257,#14258,#14259,#14260,#14261,#14262,#14263,#14264,#14265,#14266,#14267,
#14268,#14269,#14270,#14271,#14272,#14273,#14274,#14275,#14276,#14277,#14278,
#14279,#14280,#14281,#14282,#14283,#14284,#14285,#14286,#14287,#14288,#14289,
#14290,#14291,#14292,#14293,#14294,#14295,#14296,#14297,#14298,#14299,#14300,
#14301,#14302,#14303,#14304,#14305,#14306,#14307,#14308,#14309,#14310,#14311,
#14312,#14313,#14314,#14315,#14316,#14317,#14318,#14319,#14320,#14321,#14322,
#14323,#14324,#14325,#14326,#14327,#14328,#14329,#14330,#14331,#14332,#14333,
#14334,#14335,#14336,#14337,#14338,#14339,#14340,#14341,#14342,#14343,#14344,
#14345,#14346,#14347,#14348,#14349,#14350,#14351,#14352,#14353,#14354,#14355,
#14356,#14357,#14358,#14359,#14360,#14361,#14362,#14363,#14364),
 .UNSPECIFIED.,.F.,.F.,(4,3,3,3,3,3,3,3,3,3,3,3,3,3,3,3,3,3,3,3,3,3,3,3,
3,3,3,3,3,3,3,3,3,3,3,3,3,3,3,3,3,3,3,3,3,3,3,3,3,3,3,3,3,3,3,3,3,3,3,3,
3,3,3,4),(84.8230016469247,84.9270370546266,85.0310354285839,85.135033069763,
85.2391393980532,85.3433028849637,85.4476570100154,85.5187774560374,85.6237232709015,
85.7285113359001,85.8331758665414,85.9377743743331,86.0423424437451,86.1469156150778,
86.251599570145,86.3563446335458,86.4612724800061,86.5174583243981,86.6224041392623,
86.7271922042609,86.8318567349023,86.936455242694,87.0410233121059,87.1455964834384,
87.2502804385056,87.3550255019063,87.4599533483666,87.5161391927589,87.6210850076231,
87.725873072622,87.8305376032632,87.9351361110549,88.0397041804669,88.1442773517997,
88.2489613068668,88.3537063702675,88.4586342167277,88.5148200611196,88.6197658759839,
88.7245539409826,88.8292184716239,88.9338169794156,89.0383850488277,89.1429582201606,
89.2476421752278,89.3523872386285,89.4573150850887,89.5135009294804,89.6184467443445,
89.7232348093431,89.8278993399843,89.9324978477761,90.037065917188,90.1416390885208,
90.246323043588,90.3510681069884,90.4559959534485,90.5121817978411,90.6188240101089,
90.7252911795686,90.831589163945,90.9377877569733,91.0439192365143,91.1061869541043),
 .UNSPECIFIED.);
#789=B_SPLINE_CURVE_WITH_KNOTS('',3,(#14366,#14367,#14368,#14369,#14370,
#14371,#14372,#14373,#14374,#14375),.UNSPECIFIED.,.F.,.F.,(4,1,1,1,1,1,
1,4),(91.1061934734467,91.5108626662019,92.5095435345626,93.5082244029234,
94.5069052712841,95.5055861396449,96.5042670080056,97.3893634456),
 .UNSPECIFIED.);
#790=B_SPLINE_CURVE_WITH_KNOTS('',3,(#14377,#14378,#14379,#14380,#14381,
#14382,#14383,#14384,#14385,#14386,#14387,#14388,#14389,#14390,#14391,#14392,
#14393,#14394,#14395,#14396,#14397,#14398,#14399,#14400,#14401,#14402,#14403,
#14404,#14405,#14406,#14407,#14408,#14409,#14410,#14411,#14412,#14413,#14414,
#14415,#14416,#14417,#14418,#14419,#14420,#14421,#14422,#14423,#14424,#14425,
#14426,#14427,#14428,#14429,#14430,#14431,#14432,#14433,#14434,#14435,#14436,
#14437,#14438,#14439,#14440,#14441,#14442,#14443,#14444,#14445,#14446,#14447,
#14448,#14449,#14450,#14451,#14452,#14453,#14454,#14455,#14456,#14457,#14458,
#14459,#14460,#14461,#14462,#14463,#14464,#14465,#14466,#14467,#14468,#14469,
#14470,#14471,#14472,#14473,#14474,#14475,#14476,#14477,#14478,#14479,#14480,
#14481,#14482,#14483,#14484,#14485,#14486,#14487,#14488,#14489,#14490,#14491,
#14492,#14493,#14494,#14495,#14496,#14497,#14498,#14499,#14500,#14501,#14502,
#14503,#14504,#14505,#14506,#14507,#14508,#14509,#14510,#14511,#14512,#14513,
#14514,#14515,#14516,#14517,#14518,#14519,#14520,#14521,#14522,#14523,#14524,
#14525,#14526,#14527,#14528,#14529,#14530,#14531,#14532,#14533,#14534,#14535,
#14536,#14537,#14538,#14539,#14540,#14541,#14542,#14543,#14544,#14545,#14546,
#14547,#14548,#14549,#14550,#14551,#14552,#14553,#14554,#14555,#14556,#14557,
#14558,#14559,#14560,#14561,#14562,#14563,#14564,#14565,#14566),
 .UNSPECIFIED.,.F.,.F.,(4,3,3,3,3,3,3,3,3,3,3,3,3,3,3,3,3,3,3,3,3,3,3,3,
3,3,3,3,3,3,3,3,3,3,3,3,3,3,3,3,3,3,3,3,3,3,3,3,3,3,3,3,3,3,3,3,3,3,3,3,
3,3,3,4),(97.3893722612839,97.5029478763664,97.6078936912306,97.7126817562294,
97.8173462868706,97.9219447946623,98.0265128640743,98.131086035407,98.2357699904742,
98.3405150538749,98.4454429003351,98.5016287447271,98.6065745595913,98.7113626245902,
98.8160271552315,98.9206256630233,99.0251937324353,99.129766903768,99.2344508588353,
99.339195922236,99.4441237686963,99.5003096130879,99.6052554279521,99.7100434929509,
99.8147080235921,99.9193065313838,100.023874600796,100.128447772128,100.233131727196,
100.337876790596,100.442804637057,100.498990481449,100.603936296313,100.708724361312,
100.813388891953,100.917987399745,101.022555469157,101.127128640489,101.231812595557,
101.336557658957,101.441485505417,101.497671349809,101.602617164673,101.707405229672,
101.812069760313,101.916668268105,102.021236337517,102.12580950885,102.230493463917,
102.335238527318,102.440166373778,102.49635221817,102.601298033034,102.706086098033,
102.810750628674,102.915349136466,103.019917205878,103.124490377211,103.229174332278,
103.333919395679,103.438847242139,103.495033086531,103.655360446659,103.672557568463),
 .UNSPECIFIED.);
#791=B_SPLINE_CURVE_WITH_KNOTS('',3,(#14568,#14569,#14570,#14571,#14572,
#14573,#14574,#14575,#14576,#14577,#14578,#14579,#14580,#14581,#14582,#14583,
#14584,#14585,#14586,#14587,#14588,#14589,#14590,#14591,#14592,#14593,#14594,
#14595,#14596,#14597,#14598,#14599,#14600,#14601,#14602,#14603,#14604,#14605,
#14606,#14607,#14608,#14609,#14610,#14611,#14612,#14613,#14614,#14615,#14616,
#14617,#14618,#14619,#14620,#14621,#14622,#14623,#14624,#14625,#14626,#14627,
#14628,#14629,#14630,#14631,#14632,#14633,#14634,#14635,#14636,#14637,#14638,
#14639,#14640,#14641,#14642,#14643,#14644,#14645,#14646,#14647,#14648,#14649,
#14650,#14651,#14652,#14653,#14654,#14655,#14656,#14657,#14658,#14659,#14660,
#14661,#14662,#14663,#14664,#14665,#14666,#14667,#14668,#14669,#14670,#14671,
#14672,#14673,#14674,#14675,#14676,#14677,#14678,#14679,#14680,#14681,#14682,
#14683,#14684,#14685,#14686,#14687,#14688,#14689,#14690,#14691,#14692,#14693,
#14694,#14695,#14696,#14697,#14698,#14699,#14700,#14701,#14702,#14703,#14704,
#14705,#14706,#14707,#14708,#14709,#14710,#14711,#14712,#14713,#14714,#14715,
#14716,#14717,#14718,#14719,#14720,#14721,#14722,#14723,#14724,#14725,#14726,
#14727,#14728,#14729,#14730,#14731,#14732,#14733,#14734,#14735,#14736,#14737,
#14738,#14739,#14740,#14741,#14742,#14743,#14744,#14745,#14746,#14747,#14748,
#14749,#14750,#14751,#14752,#14753,#14754,#14755,#14756,#14757,#14758,#14759,
#14760,#14761,#14762,#14763,#14764,#14765,#14766,#14767,#14768,#14769,#14770,
#14771,#14772,#14773,#14774,#14775,#14776,#14777,#14778,#14779,#14780,#14781,
#14782,#14783,#14784,#14785,#14786,#14787,#14788,#14789,#14790,#14791,#14792,
#14793,#14794,#14795,#14796,#14797,#14798,#14799,#14800,#14801,#14802,#14803,
#14804,#14805,#14806,#14807,#14808,#14809,#14810,#14811,#14812,#14813,#14814,
#14815,#14816,#14817,#14818,#14819,#14820,#14821,#14822,#14823,#14824,#14825,
#14826,#14827,#14828,#14829,#14830,#14831,#14832,#14833,#14834,#14835,#14836,
#14837,#14838,#14839,#14840,#14841,#14842,#14843,#14844,#14845,#14846,#14847,
#14848,#14849,#14850,#14851,#14852,#14853,#14854,#14855,#14856,#14857,#14858,
#14859,#14860,#14861,#14862,#14863,#14864,#14865,#14866,#14867,#14868,#14869,
#14870,#14871,#14872,#14873,#14874,#14875,#14876,#14877,#14878,#14879,#14880,
#14881,#14882,#14883,#14884,#14885,#14886,#14887,#14888,#14889,#14890,#14891,
#14892,#14893,#14894,#14895,#14896,#14897,#14898,#14899,#14900,#14901,#14902,
#14903,#14904,#14905,#14906,#14907,#14908,#14909,#14910,#14911,#14912,#14913,
#14914,#14915,#14916,#14917,#14918,#14919,#14920,#14921,#14922,#14923,#14924,
#14925,#14926,#14927,#14928,#14929,#14930,#14931,#14932,#14933,#14934,#14935,
#14936,#14937,#14938,#14939,#14940,#14941,#14942,#14943,#14944,#14945,#14946,
#14947,#14948,#14949,#14950,#14951,#14952,#14953,#14954,#14955,#14956,#14957,
#14958,#14959,#14960,#14961,#14962,#14963,#14964,#14965,#14966,#14967,#14968,
#14969,#14970,#14971,#14972,#14973,#14974,#14975,#14976,#14977,#14978,#14979,
#14980,#14981,#14982,#14983,#14984,#14985,#14986,#14987,#14988,#14989,#14990,
#14991,#14992,#14993,#14994,#14995,#14996,#14997,#14998,#14999,#15000,#15001,
#15002,#15003,#15004,#15005,#15006,#15007,#15008,#15009,#15010,#15011,#15012,
#15013,#15014,#15015,#15016,#15017,#15018,#15019,#15020,#15021,#15022,#15023,
#15024,#15025,#15026,#15027,#15028,#15029,#15030,#15031,#15032,#15033,#15034,
#15035,#15036,#15037,#15038,#15039),.UNSPECIFIED.,.F.,.F.,(4,2,2,2,2,2,
2,2,2,2,2,2,2,2,2,2,2,2,2,2,2,2,2,2,2,2,2,2,2,2,2,2,2,2,2,2,2,2,2,2,2,2,
2,2,2,2,2,2,2,2,2,2,2,2,2,2,2,2,2,2,2,2,2,2,2,2,2,2,2,2,2,2,2,2,2,2,2,2,
2,2,2,2,2,2,2,2,2,2,2,2,2,2,2,2,2,2,2,2,2,2,2,2,2,2,2,2,2,2,2,2,2,2,2,2,
2,2,2,2,2,2,2,2,2,2,2,2,2,2,2,2,2,2,2,2,2,2,2,2,2,2,2,2,2,2,2,2,2,2,2,2,
2,2,2,2,2,2,2,2,2,2,2,2,2,2,2,2,2,2,2,2,2,2,2,2,2,2,2,2,2,2,2,2,2,2,2,2,
2,2,2,2,2,2,2,2,2,2,2,2,2,2,2,2,2,2,2,2,2,2,2,2,2,2,2,2,2,2,2,2,2,2,2,2,
2,2,2,2,2,2,2,2,2,2,2,2,2,4),(-2.51381709144448,-2.4616943203403,-2.45636384935998,
-2.45229589263989,-2.4503884266314,-2.44892844628467,-2.44753723688448,
-2.44518212638536,-2.43883933923972,-2.39132865758641,-2.37432821273789,
-2.35422184584957,-2.35137005240454,-2.35045549044507,-2.3496938177306,
-2.34888308507486,-2.34784610220737,-2.3461874676665,-2.33745085149639,
-2.33318433166976,-2.32140295634083,-2.27597377532883,-2.26242688882561,
-2.25423253663617,-2.25161330702175,-2.25000925115995,-2.24855422004964,
-2.24668387186621,-2.24280799441645,-2.21017357382959,-2.17511733595217,
-2.15544239993991,-2.15305391245716,-2.15120094119025,-2.15021742027139,
-2.14948708218152,-2.14856556988473,-2.14697815647314,-2.14128080460466,
-2.0786233247721,-2.06353115175816,-2.05449563222558,-2.05187977319521,
-2.05027659292584,-2.04882157731506,-2.04695015901558,-2.04306812236764,
-2.00993617628532,-1.95824262510073,-1.95261989831584,-1.95111057341721,
-1.95020646723168,-1.94939102389445,-1.94833235332837,-1.9460267589751,
-1.91093287082707,-1.88024170872365,-1.8642950648383,-1.85486229851676,
-1.85222353402949,-1.85061511344793,-1.84916106513199,-1.84729885398925,
-1.844324736508,-1.83979389570394,-1.79155652170574,-1.7677523338987,-1.75832095640315,
-1.75291336925023,-1.7514243542899,-1.75052475162212,-1.74970796570809,
-1.74864034809405,-1.74628687915129,-1.72030802225369,-1.66873734036535,
-1.65570126133217,-1.65276682486339,-1.65109287021838,-1.64979326604914,
-1.64809239473104,-1.64511736847035,-1.64007469943735,-1.59192421493179,
-1.56806020222045,-1.55861480556869,-1.55320146741699,-1.55171191212857,
-1.55081219715275,-1.54999546090758,-1.54892811062603,-1.5465760358642,
-1.5208410503503,-1.49123725349215,-1.4605957813531,-1.45461987527319,-1.45239345271687,
-1.45087501438962,-1.44939727919356,-1.44762597562196,-1.44323349537697,
-1.44043071158282,-1.39183512808602,-1.3682776509208,-1.3589042029825,-1.35352043875533,
-1.35203368159175,-1.35113455630874,-1.35031757477421,-1.34924886078076,
-1.34688962417538,-1.31959140073318,-1.28267592549371,-1.25727990435006,
-1.25414782900595,-1.25225846264476,-1.25079626412085,-1.24921650240911,
-1.24670712555776,-1.2385161053402,-1.22536323324388,-1.1723454382188,-1.15505810065911,
-1.15305818353829,-1.15203399145868,-1.15127715654279,-1.15043984266644,
-1.14923748612129,-1.14616640606154,-1.13105297241606,-1.1010401044924,
-1.05816980319124,-1.05430246779117,-1.05243357103647,-1.05097847409879,
-1.04937313329847,-1.04674905873934,-1.03746901763568,-1.02187697914105,
-0.991434506836916,-0.972462001061123,-0.95536988070217,-0.953155426613753,
-0.952113905239302,-0.951300636924812,-0.950386719699435,-0.948833886215519,
-0.942724788106874,-0.931528276223083,-0.90168752149348,-0.858485925908308,
-0.854624189957158,-0.852756443087467,-0.851301544566228,-0.849695714900161,
-0.847069234922686,-0.837764107485972,-0.822113578063696,-0.791625637597253,
-0.755804495926459,-0.753510002657553,-0.752453304321176,-0.751638026076871,
-0.750732618418351,-0.749217909705027,-0.743538729456008,-0.733440390370134,
-0.706868042805538,-0.662549361485804,-0.65838064817793,-0.6551423391341,
-0.653221783663702,-0.651754588679456,-0.650188099119181,-0.647738950432579,
-0.64007190767818,-0.585135754711058,-0.556159379838001,-0.553797991958006,
-0.552728794028803,-0.551911653521997,-0.551012572867447,-0.549526363686655,
-0.544149547156414,-0.534794645763726,-0.511317516205744,-0.462636722700139,
-0.460428687641927,-0.455728777501401,-0.45385742087868,-0.452489216080156,
-0.451016400848921,-0.449028351186105,-0.444627824642235,-0.438690332297171,
-0.423764170729645,-0.373584920335847,-0.356206710964582,-0.35420447156368,
-0.353179651521646,-0.352422626435502,-0.351585406504917,-0.350383719761933,
-0.347467231191857,-0.312517085664562,-0.27794077061886,-0.27243982345828,
-0.258198609356565,-0.255335165775178,-0.253506514879707,-0.252055870905966,
-0.250427386356295,-0.24787127424443,-0.238625657250771,-0.223047353278985,
-0.190779561646613,-0.185490330609927,-0.15672656894149,-0.154364801672018,
-0.153295508070814,-0.152478326607812,-0.15157923551403,-0.150645997651498,
-0.147597906892484,-0.113426603515479,-0.100055212277475,-0.0874973804172144,
-0.0595262308992935,-0.0557308961226528,-0.0538760873696228,-0.0524225632821771,
-0.050809329075979,-0.0491448252879598,-0.0466820881505009,-0.0373021931558657,
-0.00059233830958253),.UNSPECIFIED.);
#792=B_SPLINE_CURVE_WITH_KNOTS('',3,(#15041,#15042,#15043,#15044,#15045,
#15046,#15047,#15048,#15049,#15050,#15051,#15052,#15053,#15054,#15055,#15056,
#15057,#15058,#15059,#15060,#15061,#15062,#15063,#15064,#15065,#15066,#15067,
#15068,#15069,#15070,#15071,#15072,#15073,#15074,#15075,#15076,#15077,#15078,
#15079,#15080,#15081,#15082,#15083,#15084,#15085,#15086,#15087,#15088,#15089,
#15090,#15091,#15092,#15093,#15094,#15095,#15096,#15097,#15098,#15099,#15100,
#15101,#15102,#15103,#15104,#15105,#15106,#15107,#15108,#15109,#15110,#15111,
#15112,#15113,#15114,#15115,#15116,#15117,#15118,#15119,#15120,#15121,#15122,
#15123,#15124,#15125,#15126,#15127,#15128,#15129,#15130,#15131,#15132,#15133,
#15134,#15135,#15136,#15137,#15138,#15139,#15140,#15141,#15142,#15143,#15144,
#15145,#15146,#15147,#15148,#15149,#15150,#15151,#15152,#15153,#15154,#15155,
#15156,#15157,#15158,#15159,#15160,#15161,#15162,#15163,#15164,#15165,#15166,
#15167,#15168,#15169,#15170,#15171,#15172,#15173,#15174,#15175,#15176,#15177,
#15178,#15179,#15180,#15181,#15182,#15183,#15184,#15185,#15186,#15187,#15188,
#15189,#15190,#15191,#15192,#15193,#15194,#15195,#15196,#15197,#15198,#15199,
#15200,#15201,#15202,#15203,#15204,#15205,#15206,#15207,#15208,#15209,#15210,
#15211,#15212,#15213,#15214,#15215,#15216,#15217,#15218,#15219,#15220,#15221,
#15222,#15223,#15224,#15225,#15226,#15227,#15228,#15229,#15230,#15231,#15232,
#15233,#15234,#15235,#15236,#15237,#15238,#15239,#15240,#15241,#15242,#15243,
#15244,#15245,#15246,#15247,#15248,#15249,#15250,#15251,#15252,#15253,#15254,
#15255,#15256,#15257,#15258,#15259,#15260,#15261,#15262,#15263,#15264,#15265,
#15266,#15267,#15268,#15269,#15270,#15271,#15272,#15273,#15274,#15275,#15276,
#15277,#15278,#15279,#15280,#15281,#15282,#15283,#15284,#15285,#15286,#15287,
#15288,#15289,#15290,#15291,#15292,#15293,#15294,#15295,#15296,#15297,#15298,
#15299,#15300,#15301,#15302,#15303,#15304,#15305,#15306,#15307,#15308,#15309,
#15310,#15311,#15312,#15313,#15314,#15315,#15316,#15317,#15318,#15319,#15320,
#15321,#15322,#15323,#15324,#15325,#15326,#15327,#15328,#15329,#15330,#15331,
#15332,#15333,#15334,#15335,#15336,#15337,#15338,#15339,#15340,#15341,#15342,
#15343,#15344,#15345,#15346,#15347,#15348,#15349,#15350,#15351,#15352,#15353,
#15354,#15355,#15356,#15357,#15358,#15359,#15360,#15361,#15362,#15363,#15364,
#15365,#15366,#15367,#15368,#15369,#15370,#15371,#15372,#15373,#15374,#15375,
#15376,#15377,#15378,#15379,#15380,#15381,#15382,#15383,#15384,#15385,#15386,
#15387,#15388,#15389,#15390,#15391,#15392,#15393,#15394,#15395,#15396,#15397,
#15398,#15399,#15400,#15401,#15402,#15403,#15404,#15405,#15406,#15407,#15408,
#15409,#15410,#15411,#15412,#15413,#15414,#15415,#15416,#15417,#15418,#15419,
#15420,#15421,#15422,#15423,#15424,#15425,#15426,#15427,#15428,#15429,#15430,
#15431,#15432,#15433,#15434,#15435,#15436,#15437,#15438,#15439,#15440,#15441,
#15442,#15443,#15444,#15445,#15446,#15447,#15448,#15449,#15450,#15451,#15452,
#15453,#15454,#15455,#15456,#15457,#15458,#15459,#15460,#15461,#15462,#15463,
#15464,#15465,#15466,#15467,#15468,#15469,#15470,#15471,#15472,#15473,#15474,
#15475,#15476,#15477,#15478,#15479,#15480,#15481,#15482,#15483,#15484,#15485,
#15486,#15487,#15488,#15489,#15490,#15491,#15492,#15493,#15494,#15495,#15496,
#15497,#15498,#15499,#15500,#15501,#15502,#15503,#15504,#15505,#15506,#15507,
#15508,#15509,#15510,#15511,#15512,#15513,#15514,#15515,#15516,#15517,#15518,
#15519,#15520,#15521,#15522,#15523,#15524),.UNSPECIFIED.,.F.,.F.,(4,2,2,
2,2,2,2,2,2,2,2,2,2,2,2,2,2,2,2,2,2,2,2,2,2,2,2,2,2,2,2,2,2,2,2,2,2,2,2,
2,2,2,2,2,2,2,2,2,2,2,2,2,2,2,2,2,2,2,2,2,2,2,2,2,2,2,2,2,2,2,2,2,2,2,2,
2,2,2,2,2,2,2,2,2,2,2,2,2,2,2,2,2,2,2,2,2,2,2,2,2,2,2,2,2,2,2,2,2,2,2,2,
2,2,2,2,2,2,2,2,2,2,2,2,2,2,2,2,2,2,2,2,2,2,2,2,2,2,2,2,2,2,2,2,2,2,2,2,
2,2,2,2,2,2,2,2,2,2,2,2,2,2,2,2,2,2,2,2,2,2,2,2,2,2,2,2,2,2,2,2,2,2,2,2,
2,2,2,2,2,2,2,2,2,2,2,2,2,2,2,2,2,2,2,2,2,2,2,2,2,2,2,2,2,2,2,2,2,2,2,2,
2,2,2,2,2,2,2,2,2,2,2,2,2,2,2,2,2,2,2,2,2,2,4),(-2.51387412169946,-2.47424051490727,
-2.47065529924497,-2.46886192572763,-2.46776045391495,-2.46674226431793,
-2.46601006212805,-2.46521357297149,-2.46379209649113,-2.45949943594632,
-2.42157509791276,-2.40265965364949,-2.37539707095867,-2.37006884777345,
-2.36842151295062,-2.36682021689027,-2.36536394954583,-2.3634867604667,
-2.3595776229956,-2.32316829797097,-2.28933548144493,-2.27619027760965,
-2.27166976445615,-2.26857687944786,-2.26764352786978,-2.26674436395602,
-2.26592716231359,-2.26485791302871,-2.26249650716216,-2.23448538417367,
-2.19399620985139,-2.17368780881667,-2.16974318254306,-2.1678290092893,
-2.16636767872935,-2.1649780229331,-2.16263245539582,-2.15635958599902,
-2.10691533695347,-2.07386515890655,-2.07077106158281,-2.06847499590965,
-2.06739387202363,-2.06657758679952,-2.06578838518536,-2.06440346976183,
-2.0603827891444,-2.05953942291496,-1.99611070678133,-1.98069450149456,
-1.97148937085782,-1.96887268915347,-1.96726895304265,-1.96581339911095,
-1.96394124103311,-1.9600574982783,-1.92689114075823,-1.87516991124119,
-1.86957187906321,-1.86806449333192,-1.86716061328382,-1.86634472155771,
-1.86528460557971,-1.86297250963142,-1.82826008456372,-1.79742618884047,
-1.78130531693621,-1.77179734699623,-1.76915064622207,-1.76754008538151,
-1.76608584957558,-1.76422581888903,-1.7604045258413,-1.7567183920104,-1.70831024876051,
-1.68460410373265,-1.6751944056072,-1.66979519786641,-1.6683066382996,-1.66740692978507,
-1.66658977771468,-1.66552132079175,-1.66316456551867,-1.63693672993607,
-1.58411719571013,-1.5723709882152,-1.56953029564355,-1.56787665283292,
-1.56642925993887,-1.56463823011855,-1.56189673040706,-1.5569125799063,
-1.50873421855757,-1.48486905510172,-1.4754220134025,-1.47000745112446,
-1.46851743071336,-1.46761740846391,-1.466800374639,-1.46573261057816,-1.46337952504495,
-1.43202708577063,-1.42677918752818,-1.39878364824676,-1.3820739368407,
-1.37231749372118,-1.36964695848821,-1.36803103750096,-1.36657783713793,
-1.36472721109611,-1.36095366066974,-1.31387223358467,-1.27518070365034,
-1.27184819960044,-1.26938965048138,-1.26829072386411,-1.26747175599771,
-1.26657748447456,-1.26511344090479,-1.26049015981145,-1.25730645828561,
-1.24235705005221,-1.19358789874244,-1.17398311092688,-1.17082998796573,
-1.16893409288588,-1.1674704923256,-1.16589283176416,-1.16339450754561,
-1.155306688426,-1.1423778782493,-1.09191565227756,-1.08659026653516,-1.07159020794651,
-1.06944149118093,-1.06840139167889,-1.06758999541161,-1.06666413621532,
-1.06505844069888,-1.05830190392628,-1.04535759819697,-1.02041660586387,
-0.974694866000277,-0.97088203294331,-0.969023546622891,-0.967569351476187,
-0.965957640192113,-0.96330630598602,-0.953752506466787,-0.937521908538539,
-0.906572610798441,-0.872091955684922,-0.869804100260906,-0.868732178535826,
-0.867914452795685,-0.867016335720977,-0.865535107965709,-0.860211962752534,
-0.850987452791029,-0.828065225811737,-0.778558549755146,-0.772301188735705,
-0.769957841512482,-0.768568486050967,-0.767106725081874,-0.765190752233494,
-0.761080879115719,-0.723613825523667,-0.68347320988439,-0.671828506745652,
-0.669841573602604,-0.668820726486177,-0.668011067774648,-0.667072144789106,
-0.665407190718475,-0.657830321581256,-0.608940431929072,-0.602873487396412,
-0.575103641001259,-0.571314960979271,-0.569461300428425,-0.568007717182066,
-0.566393430508175,-0.563730359592587,-0.554053285731037,-0.537530408990782,
-0.506354302789171,-0.487705740959814,-0.472319635423436,-0.470157320112599,
-0.469114591644733,-0.46830298489631,-0.467378923017734,-0.465781120450227,
-0.459125185032049,-0.44646004502937,-0.407521753046994,-0.375509390967726,
-0.371640989158788,-0.369771635651691,-0.3683162093041,-0.368313609442767,
-0.368311015553016,-0.368308427658644,-0.368305845741099,-0.368303269768205,
-0.368300699725793,-0.368298135594457,-0.366719163677803,-0.36417883826322,
-0.3611541885163,-0.355288692253156,-0.340618821769142,-0.30495590249967,
-0.283209842175027,-0.272292827981774,-0.27051577878822,-0.269454494549948,
-0.268638391572769,-0.267735017431447,-0.266230078767635,-0.26065888634933,
-0.208943721982646,-0.175765854701592,-0.171883523432426,-0.170011502656316,
-0.168555812686019,-0.167200259220575,-0.164974753350029,-0.158580383062122,
-0.149035158608648,-0.127500668087479,-0.0983596711902327,-0.0731308752864359,
-0.070779654450056,-0.0697122656681324,-0.0688953227586978,-0.0679951814165042,
-0.066504507876579,-0.0610826223315877,-0.0149734459364435,-0.000592883991003962),
 .UNSPECIFIED.);
#793=B_SPLINE_CURVE_WITH_KNOTS('',3,(#15526,#15527,#15528,#15529,#15530,
#15531,#15532,#15533,#15534,#15535,#15536,#15537,#15538,#15539,#15540,#15541,
#15542,#15543,#15544,#15545,#15546,#15547,#15548,#15549,#15550,#15551,#15552,
#15553,#15554,#15555,#15556,#15557,#15558,#15559,#15560,#15561,#15562,#15563,
#15564,#15565,#15566,#15567,#15568,#15569,#15570,#15571,#15572,#15573,#15574,
#15575,#15576,#15577,#15578,#15579,#15580,#15581,#15582,#15583,#15584,#15585,
#15586,#15587,#15588,#15589,#15590,#15591,#15592,#15593,#15594,#15595,#15596,
#15597,#15598,#15599,#15600,#15601,#15602,#15603,#15604,#15605,#15606,#15607,
#15608,#15609,#15610,#15611,#15612,#15613,#15614,#15615,#15616,#15617,#15618,
#15619,#15620,#15621,#15622,#15623,#15624,#15625,#15626,#15627,#15628,#15629,
#15630,#15631,#15632,#15633,#15634,#15635,#15636,#15637,#15638,#15639,#15640,
#15641,#15642,#15643,#15644,#15645,#15646,#15647,#15648,#15649,#15650,#15651,
#15652,#15653,#15654,#15655,#15656,#15657,#15658,#15659,#15660,#15661,#15662,
#15663,#15664,#15665,#15666,#15667,#15668,#15669,#15670,#15671,#15672,#15673,
#15674,#15675,#15676,#15677,#15678,#15679,#15680,#15681,#15682,#15683,#15684,
#15685,#15686,#15687,#15688,#15689,#15690,#15691,#15692,#15693,#15694,#15695,
#15696,#15697,#15698,#15699,#15700,#15701,#15702,#15703,#15704,#15705,#15706,
#15707,#15708,#15709,#15710,#15711,#15712,#15713,#15714,#15715,#15716,#15717,
#15718,#15719,#15720,#15721,#15722,#15723,#15724,#15725,#15726,#15727,#15728,
#15729,#15730,#15731,#15732,#15733,#15734,#15735,#15736,#15737,#15738,#15739,
#15740,#15741,#15742,#15743,#15744,#15745,#15746,#15747,#15748,#15749,#15750,
#15751,#15752,#15753,#15754,#15755,#15756,#15757,#15758,#15759,#15760,#15761,
#15762,#15763,#15764,#15765,#15766,#15767,#15768,#15769,#15770,#15771,#15772,
#15773,#15774,#15775,#15776,#15777,#15778,#15779,#15780,#15781,#15782,#15783,
#15784,#15785,#15786,#15787,#15788,#15789,#15790,#15791,#15792,#15793,#15794,
#15795,#15796,#15797,#15798,#15799,#15800,#15801,#15802,#15803,#15804,#15805,
#15806,#15807,#15808,#15809,#15810,#15811,#15812,#15813,#15814,#15815,#15816,
#15817,#15818,#15819,#15820,#15821,#15822,#15823,#15824,#15825,#15826,#15827,
#15828,#15829,#15830,#15831,#15832,#15833,#15834,#15835,#15836,#15837,#15838,
#15839,#15840,#15841,#15842,#15843,#15844,#15845,#15846,#15847,#15848,#15849,
#15850,#15851,#15852,#15853,#15854,#15855,#15856,#15857,#15858,#15859,#15860,
#15861,#15862,#15863,#15864,#15865,#15866,#15867,#15868,#15869,#15870,#15871,
#15872,#15873,#15874,#15875,#15876,#15877,#15878,#15879,#15880,#15881,#15882,
#15883,#15884,#15885,#15886,#15887,#15888,#15889,#15890,#15891,#15892,#15893,
#15894,#15895,#15896,#15897,#15898,#15899,#15900,#15901,#15902,#15903,#15904,
#15905,#15906,#15907,#15908,#15909,#15910,#15911,#15912,#15913,#15914,#15915,
#15916,#15917,#15918,#15919,#15920,#15921,#15922,#15923,#15924,#15925,#15926,
#15927,#15928,#15929,#15930,#15931,#15932,#15933,#15934,#15935,#15936,#15937,
#15938,#15939,#15940,#15941,#15942,#15943,#15944,#15945,#15946,#15947,#15948,
#15949,#15950,#15951,#15952,#15953,#15954,#15955,#15956,#15957,#15958,#15959,
#15960,#15961,#15962,#15963,#15964,#15965,#15966,#15967,#15968,#15969,#15970,
#15971,#15972,#15973,#15974,#15975,#15976,#15977,#15978,#15979,#15980,#15981,
#15982,#15983,#15984,#15985,#15986,#15987,#15988,#15989,#15990,#15991,#15992,
#15993,#15994,#15995,#15996,#15997,#15998,#15999,#16000,#16001,#16002,#16003,
#16004,#16005,#16006,#16007,#16008,#16009,#16010,#16011,#16012,#16013,#16014,
#16015,#16016,#16017),.UNSPECIFIED.,.F.,.F.,(4,2,2,2,2,2,2,2,2,2,2,2,2,
2,2,2,2,2,2,2,2,2,2,2,2,2,2,2,2,2,2,2,2,2,2,2,2,2,2,2,2,2,2,2,2,2,2,2,2,
2,2,2,2,2,2,2,2,2,2,2,2,2,2,2,2,2,2,2,2,2,2,2,2,2,2,2,2,2,2,2,2,2,2,2,2,
2,2,2,2,2,2,2,2,2,2,2,2,2,2,2,2,2,2,2,2,2,2,2,2,2,2,2,2,2,2,2,2,2,2,2,2,
2,2,2,2,2,2,2,2,2,2,2,2,2,2,2,2,2,2,2,2,2,2,2,2,2,2,2,2,2,2,2,2,2,2,2,2,
2,2,2,2,2,2,2,2,2,2,2,2,2,2,2,2,2,2,2,2,2,2,2,2,2,2,2,2,2,2,2,2,2,2,2,2,
2,2,2,2,2,2,2,2,2,2,2,2,2,2,2,2,2,2,2,2,2,2,2,2,2,2,2,2,2,2,2,2,2,2,2,2,
2,2,2,2,2,2,2,2,2,2,2,2,2,2,2,2,4),(-2.51333060447836,-2.49512983230018,
-2.48739716911243,-2.48522350706903,-2.48367799139685,-2.48232491170383,
-2.480862333055,-2.47896655172281,-2.47581096820282,-2.45610152696639,-2.45367957048176,
-2.44115764410605,-2.39258688301428,-2.38509332619115,-2.38343500197589,
-2.38249801260629,-2.38168889958435,-2.3806673002386,-2.37867459955377,
-2.36689794538597,-2.31562663635226,-2.29753853462042,-2.29074574367014,
-2.28738240505075,-2.28460723191478,-2.28297760776761,-2.28296984974125,
-2.2829619921872,-2.28295403358371,-2.28294597238488,-2.28293780702015,
-2.28292953589554,-2.28292115751315,-2.2814738439416,-2.27967050619776,
-2.27688682678902,-2.263793784105,-2.20345593376292,-2.18607702469524,-2.18403008716689,
-2.18301084009084,-2.18227886593025,-2.18148362130747,-2.18006682497597,
-2.17580565351732,-2.12913863406614,-2.09159276277847,-2.08799192750396,
-2.08585361230794,-2.08392971250419,-2.08248742401021,-2.08112037096703,
-2.07925161613137,-2.07456360181829,-2.07234178796808,-2.02366918642796,
-2.00018797528709,-1.99083407297192,-1.98545900047289,-1.9839734796391,
-1.98307486181455,-1.98225817079891,-1.98118960877375,-1.97882979714319,
-1.95091812639709,-1.89922297759728,-1.88803115452106,-1.88523600312759,
-1.88359318742138,-1.88214572230551,-1.88034212786995,-1.87755792403532,
-1.87255623832035,-1.82760452779704,-1.80148334203757,-1.79150175612692,
-1.78587079925225,-1.78436103358559,-1.783457014399,-1.78264189379707,-1.78158396503917,
-1.77928123694008,-1.74400931283244,-1.71339177420336,-1.69753153112137,
-1.6881365625347,-1.6855020529409,-1.68389491383127,-1.68244117114537,-1.68057816657373,
-1.67673790970057,-1.64637045593677,-1.60525906039829,-1.59295101130457,
-1.58642719358636,-1.58484058313001,-1.58391941224498,-1.58310800220936,
-1.58206242507518,-1.57988335043724,-1.56396213145341,-1.56035862718075,
-1.55531910366999,-1.51549578637999,-1.49850570343895,-1.48863439058073,
-1.48595432231957,-1.48433699802903,-1.48288532492683,-1.4810404586082,
-1.47812234922137,-1.46299243308917,-1.45911671122481,-1.40503623496431,
-1.39314669652792,-1.3867772291463,-1.38520296730797,-1.38428447375514,
-1.38347246111477,-1.38242215810779,-1.38021925465062,-1.36351367357653,
-1.31618168607164,-1.29895897895577,-1.28899117544015,-1.28630201567029,
-1.28468258338822,-1.28323116895794,-1.2813895624857,-1.27848237003607,
-1.2635324900243,-1.25959153704919,-1.25710657351285,-1.19821909763059,
-1.18773087683868,-1.18597578920766,-1.18492120771139,-1.18410635896853,
-1.18320011223132,-1.18168113203052,-1.17595311458867,-1.16573166023608,
-1.13870760724108,-1.09504822815608,-1.09144095134786,-1.08748379232594,
-1.08561791707192,-1.08415939141838,-1.08256896156834,-1.08001073900125,
-1.0713685148452,-1.05722444819886,-0.99761407634702,-0.987934035231894,
-0.986221350273743,-0.985179225793872,-0.984365926159305,-0.983452461527025,
-0.981901493133867,-0.975813396348231,-0.964671379336478,-0.934923235539195,
-0.891546167579989,-0.887690814054384,-0.885824394156436,-0.884369740014561,
-0.882763377619921,-0.880134202681171,-0.870800632583476,-0.855083584867605,
-0.824544298368596,-0.78888418118745,-0.786587924644967,-0.785530936827555,
-0.784715662306423,-0.783810506513335,-0.782296757155216,-0.77662728337384,
-0.766552901756687,-0.740071841816019,-0.695635521922242,-0.691794992877175,
-0.687989627370943,-0.686133080748478,-0.684679631758147,-0.683067955995739,
-0.680414861002306,-0.670835218872872,-0.654540932222524,-0.623549652583773,
-0.621229064560786,-0.589292506369531,-0.586947072784163,-0.585880929203905,
-0.58506435168189,-0.584163978393464,-0.58267157115461,-0.577228877233172,
-0.530685940186298,-0.492272965017269,-0.488360815026363,-0.486503477252888,
-0.485046052813652,-0.483451142820358,-0.48087315215765,-0.472044112075408,
-0.457482027055751,-0.394962607227355,-0.388412649716335,-0.386762655115358,
-0.385817286049692,-0.385028361912028,-0.384046630407367,-0.382977225585352,
-0.381261318831078,-0.377889443708013,-0.338178026259798,-0.292306479083492,
-0.288500533607447,-0.286643742969465,-0.285190120619366,-0.283578270758942,
-0.280924930870097,-0.271344852143821,-0.255050277372561,-0.225564576575613,
-0.214817149280862,-0.189807967755032,-0.187458270636641,-0.186391277191671,
-0.185590505211471,-0.184713395261896,-0.183312272936186,-0.181628829054493,
-0.178345268818256,-0.170034772719444,-0.135978374418879,-0.0927087360612524,
-0.0888492938507777,-0.0869820119315153,-0.0855271867967861,-0.0839211446664105,
-0.0812936506670929,-0.0719780352331019,-0.056303059782647,-0.000592941019645857),
 .UNSPECIFIED.);
#794=B_SPLINE_CURVE_WITH_KNOTS('',3,(#16019,#16020,#16021,#16022,#16023,
#16024,#16025,#16026,#16027,#16028,#16029,#16030,#16031,#16032,#16033,#16034,
#16035,#16036,#16037,#16038,#16039,#16040,#16041,#16042,#16043,#16044,#16045,
#16046,#16047,#16048,#16049,#16050,#16051,#16052,#16053,#16054,#16055,#16056,
#16057,#16058,#16059,#16060,#16061,#16062,#16063,#16064,#16065,#16066,#16067,
#16068,#16069,#16070,#16071,#16072,#16073,#16074,#16075,#16076,#16077,#16078,
#16079,#16080,#16081,#16082,#16083,#16084,#16085,#16086,#16087,#16088,#16089,
#16090,#16091,#16092,#16093,#16094,#16095,#16096,#16097,#16098,#16099,#16100,
#16101,#16102,#16103,#16104,#16105,#16106,#16107,#16108,#16109,#16110,#16111,
#16112,#16113,#16114,#16115,#16116,#16117,#16118,#16119,#16120,#16121,#16122,
#16123,#16124,#16125,#16126,#16127,#16128,#16129,#16130,#16131,#16132,#16133,
#16134,#16135,#16136,#16137,#16138,#16139,#16140,#16141,#16142,#16143,#16144,
#16145,#16146,#16147,#16148,#16149,#16150,#16151,#16152,#16153,#16154,#16155,
#16156,#16157,#16158,#16159,#16160,#16161,#16162,#16163,#16164,#16165,#16166,
#16167,#16168,#16169,#16170,#16171,#16172,#16173,#16174,#16175,#16176,#16177,
#16178,#16179,#16180,#16181,#16182,#16183,#16184,#16185,#16186,#16187,#16188,
#16189,#16190,#16191,#16192,#16193,#16194,#16195,#16196,#16197,#16198,#16199,
#16200,#16201,#16202,#16203,#16204,#16205,#16206,#16207,#16208),
 .UNSPECIFIED.,.F.,.F.,(4,3,3,3,3,3,3,3,3,3,3,3,3,3,3,3,3,3,3,3,3,3,3,3,
3,3,3,3,3,3,3,3,3,3,3,3,3,3,3,3,3,3,3,3,3,3,3,3,3,3,3,3,3,3,3,3,3,3,3,3,
3,3,3,4),(141.371669411541,141.444906084239,141.549851899103,141.654639964102,
141.759304494743,141.863903002535,141.968471071947,142.07304424328,142.177728198347,
142.282473261748,142.387401108208,142.4435869526,142.548532767464,142.653320832463,
142.757985363105,142.862583870896,142.967151940308,143.071725111641,143.176409066708,
143.281154130109,143.38608197657,143.442267820961,143.547213635825,143.652001700824,
143.756666231465,143.861264739257,143.965832808669,144.070405980001,144.175089935069,
144.279834998469,144.38476284493,144.440948689322,144.545894504186,144.650682569185,
144.755347099826,144.859945607618,144.96451367703,145.069086848362,145.173770803429,
145.27851586683,145.38344371329,145.439629557682,145.544575372546,145.649363437545,
145.754027968186,145.858626475978,145.96319454539,146.067767716722,146.172451671789,
146.27719673519,146.38212458165,146.438310426043,146.543256240907,146.648044305906,
146.752708836547,146.857307344339,146.961875413751,147.066448585084,147.171132540151,
147.275877603552,147.380805450012,147.436991294404,147.581269901374,147.654854718721),
 .UNSPECIFIED.);
#795=B_SPLINE_CURVE_WITH_KNOTS('',3,(#16210,#16211,#16212,#16213,#16214,
#16215,#16216,#16217,#16218,#16219,#16220,#16221,#16222,#16223,#16224,#16225,
#16226,#16227,#16228,#16229,#16230,#16231,#16232,#16233,#16234,#16235,#16236,
#16237,#16238,#16239,#16240,#16241,#16242,#16243,#16244,#16245,#16246,#16247,
#16248,#16249,#16250,#16251,#16252,#16253,#16254,#16255,#16256,#16257,#16258,
#16259,#16260,#16261,#16262,#16263,#16264,#16265,#16266,#16267,#16268,#16269,
#16270,#16271,#16272,#16273,#16274,#16275,#16276,#16277,#16278,#16279,#16280,
#16281,#16282,#16283,#16284,#16285,#16286,#16287,#16288,#16289,#16290,#16291,
#16292,#16293,#16294,#16295,#16296,#16297,#16298,#16299,#16300,#16301,#16302,
#16303,#16304,#16305,#16306,#16307,#16308,#16309,#16310,#16311,#16312,#16313,
#16314,#16315,#16316,#16317,#16318,#16319,#16320,#16321,#16322,#16323,#16324,
#16325,#16326,#16327,#16328,#16329,#16330,#16331,#16332,#16333,#16334,#16335,
#16336,#16337,#16338,#16339,#16340,#16341,#16342,#16343,#16344,#16345,#16346,
#16347,#16348,#16349,#16350,#16351,#16352,#16353,#16354,#16355,#16356,#16357,
#16358,#16359,#16360,#16361,#16362,#16363,#16364,#16365,#16366,#16367,#16368,
#16369,#16370,#16371,#16372,#16373,#16374,#16375,#16376,#16377,#16378,#16379,
#16380,#16381,#16382,#16383,#16384,#16385,#16386,#16387,#16388,#16389,#16390,
#16391,#16392,#16393,#16394,#16395,#16396,#16397,#16398,#16399,#16400,#16401,
#16402,#16403,#16404,#16405,#16406,#16407,#16408,#16409,#16410,#16411,#16412,
#16413,#16414,#16415,#16416,#16417,#16418,#16419,#16420,#16421,#16422,#16423,
#16424,#16425,#16426,#16427,#16428,#16429,#16430,#16431,#16432,#16433,#16434,
#16435,#16436,#16437,#16438,#16439,#16440,#16441,#16442,#16443,#16444,#16445,
#16446,#16447,#16448,#16449,#16450,#16451,#16452,#16453,#16454,#16455,#16456,
#16457,#16458,#16459,#16460,#16461,#16462,#16463,#16464,#16465,#16466,#16467,
#16468,#16469,#16470,#16471,#16472,#16473,#16474,#16475,#16476,#16477,#16478,
#16479,#16480,#16481,#16482,#16483,#16484,#16485,#16486,#16487,#16488,#16489,
#16490,#16491,#16492,#16493,#16494,#16495,#16496,#16497,#16498,#16499,#16500,
#16501,#16502,#16503,#16504,#16505,#16506,#16507,#16508,#16509,#16510,#16511,
#16512,#16513,#16514,#16515,#16516,#16517,#16518,#16519,#16520,#16521,#16522,
#16523,#16524,#16525,#16526,#16527,#16528,#16529,#16530,#16531,#16532,#16533,
#16534,#16535,#16536,#16537,#16538,#16539,#16540,#16541,#16542,#16543,#16544,
#16545,#16546,#16547,#16548,#16549,#16550,#16551,#16552,#16553,#16554,#16555,
#16556,#16557,#16558,#16559,#16560,#16561,#16562,#16563,#16564,#16565,#16566,
#16567,#16568,#16569,#16570,#16571,#16572,#16573,#16574,#16575,#16576,#16577,
#16578,#16579,#16580,#16581,#16582,#16583,#16584,#16585,#16586,#16587,#16588,
#16589,#16590,#16591,#16592,#16593,#16594,#16595,#16596,#16597,#16598,#16599,
#16600,#16601,#16602,#16603,#16604,#16605,#16606,#16607,#16608,#16609,#16610,
#16611,#16612,#16613,#16614,#16615,#16616,#16617,#16618,#16619,#16620,#16621,
#16622,#16623,#16624,#16625,#16626,#16627,#16628,#16629,#16630,#16631,#16632,
#16633,#16634,#16635,#16636,#16637,#16638,#16639,#16640,#16641,#16642,#16643,
#16644,#16645,#16646,#16647,#16648,#16649,#16650,#16651,#16652,#16653,#16654,
#16655,#16656,#16657,#16658,#16659,#16660,#16661,#16662,#16663,#16664,#16665,
#16666,#16667,#16668,#16669),.UNSPECIFIED.,.F.,.F.,(4,2,2,2,2,2,2,2,2,2,
2,2,2,2,2,2,2,2,2,2,2,2,2,2,2,2,2,2,2,2,2,2,2,2,2,2,2,2,2,2,2,2,2,2,2,2,
2,2,2,2,2,2,2,2,2,2,2,2,2,2,2,2,2,2,2,2,2,2,2,2,2,2,2,2,2,2,2,2,2,2,2,2,
2,2,2,2,2,2,2,2,2,2,2,2,2,2,2,2,2,2,2,2,2,2,2,2,2,2,2,2,2,2,2,2,2,2,2,2,
2,2,2,2,2,2,2,2,2,2,2,2,2,2,2,2,2,2,2,2,2,2,2,2,2,2,2,2,2,2,2,2,2,2,2,2,
2,2,2,2,2,2,2,2,2,2,2,2,2,2,2,2,2,2,2,2,2,2,2,2,2,2,2,2,2,2,2,2,2,2,2,2,
2,2,2,2,2,2,2,2,2,2,2,2,2,2,2,2,2,2,2,2,2,2,2,2,2,2,2,2,2,2,2,2,2,2,2,2,
2,2,2,4),(-2.51385606234959,-2.47289550666998,-2.46356794956306,-2.46111353504795,
-2.45945278962572,-2.45784236606457,-2.45638908982159,-2.45453144208573,
-2.45071914265189,-2.40504735754676,-2.38668764753374,-2.3626464817215,
-2.35959888299152,-2.3586659586041,-2.35776720741894,-2.35695038458105,
-2.35588163587887,-2.35352135528082,-2.32459325832703,-2.29654340663641,
-2.27463527058973,-2.26689177004872,-2.26146409540678,-2.25981102992099,
-2.25820593673958,-2.25675135916563,-2.25488354117365,-2.2510199230131,
-2.21923394508305,-2.17925802622926,-2.16716200873673,-2.16073636769438,
-2.15915933173981,-2.15823299936577,-2.15742225151546,-2.15638438753919,
-2.15424510202596,-2.13947833821309,-2.08573634478856,-2.07138609772281,
-2.06267867958504,-2.06018950617599,-2.05857215376388,-2.05712027059102,
-2.0552748847606,-2.0523554559506,-2.04772243049398,-1.99953752651721,-1.97570503865045,
-1.96626763202286,-1.96085781200313,-1.95936874075576,-1.95846921877153,
-1.95765258734327,-1.95658528009643,-1.95478665688354,-1.94340978003152,
-1.91799123012333,-1.88772698119719,-1.87231931385273,-1.86311869212441,
-1.86050300448751,-1.85889981677321,-1.85744472068075,-1.85557309562895,
-1.8516902564788,-1.81850816048406,-1.76677209309934,-1.76122514784952,
-1.75972286504623,-1.75882030654831,-1.75800439130672,-1.75694263174336,
-1.75516325271525,-1.74418860798185,-1.7213700173946,-1.69006124486661,
-1.6733213756367,-1.66355332823,-1.66088233559437,-1.6592666840574,-1.65781407615172,
-1.65596468476574,-1.65219533122811,-1.60502624999197,-1.57768488428766,
-1.56736687116784,-1.56160080505959,-1.56007822315026,-1.5591710950712,
-1.55835632361331,-1.55730299370152,-1.55502618203653,-1.51836063908331,
-1.48818819115999,-1.47290008543883,-1.46375087704527,-1.46114000320452,
-1.4595376828324,-1.45808200624963,-1.45620771633176,-1.45231239056028,
-1.41813895341619,-1.3696200900882,-1.36214515817374,-1.36048749067014,
-1.35955033309762,-1.35874073987037,-1.35771810242628,-1.35572208412949,
-1.34386197823689,-1.3234183275915,-1.30132873804255,-1.26646890964632,
-1.26243309055215,-1.26053148516619,-1.25907203090686,-1.25748285564766,
-1.25493161807489,-1.24635940399886,-1.23237234035762,-1.1737477686684,
-1.16292590825433,-1.16115360223897,-1.16009373147221,-1.15927785796119,
-1.15837380527384,-1.15686572494401,-1.15126049497782,-1.09956355010413,
-1.0664137758482,-1.06253011394748,-1.06065787825693,-1.05920221136876,
-1.05759829748458,-1.05498120590484,-1.04577347292208,-1.03034944725737,
-1.00003824854281,-0.974444453268759,-0.963217081629322,-0.961425080661047,
-0.960359485519636,-0.959542836383574,-0.958641852747923,-0.957147301611772,
-0.951684564572241,-0.904750413416738,-0.866727949660168,-0.862816791798437,
-0.860939257541546,-0.859482998580386,-0.857881989878447,-0.855277644510307,
-0.846195533357814,-0.831059900270178,-0.800981318644419,-0.76392248464805,
-0.761650983747574,-0.76059854805586,-0.759783785527602,-0.758875911574715,
-0.757350430041585,-0.751554121543871,-0.741161930845878,-0.713611615629383,
-0.666803003257231,-0.663023986710399,-0.661172484336627,-0.65971941981336,
-0.658104499610478,-0.655437586305811,-0.645716022975051,-0.62908574926352,
-0.597830214320749,-0.576207056548242,-0.57539762546806,-0.563810642904664,
-0.561827083870032,-0.560807127637897,-0.559997738146478,-0.559058629711448,
-0.557392114679074,-0.549787528579539,-0.500782834838224,-0.46726483750101,
-0.463377037633508,-0.461504163055148,-0.460048603246971,-0.458445418112704,
-0.455830894810249,-0.446813098092226,-0.43176098598118,-0.374633903527819,
-0.36395183998955,-0.36218657607293,-0.361128814582881,-0.360313290673357,
-0.359408236747614,-0.357925866044045,-0.352588346756007,-0.301099518212894,
-0.267469031499313,-0.263579584304299,-0.261706300654746,-0.260250594069233,
-0.258647420319844,-0.256033306141193,-0.247877597067883,-0.234418582662184,
-0.192651244087699,-0.164825145006643,-0.16246394362629,-0.161394755778702,
-0.160577591547324,-0.159678450950414,-0.158745141000032,-0.155696274999276,
-0.133638589593711,-0.116108185495929,-0.0714612337013633,-0.0674036936796014,
-0.0637812838962045,-0.0619364316131628,-0.0604840974397912,-0.0588653394882416,
-0.0561812706654817,-0.0530006397652199,-0.0467126239847654,-0.000592616177282767),
 .UNSPECIFIED.);
#796=B_SPLINE_CURVE_WITH_KNOTS('',3,(#16671,#16672,#16673,#16674,#16675,
#16676,#16677,#16678,#16679,#16680,#16681,#16682,#16683,#16684,#16685,#16686,
#16687,#16688,#16689,#16690,#16691,#16692,#16693,#16694,#16695,#16696,#16697,
#16698,#16699,#16700,#16701,#16702,#16703,#16704,#16705,#16706,#16707,#16708,
#16709,#16710,#16711,#16712,#16713,#16714,#16715,#16716,#16717,#16718,#16719,
#16720,#16721,#16722,#16723,#16724,#16725,#16726,#16727,#16728,#16729,#16730,
#16731,#16732,#16733,#16734,#16735,#16736,#16737,#16738,#16739,#16740,#16741,
#16742,#16743,#16744,#16745,#16746,#16747,#16748,#16749,#16750,#16751,#16752,
#16753,#16754,#16755,#16756,#16757,#16758,#16759,#16760,#16761,#16762,#16763,
#16764,#16765,#16766,#16767,#16768,#16769,#16770,#16771,#16772,#16773,#16774,
#16775,#16776,#16777,#16778,#16779,#16780,#16781,#16782,#16783,#16784,#16785,
#16786,#16787,#16788,#16789,#16790,#16791,#16792,#16793,#16794,#16795,#16796,
#16797,#16798,#16799,#16800,#16801,#16802,#16803,#16804,#16805,#16806,#16807,
#16808,#16809,#16810,#16811,#16812,#16813,#16814,#16815,#16816,#16817,#16818,
#16819,#16820,#16821,#16822,#16823,#16824,#16825,#16826,#16827,#16828,#16829,
#16830,#16831,#16832,#16833,#16834,#16835,#16836,#16837,#16838,#16839,#16840,
#16841,#16842,#16843,#16844,#16845,#16846,#16847,#16848,#16849,#16850,#16851,
#16852,#16853,#16854,#16855,#16856,#16857,#16858,#16859,#16860,#16861,#16862,
#16863,#16864,#16865,#16866,#16867,#16868,#16869,#16870,#16871,#16872,#16873,
#16874,#16875,#16876,#16877,#16878,#16879,#16880,#16881,#16882,#16883,#16884,
#16885,#16886,#16887,#16888,#16889,#16890,#16891,#16892,#16893,#16894,#16895,
#16896,#16897,#16898,#16899,#16900,#16901,#16902,#16903,#16904,#16905,#16906,
#16907,#16908,#16909,#16910,#16911,#16912,#16913,#16914,#16915,#16916,#16917,
#16918,#16919,#16920,#16921,#16922,#16923,#16924,#16925,#16926,#16927,#16928,
#16929,#16930,#16931,#16932,#16933,#16934,#16935,#16936,#16937,#16938,#16939,
#16940,#16941,#16942,#16943,#16944,#16945,#16946,#16947,#16948,#16949,#16950,
#16951,#16952,#16953,#16954,#16955,#16956,#16957,#16958,#16959,#16960,#16961,
#16962,#16963,#16964,#16965,#16966,#16967,#16968,#16969,#16970,#16971,#16972,
#16973,#16974,#16975,#16976,#16977,#16978,#16979,#16980,#16981,#16982,#16983,
#16984,#16985,#16986,#16987,#16988,#16989,#16990,#16991,#16992,#16993,#16994,
#16995,#16996,#16997,#16998,#16999,#17000,#17001,#17002,#17003,#17004,#17005,
#17006,#17007,#17008,#17009,#17010,#17011,#17012,#17013,#17014,#17015,#17016,
#17017,#17018,#17019,#17020,#17021,#17022,#17023,#17024,#17025,#17026,#17027,
#17028,#17029,#17030,#17031,#17032,#17033,#17034,#17035,#17036,#17037,#17038,
#17039,#17040,#17041,#17042,#17043,#17044,#17045,#17046,#17047,#17048,#17049,
#17050,#17051,#17052,#17053,#17054,#17055,#17056,#17057,#17058,#17059,#17060,
#17061,#17062,#17063,#17064,#17065,#17066,#17067,#17068,#17069,#17070,#17071,
#17072,#17073,#17074,#17075,#17076,#17077,#17078,#17079,#17080,#17081,#17082,
#17083,#17084,#17085,#17086,#17087,#17088,#17089,#17090,#17091,#17092,#17093,
#17094,#17095,#17096,#17097,#17098,#17099,#17100,#17101,#17102,#17103,#17104,
#17105,#17106,#17107,#17108,#17109,#17110,#17111,#17112,#17113,#17114,#17115,
#17116,#17117,#17118,#17119,#17120,#17121,#17122,#17123,#17124,#17125,#17126,
#17127,#17128,#17129,#17130,#17131,#17132,#17133,#17134,#17135,#17136,#17137,
#17138,#17139,#17140,#17141,#17142,#17143,#17144,#17145,#17146,#17147,#17148,
#17149,#17150,#17151,#17152,#17153,#17154,#17155,#17156,#17157,#17158,#17159,
#17160,#17161,#17162,#17163,#17164,#17165,#17166,#17167,#17168,#17169,#17170,
#17171,#17172,#17173,#17174,#17175,#17176,#17177,#17178,#17179,#17180),
 .UNSPECIFIED.,.F.,.F.,(4,2,2,2,2,2,2,2,2,2,2,2,2,2,2,2,2,2,2,2,2,2,2,2,
2,2,2,2,2,2,2,2,2,2,2,2,2,2,2,2,2,2,2,2,2,2,2,2,2,2,2,2,2,2,2,2,2,2,2,2,
2,2,2,2,2,2,2,2,2,2,2,2,2,2,2,2,2,2,2,2,2,2,2,2,2,2,2,2,2,2,2,2,2,2,2,2,
2,2,2,2,2,2,2,2,2,2,2,2,2,2,2,2,2,2,2,2,2,2,2,2,2,2,2,2,2,2,2,2,2,2,2,2,
2,2,2,2,2,2,2,2,2,2,2,2,2,2,2,2,2,2,2,2,2,2,2,2,2,2,2,2,2,2,2,2,2,2,2,2,
2,2,2,2,2,2,2,2,2,2,2,2,2,2,2,2,2,2,2,2,2,2,2,2,2,2,2,2,2,2,2,2,2,2,2,2,
2,2,2,2,2,2,2,2,2,2,2,2,2,2,2,2,2,2,2,2,2,2,2,2,2,2,2,2,2,2,2,2,2,2,2,2,
2,2,2,2,2,2,2,2,2,2,2,2,2,2,4),(-2.51290263866645,-2.47973011981934,-2.47687838336318,
-2.4754543019939,-2.47450637763105,-2.47359717657777,-2.47278313890905,
-2.47173415476316,-2.46999790889112,-2.45987326217793,-2.43689520006323,
-2.42523894652728,-2.41513819529139,-2.38741498789146,-2.37825479294101,
-2.37562306929992,-2.37401630677287,-2.37256204358753,-2.37069717403871,
-2.36684878503042,-2.32278899666483,-2.2907434005837,-2.28159864658033,
-2.27633001841743,-2.27485682249618,-2.27395406575148,-2.27313829126578,
-2.27207713911402,-2.27029968474887,-2.25936226367964,-2.24654594397127,
-2.20142200124546,-2.18715731591929,-2.17860961507587,-2.17596952937816,
-2.17436088760221,-2.17290701841427,-2.17104556262997,-2.16807370470927,
-2.15208061106345,-2.14310410972149,-2.09637996204847,-2.08358561876969,
-2.07690028803354,-2.07530564152039,-2.07437529290822,-2.07356505117363,
-2.07253308948188,-2.07049294734063,-2.05761840199576,-2.05179205883425,
-2.01952404619975,-1.98145347040855,-1.97732896905583,-1.97541074887351,
-1.9739492038865,-1.97256149495135,-1.97022442220972,-1.96400845617728,
-1.91379525965114,-1.89325566706623,-1.88286096088637,-1.87706461298844,
-1.87553935050035,-1.87463165560911,-1.87381708342562,-1.87276494088064,
-1.87049423633264,-1.83336638788513,-1.80335267529129,-1.78062290291438,
-1.77722326985005,-1.77544932620379,-1.77414240546558,-1.77272761853201,
-1.77025329768429,-1.76410827515316,-1.71785869438524,-1.67957896568547,
-1.67664367443911,-1.67546301316162,-1.6746300030873,-1.67386895169163,
-1.67282797682456,-1.67076186678387,-1.63497006790056,-1.60450569083791,
-1.58885034863243,-1.5795421742219,-1.5769154276754,-1.57530955561765,-1.57385469711829,
-1.57198711109074,-1.56812610418335,-1.52486297318037,-1.49501981977373,
-1.48383720702256,-1.47773407080385,-1.47618175485276,-1.47526796178253,
-1.47445467905634,-1.47341298503938,-1.4717018526904,-1.46205089338169,
-1.45888748788825,-1.40401280454187,-1.38885755828111,-1.37976632101085,
-1.37716134329457,-1.37556036666545,-1.37410441372813,-1.37222766355903,
-1.36831956269003,-1.33201740601209,-1.29816353075714,-1.28497028464304,
-1.27812668621169,-1.27651478412686,-1.2755877887263,-1.27477696442944,
-1.27373966454656,-1.27160380759659,-1.25693941156251,-1.23050542730217,
-1.18600250189791,-1.18209614667404,-1.17833294029778,-1.17648475236689,
-1.17503225814045,-1.17341587345087,-1.17074167409172,-1.16093994983232,
-1.14411690791391,-1.11271461474076,-1.08943789072646,-1.07903767343225,
-1.07728693542252,-1.07623357895926,-1.07541882888513,-1.07451176338701,
-1.07298938074197,-1.06722507935204,-1.05691280156251,-1.0295934499279,
-0.982439373647723,-0.978670629694255,-0.976821397650103,-0.97536885029814,
-0.973753199333288,-0.971082053494814,-0.961311822767727,-0.944563885643717,
-0.913220829775399,-0.890278788010786,-0.879419393404867,-0.877645695181092,
-0.876585617404193,-0.875769962364344,-0.874866562534489,-0.873360457273545,
-0.867772451398172,-0.816088873812106,-0.782939753848354,-0.779057389371201,
-0.777185822610964,-0.775730695191473,-0.774127395324874,-0.771511349941322,
-0.762307749492934,-0.746891087061412,-0.716592481286442,-0.69099289446969,
-0.679780396665591,-0.677989579009808,-0.676924531926145,-0.676108209665247,
-0.675207485965857,-0.673713151295325,-0.668248881839877,-0.621259459467422,
-0.583328322254114,-0.579418498201252,-0.577541640178106,-0.576085921637413,
-0.574485523106977,-0.571882206311651,-0.562804042799036,-0.547675335952938,
-0.517609013257925,-0.480561084133031,-0.478290396652119,-0.477238347288493,
-0.476423887995528,-0.475516356485675,-0.473991460344343,-0.468197492753957,
-0.457809629451998,-0.430272445371526,-0.383480207330429,-0.379701074965947,
-0.377849960450568,-0.376397403387119,-0.374920448077874,-0.37246596139373,
-0.369568108065626,-0.3640392875826,-0.350536032217847,-0.294888758217795,
-0.292140623241821,-0.280461447916172,-0.278473422570434,-0.27745264000543,
-0.276643356604188,-0.275705237214562,-0.274042618433334,-0.266491524910349,
-0.217715711568212,-0.183932697841923,-0.180044256181476,-0.178171513528571,
-0.176716252580075,-0.176698987716623,-0.176682356260034,-0.176666329637557,
-0.176650880787118,-0.176635984134886,-0.176621615491089,-0.176607751969285,
-0.176594371908458,-0.176581454781815,-0.176568981136048,-0.176556932521543,
-0.176545291430695,-0.176534041245863,-0.176523166174698,-0.17651265120998,
-0.176502482077711,-0.17649264519348,-0.176483127621512,-0.176473917056579,
-0.176465001764495,-0.174809102909438,-0.171925927210577,-0.168397887116606,
-0.161144032794144,-0.141248451103759,-0.0830076872079403,-0.0794405920852786,
-0.0781220096349165,-0.0773459935269317,-0.076523549719491,-0.0754022315016852,
-0.0728184844714701,-0.0409558825915921,-0.000592896245600241),
 .UNSPECIFIED.);
#797=B_SPLINE_CURVE_WITH_KNOTS('',3,(#17182,#17183,#17184,#17185,#17186,
#17187,#17188,#17189,#17190,#17191,#17192,#17193,#17194,#17195,#17196,#17197,
#17198,#17199,#17200,#17201,#17202,#17203,#17204,#17205,#17206,#17207,#17208,
#17209,#17210,#17211,#17212,#17213,#17214,#17215,#17216,#17217,#17218,#17219,
#17220,#17221,#17222,#17223,#17224,#17225,#17226,#17227,#17228,#17229,#17230,
#17231,#17232,#17233,#17234,#17235,#17236,#17237,#17238,#17239,#17240,#17241,
#17242,#17243,#17244,#17245,#17246,#17247,#17248,#17249,#17250,#17251,#17252,
#17253,#17254,#17255,#17256,#17257,#17258,#17259,#17260,#17261,#17262,#17263,
#17264,#17265,#17266,#17267,#17268,#17269,#17270,#17271,#17272,#17273,#17274,
#17275,#17276,#17277,#17278,#17279,#17280,#17281,#17282,#17283,#17284,#17285,
#17286,#17287,#17288,#17289,#17290,#17291,#17292,#17293,#17294,#17295,#17296,
#17297,#17298,#17299,#17300,#17301,#17302,#17303,#17304,#17305,#17306,#17307,
#17308,#17309,#17310,#17311,#17312,#17313,#17314,#17315,#17316,#17317,#17318,
#17319,#17320,#17321,#17322,#17323,#17324,#17325,#17326,#17327,#17328,#17329,
#17330,#17331,#17332,#17333,#17334,#17335,#17336,#17337,#17338,#17339,#17340,
#17341,#17342,#17343,#17344,#17345,#17346,#17347,#17348,#17349,#17350,#17351,
#17352,#17353,#17354,#17355,#17356,#17357,#17358,#17359,#17360,#17361,#17362,
#17363,#17364,#17365,#17366,#17367,#17368,#17369,#17370,#17371,#17372,#17373,
#17374,#17375,#17376,#17377,#17378,#17379,#17380,#17381,#17382,#17383,#17384,
#17385,#17386,#17387,#17388,#17389,#17390,#17391,#17392,#17393,#17394,#17395,
#17396,#17397,#17398,#17399,#17400,#17401,#17402,#17403,#17404,#17405,#17406,
#17407,#17408,#17409,#17410,#17411,#17412,#17413,#17414,#17415,#17416,#17417,
#17418,#17419,#17420,#17421,#17422,#17423,#17424,#17425,#17426,#17427,#17428,
#17429,#17430,#17431,#17432,#17433,#17434,#17435,#17436,#17437,#17438,#17439,
#17440,#17441,#17442,#17443,#17444,#17445,#17446,#17447,#17448,#17449,#17450,
#17451,#17452,#17453,#17454,#17455,#17456,#17457,#17458,#17459,#17460,#17461,
#17462,#17463,#17464,#17465,#17466,#17467,#17468,#17469,#17470,#17471,#17472,
#17473,#17474,#17475,#17476,#17477,#17478,#17479,#17480,#17481,#17482,#17483,
#17484,#17485,#17486,#17487,#17488,#17489,#17490,#17491,#17492,#17493,#17494,
#17495,#17496,#17497,#17498,#17499,#17500,#17501,#17502,#17503,#17504,#17505,
#17506,#17507,#17508,#17509,#17510,#17511,#17512,#17513,#17514,#17515,#17516,
#17517,#17518,#17519,#17520,#17521,#17522,#17523,#17524,#17525,#17526,#17527,
#17528,#17529,#17530,#17531,#17532,#17533,#17534,#17535,#17536,#17537,#17538,
#17539,#17540,#17541,#17542,#17543,#17544,#17545,#17546,#17547,#17548,#17549,
#17550,#17551,#17552,#17553,#17554,#17555,#17556,#17557,#17558,#17559,#17560,
#17561,#17562,#17563,#17564,#17565,#17566,#17567,#17568,#17569,#17570,#17571,
#17572,#17573,#17574,#17575,#17576,#17577,#17578,#17579,#17580,#17581,#17582,
#17583,#17584,#17585,#17586,#17587,#17588,#17589,#17590,#17591,#17592,#17593,
#17594,#17595,#17596,#17597,#17598,#17599,#17600,#17601,#17602,#17603,#17604,
#17605,#17606,#17607,#17608,#17609,#17610,#17611,#17612,#17613,#17614,#17615,
#17616,#17617,#17618,#17619,#17620,#17621,#17622,#17623,#17624,#17625,#17626,
#17627,#17628,#17629,#17630,#17631,#17632,#17633,#17634,#17635,#17636,#17637,
#17638,#17639,#17640,#17641,#17642,#17643,#17644,#17645,#17646,#17647,#17648,
#17649,#17650,#17651,#17652,#17653,#17654,#17655,#17656,#17657,#17658,#17659,
#17660,#17661,#17662,#17663,#17664,#17665,#17666,#17667,#17668,#17669,#17670,
#17671,#17672,#17673,#17674,#17675,#17676,#17677,#17678,#17679,#17680,#17681,
#17682,#17683,#17684,#17685,#17686,#17687,#17688,#17689,#17690,#17691,#17692,
#17693,#17694,#17695,#17696,#17697,#17698,#17699,#17700,#17701,#17702,#17703,
#17704,#17705,#17706,#17707,#17708,#17709,#17710,#17711,#17712,#17713,#17714,
#17715,#17716,#17717,#17718,#17719,#17720,#17721,#17722,#17723,#17724,#17725,
#17726,#17727,#17728,#17729,#17730,#17731,#17732,#17733,#17734,#17735,#17736,
#17737,#17738,#17739,#17740,#17741,#17742,#17743,#17744,#17745,#17746,#17747,
#17748,#17749,#17750,#17751,#17752,#17753,#17754,#17755,#17756,#17757,#17758,
#17759,#17760,#17761,#17762,#17763,#17764,#17765,#17766,#17767,#17768,#17769,
#17770,#17771),.UNSPECIFIED.,.F.,.F.,(4,2,2,2,2,2,2,2,2,2,2,2,2,2,2,2,2,
2,2,2,2,2,2,2,2,2,2,2,2,2,2,2,2,2,2,2,2,2,2,2,2,2,2,2,2,2,2,2,2,2,2,2,2,
2,2,2,2,2,2,2,2,2,2,2,2,2,2,2,2,2,2,2,2,2,2,2,2,2,2,2,2,2,2,2,2,2,2,2,2,
2,2,2,2,2,2,2,2,2,2,2,2,2,2,2,2,2,2,2,2,2,2,2,2,2,2,2,2,2,2,2,2,2,2,2,2,
2,2,2,2,2,2,2,2,2,2,2,2,2,2,2,2,2,2,2,2,2,2,2,2,2,2,2,2,2,2,2,2,2,2,2,2,
2,2,2,2,2,2,2,2,2,2,2,2,2,2,2,2,2,2,2,2,2,2,2,2,2,2,2,2,2,2,2,2,2,2,2,2,
2,2,2,2,2,2,2,2,2,2,2,2,2,2,2,2,2,2,2,2,2,2,2,2,2,2,2,2,2,2,2,2,2,2,2,2,
2,2,2,2,2,2,2,2,2,2,2,2,2,2,2,2,2,2,2,2,2,2,2,2,2,2,2,2,2,2,2,2,2,2,2,2,
2,2,2,2,2,2,2,2,2,2,2,2,2,2,2,2,2,2,2,2,2,2,2,2,2,4),(-2.5085577871456,
-2.49262769230154,-2.48973435213939,-2.48789106392997,-2.48647124813858,
-2.48508379812839,-2.48370772053238,-2.48142077175534,-2.47549771094919,
-2.47408501189765,-2.47255980809686,-2.46873366496435,-2.45991519426738,
-2.40424748579275,-2.39404164677233,-2.38832358910043,-2.3868074239447,
-2.38590289490233,-2.38508961313634,-2.38403709775285,-2.38228553318593,
-2.3718202117363,-2.36966228132628,-2.31948581048527,-2.30125336278384,
-2.2944264626496,-2.29105236712866,-2.28826698358676,-2.28663851850139,
-2.28663067064916,-2.28662272345487,-2.28661467543457,-2.28660652510974,
-2.28659827095719,-2.28658991144072,-2.2865814450022,-2.28657287005424,
-2.28656418497052,-2.28655538811812,-2.2865464778247,-2.28653745239372,
-2.28652830984985,-2.28651955427403,-2.28651030289548,-2.28650052715088,
-2.28649019680124,-2.28647927996775,-2.28502880740622,-2.28317527238802,
-2.2793732862155,-2.25099595887576,-2.21419312138386,-2.19740890154388,
-2.18937661615718,-2.18768474224462,-2.18674137401547,-2.18593440908957,
-2.18492527086308,-2.18335403892253,-2.17589274737912,-2.1144368056051,
-2.10002498690207,-2.09423685596148,-2.0912431577006,-2.08871494933066,
-2.08714624463599,-2.08569445045336,-2.08382894116673,-2.07996553795128,
-2.04779673602627,-2.01097855770539,-1.99705169007737,-1.98995668162642,
-1.98832857206545,-1.98739927327844,-1.98659089164357,-1.9855625315347,
-1.98353329134673,-1.97084294733751,-1.94685960502824,-1.91667531680973,
-1.90132215607051,-1.8921502882157,-1.88954092074849,-1.88794121408498,
-1.88648902004258,-1.88462076714932,-1.88074361809504,-1.8477928275812,
-1.8448442168733,-1.8107340838666,-1.79755487682282,-1.7907210379829,-1.78911228750673,
-1.78818724783696,-1.78737822616853,-1.78634335323482,-1.78421290661734,
-1.76959990887754,-1.76504705565105,-1.74816118623124,-1.71780408648842,
-1.70223399560629,-1.69296821139032,-1.69034942535417,-1.6887475801415,
-1.68729582134265,-1.68543144899528,-1.68157433216095,-1.6387494611109,
-1.60879460180205,-1.59752778361971,-1.59139651382713,-1.58984407923392,
-1.58893151444945,-1.58812019598414,-1.5870821456267,-1.58537931282474,
-1.57583137057058,-1.51628502899276,-1.5021563696958,-1.49644926850228,
-1.49215545041037,-1.49020807995149,-1.48874461413679,-1.4873699741117,
-1.48509017609615,-1.47921265445488,-1.44838403368757,-1.39977699740586,
-1.3922634976555,-1.39060578928645,-1.3896699260512,-1.38886226783422,-1.38784312635858,
-1.38585707514599,-1.37416145435572,-1.32286906489092,-1.30484185569655,
-1.29455155839888,-1.29183658750595,-1.29021337524731,-1.28876598453411,
-1.28693949272978,-1.28407564608855,-1.2697554438151,-1.26572524824921,
-1.25459880813904,-1.20236843252919,-1.1933193812704,-1.19164438808857,
-1.19060353149748,-1.18979384092836,-1.18887246850041,-1.18728050255747,
-1.18066543079516,-1.16809914869998,-1.12891292499655,-1.09722064982594,
-1.09336508253521,-1.09150096717359,-1.09004918758919,-1.08844709507886,
-1.08582739633415,-1.07655320042075,-1.06096150002224,-1.0305595962796,
-1.02818175359588,-1.00602709186288,-0.994340258008126,-0.992354643852799,
-0.99133558839003,-0.990527927343633,-0.989591976100997,-0.987933909679917,
-0.980415261503741,-0.93180549014593,-0.89800988569456,-0.89412669165631,
-0.892257242704192,-0.89080488210923,-0.889205763314542,-0.886599095726911,
-0.877454453400216,-0.862161797096055,-0.831999139486753,-0.825847376604896,
-0.795619172790457,-0.793265844149407,-0.792199620432507,-0.791384467530498,
-0.790487266337861,-0.789003513181577,-0.783628672569723,-0.77426996911521,
-0.75073873339369,-0.702330226388538,-0.699258405472533,-0.695058802223551,
-0.693149760888062,-0.691687092373907,-0.690121278343756,-0.687664512576643,
-0.679902703535731,-0.625203211144041,-0.605903288709666,-0.595665610335983,
-0.593925828127673,-0.592876851229636,-0.592064133232738,-0.59115784240309,
-0.589633493580023,-0.583823599192919,-0.573386973941746,-0.545516872100343,
-0.499325996353757,-0.495542031327326,-0.493692126837332,-0.492242149017347,
-0.490632545348288,-0.487978766637682,-0.478352458886552,-0.461933656358038,
-0.430885367087165,-0.397031003067011,-0.394942095644275,-0.393896536196289,
-0.393135388384886,-0.392323563413582,-0.391189530092257,-0.389905135173534,
-0.387659660595867,-0.370202075436377,-0.335835335094181,-0.300276883913584,
-0.296379715526992,-0.29450752219128,-0.293054796427331,-0.291457057932786,
-0.288856651701757,-0.279774425148854,-0.264625233629228,-0.232496029252278,
-0.197782587315697,-0.195475885596427,-0.19441830401704,-0.193626902941515,
-0.193624263440276,-0.193621647425824,-0.193619050614331,-0.193616472797433,
-0.193613913790316,-0.193611373374273,-0.19360885134042,-0.193606347546237,
-0.19360386179843,-0.193601393895626,-0.193598943609693,-0.193596510792769,
-0.193594095275384,-0.193591696867853,-0.193589315413587,-0.19358695071515,
-0.193584602616196,-0.193582270959006,-0.193579955568018,-0.193577656292972,
-0.193575372969015,-0.193573105428499,-0.193570853517458,-0.193568617102638,
-0.193566395995654,-0.193564190067784,-0.193561999162903,-0.193559823161396,
-0.19355766189653,-0.193555515215056,-0.193553376672008,-0.193551239611196,
-0.193549116423135,-0.19264500912432,-0.191684908487208,-0.190231650513649,
-0.187558430343268,-0.162977944106383,-0.130155513385122,-0.100730850391224,
-0.0969068410978159,-0.0950466372798334,-0.0935927848156704,-0.0919831789769273,
-0.0893392632049909,-0.0798542638730792,-0.0637828867096131,-0.000620331519808279),
 .UNSPECIFIED.);
#798=B_SPLINE_CURVE_WITH_KNOTS('',3,(#17773,#17774,#17775,#17776,#17777,
#17778,#17779,#17780,#17781,#17782,#17783),.UNSPECIFIED.,.F.,.F.,(4,1,1,
1,1,1,1,1,4),(185.353966561798,185.386864292112,186.385545160473,187.384226028834,
188.382906897195,189.381587765555,190.380268633916,191.378949502277,191.637149496705),
 .UNSPECIFIED.);
#799=B_SPLINE_CURVE_WITH_KNOTS('',3,(#17785,#17786,#17787,#17788,#17789,
#17790,#17791,#17792,#17793,#17794,#17795,#17796,#17797,#17798,#17799,#17800,
#17801,#17802,#17803,#17804,#17805,#17806,#17807,#17808,#17809,#17810,#17811,
#17812,#17813,#17814,#17815,#17816,#17817,#17818,#17819,#17820,#17821,#17822,
#17823,#17824,#17825,#17826,#17827,#17828,#17829,#17830,#17831,#17832,#17833,
#17834,#17835,#17836,#17837,#17838,#17839,#17840,#17841,#17842,#17843,#17844,
#17845,#17846,#17847,#17848,#17849,#17850,#17851,#17852,#17853,#17854,#17855,
#17856,#17857,#17858,#17859,#17860,#17861,#17862,#17863,#17864,#17865,#17866,
#17867,#17868,#17869,#17870,#17871,#17872,#17873,#17874,#17875,#17876,#17877,
#17878,#17879,#17880,#17881,#17882,#17883,#17884,#17885,#17886,#17887,#17888,
#17889,#17890,#17891,#17892,#17893,#17894,#17895,#17896,#17897,#17898,#17899,
#17900,#17901,#17902,#17903,#17904,#17905,#17906,#17907,#17908,#17909,#17910,
#17911,#17912,#17913,#17914,#17915,#17916,#17917,#17918,#17919,#17920,#17921,
#17922,#17923,#17924,#17925,#17926,#17927,#17928,#17929,#17930,#17931,#17932,
#17933,#17934,#17935,#17936,#17937,#17938,#17939,#17940,#17941,#17942,#17943,
#17944,#17945,#17946,#17947,#17948,#17949,#17950,#17951,#17952,#17953,#17954,
#17955,#17956,#17957,#17958,#17959,#17960,#17961,#17962,#17963,#17964,#17965,
#17966,#17967,#17968,#17969,#17970,#17971,#17972,#17973,#17974,#17975,#17976,
#17977,#17978,#17979,#17980,#17981,#17982,#17983,#17984,#17985,#17986,#17987,
#17988,#17989,#17990,#17991,#17992,#17993,#17994,#17995,#17996,#17997,#17998,
#17999,#18000,#18001,#18002,#18003,#18004,#18005,#18006,#18007,#18008,#18009,
#18010,#18011,#18012,#18013,#18014,#18015,#18016,#18017,#18018,#18019,#18020,
#18021,#18022,#18023,#18024,#18025,#18026,#18027,#18028,#18029,#18030,#18031,
#18032,#18033,#18034,#18035,#18036,#18037,#18038,#18039,#18040,#18041,#18042,
#18043,#18044,#18045,#18046,#18047,#18048,#18049,#18050,#18051,#18052,#18053,
#18054,#18055,#18056,#18057,#18058,#18059,#18060,#18061,#18062,#18063,#18064,
#18065,#18066,#18067,#18068,#18069,#18070,#18071,#18072,#18073,#18074,#18075,
#18076,#18077,#18078,#18079,#18080,#18081,#18082,#18083,#18084,#18085,#18086,
#18087,#18088,#18089,#18090,#18091,#18092,#18093,#18094,#18095,#18096,#18097,
#18098,#18099,#18100,#18101,#18102,#18103,#18104,#18105,#18106,#18107,#18108,
#18109,#18110,#18111,#18112,#18113,#18114,#18115,#18116,#18117,#18118,#18119,
#18120,#18121,#18122,#18123,#18124,#18125,#18126,#18127,#18128,#18129,#18130,
#18131,#18132,#18133,#18134,#18135,#18136,#18137,#18138,#18139,#18140,#18141,
#18142,#18143,#18144,#18145,#18146,#18147,#18148,#18149,#18150,#18151,#18152,
#18153,#18154,#18155,#18156,#18157,#18158,#18159,#18160,#18161,#18162,#18163,
#18164,#18165,#18166,#18167,#18168,#18169,#18170,#18171,#18172,#18173,#18174,
#18175,#18176,#18177,#18178,#18179,#18180,#18181,#18182,#18183,#18184,#18185,
#18186,#18187,#18188,#18189,#18190,#18191,#18192,#18193,#18194,#18195,#18196,
#18197,#18198,#18199,#18200,#18201,#18202,#18203,#18204,#18205,#18206,#18207,
#18208,#18209,#18210,#18211,#18212,#18213,#18214,#18215,#18216,#18217,#18218,
#18219,#18220,#18221,#18222,#18223,#18224,#18225,#18226,#18227,#18228,#18229,
#18230,#18231,#18232,#18233,#18234,#18235,#18236,#18237,#18238,#18239,#18240,
#18241,#18242,#18243,#18244,#18245,#18246,#18247,#18248,#18249,#18250,#18251,
#18252,#18253,#18254,#18255,#18256,#18257,#18258,#18259,#18260,#18261,#18262,
#18263,#18264,#18265,#18266,#18267,#18268,#18269,#18270,#18271,#18272,#18273,
#18274,#18275,#18276,#18277,#18278,#18279,#18280,#18281,#18282,#18283,#18284,
#18285,#18286,#18287,#18288,#18289,#18290,#18291,#18292,#18293,#18294,#18295,
#18296,#18297,#18298,#18299,#18300,#18301,#18302),.UNSPECIFIED.,.F.,.F.,
(4,2,2,2,2,2,2,2,2,2,2,2,2,2,2,2,2,2,2,2,2,2,2,2,2,2,2,2,2,2,2,2,2,2,2,
2,2,2,2,2,2,2,2,2,2,2,2,2,2,2,2,2,2,2,2,2,2,2,2,2,2,2,2,2,2,2,2,2,2,2,2,
2,2,2,2,2,2,2,2,2,2,2,2,2,2,2,2,2,2,2,2,2,2,2,2,2,2,2,2,2,2,2,2,2,2,2,2,
2,2,2,2,2,2,2,2,2,2,2,2,2,2,2,2,2,2,2,2,2,2,2,2,2,2,2,2,2,2,2,2,2,2,2,2,
2,2,2,2,2,2,2,2,2,2,2,2,2,2,2,2,2,2,2,2,2,2,2,2,2,2,2,2,2,2,2,2,2,2,2,2,
2,2,2,2,2,2,2,2,2,2,2,2,2,2,2,2,2,2,2,2,2,2,2,2,2,2,2,2,2,2,2,2,2,2,2,2,
2,2,2,2,2,2,2,2,2,2,2,2,2,2,2,2,2,2,2,2,2,2,2,2,2,2,2,2,2,2,2,2,2,2,2,2,
2,2,2,2,2,2,2,4),(-2.51398133414389,-2.48094175545532,-2.47168106510804,
-2.46926076959548,-2.467614212309,-2.46601368312452,-2.46455814540407,-2.46268194213675,
-2.45877502270415,-2.41991617881569,-2.39953857607119,-2.37417890363605,
-2.36845741052523,-2.366928696018,-2.36602036660579,-2.36520619840469,-2.36415585310862,
-2.36189386455443,-2.32460157946666,-2.2938197608203,-2.27934229752528,
-2.27057952874916,-2.26802678361449,-2.26642148068764,-2.26496706728765,
-2.26309995428477,-2.25923957173121,-2.22765804283565,-2.17406261966766,
-2.16893403212184,-2.16732994053434,-2.16640475970811,-2.16559379572614,
-2.16455404267801,-2.16240531666918,-2.14737899368109,-2.14144762068344,
-2.09292531544002,-2.07922365938938,-2.0708087943132,-2.06831946276363,
-2.06671666613336,-2.06526147818122,-2.0633891089575,-2.05950245858449,
-2.02601915280448,-1.97696899466405,-1.96935716017211,-1.96769038473055,
-1.96675133922251,-1.96594213101539,-1.96492257083077,-1.96294027819942,
-1.95137205100061,-1.94888585697622,-1.9262629161582,-1.89595926110847,
-1.88050481778762,-1.87128362186004,-1.86866567160033,-1.86706185467856,
-1.86560668372267,-1.86373565688326,-1.85985657030819,-1.81812693396771,
-1.78941751686676,-1.77639289024704,-1.76960934477522,-1.7680020702245,
-1.76707612572484,-1.76626518367929,-1.7652263688428,-1.76308271238347,
-1.74820159192034,-1.74181643349194,-1.72637341381769,-1.69615454481816,
-1.68080770437188,-1.6716330405734,-1.66901965959808,-1.66741680992759,
-1.66596131494738,-1.66408818780691,-1.66019864878989,-1.62630758762357,
-1.57756865760962,-1.57003235489076,-1.56837050933725,-1.56743244860871,
-1.56662297952755,-1.56560166318075,-1.56361170249996,-1.55190054996639,
-1.54932817092889,-1.52694207947948,-1.49663256533507,-1.48117464996275,
-1.47195151558511,-1.46933307986235,-1.46772897923454,-1.4662735598391,
-1.46440222611581,-1.46052254867567,-1.41878494906313,-1.38988249714859,
-1.37105324413692,-1.36897575595239,-1.36795002564225,-1.36721689675486,
-1.36642390835619,-1.36501970276723,-1.36085863534669,-1.3198402164215,
-1.27489197203946,-1.27067773545672,-1.26874244409121,-1.26727813992438,
-1.26589540141608,-1.26358485885676,-1.25753004970178,-1.22496965591972,
-1.19146752549143,-1.18668171931917,-1.17145572812837,-1.16929948115566,
-1.16825810725949,-1.16744682266727,-1.16652231652083,-1.16492184549236,
-1.15822808596142,-1.14545663805007,-1.13275059197035,-1.07758429324634,
-1.0717714755534,-1.0694988870727,-1.06812350832289,-1.06665540160461,-1.06469523726938,
-1.06034602757736,-1.05454923706921,-1.04011897833516,-0.978592954777521,
-0.971000621473652,-0.969417613263893,-0.968403624918487,-0.967594614630355,
-0.966650955466922,-0.964963866846999,-0.957049131125499,-0.940661775149694,
-0.886519352839538,-0.873540572419314,-0.870763856863685,-0.868962034808591,
-0.867513975470122,-0.865868306229021,-0.863062938440502,-0.851758961183308,
-0.799746916106645,-0.772186862548338,-0.769826244760251,-0.768757155317357,
-0.767939996180307,-0.767040785690155,-0.765554130552059,-0.760173246858827,
-0.750808700550199,-0.727291553503988,-0.678664799241963,-0.676086604778511,
-0.671634634653937,-0.669805992682046,-0.668448562896624,-0.666967512786282,
-0.664932672995948,-0.66016444508058,-0.639798857059222,-0.583519883951563,
-0.571864926345619,-0.569877615655351,-0.568856753530014,-0.568047175675012,
-0.567108451917473,-0.565444111897216,-0.557874383597566,-0.509016016821418,
-0.475301642092305,-0.471410891307572,-0.46953725809826,-0.468081403714759,
-0.466478192390659,-0.463864299432147,-0.454688686861974,-0.439338771628266,
-0.409086590448366,-0.372533950981189,-0.370253955200523,-0.369199870324798,
-0.368384832564936,-0.368383319540139,-0.368382272221675,-0.368381225017134,
-0.368380177959486,-0.368379131076913,-0.368378084328339,-0.368377037698587,
-0.368375991213697,-0.368374944861903,-0.368373898606277,-0.368372852471212,
-0.368371806486869,-0.36837076064387,-0.368369714916329,-0.368368669289933,
-0.36836762382266,-0.368366578487437,-0.368365533305993,-0.368364488214365,
-0.368363443206881,-0.368362398312207,-0.368361353537718,-0.368360308853475,
-0.368359264386209,-0.368358220053414,-0.368357175811266,-0.368356131622976,
-0.36745770110628,-0.365984347803652,-0.364179848601488,-0.360563941382592,
-0.313953809935299,-0.275587280122757,-0.271674393658817,-0.269796473049413,
-0.268340110753364,-0.266739186170573,-0.264135421636745,-0.255059780812809,
-0.239939208821071,-0.192696679347792,-0.187694572590075,-0.172574189801506,
-0.170421422503793,-0.169380625704051,-0.168569275656492,-0.167807751793634,
-0.166413642124588,-0.161945734624372,-0.154620083623877,-0.131233799457145,
-0.079072857372386,-0.0729821580967447,-0.0706658261729997,-0.069281865159288,
-0.06781792596521,-0.065885919103819,-0.061689948373313,-0.0208029638340278,
-0.00059283742129488),.UNSPECIFIED.);
#800=B_SPLINE_CURVE_WITH_KNOTS('',3,(#18304,#18305,#18306,#18307,#18308,
#18309,#18310,#18311,#18312,#18313,#18314,#18315,#18316,#18317,#18318,#18319,
#18320,#18321,#18322,#18323,#18324,#18325,#18326,#18327,#18328,#18329,#18330,
#18331,#18332,#18333,#18334,#18335,#18336,#18337,#18338,#18339,#18340,#18341,
#18342,#18343,#18344,#18345,#18346,#18347,#18348,#18349,#18350,#18351,#18352,
#18353,#18354,#18355,#18356,#18357,#18358,#18359,#18360,#18361,#18362,#18363,
#18364,#18365,#18366,#18367,#18368,#18369,#18370,#18371,#18372,#18373,#18374,
#18375,#18376,#18377,#18378,#18379,#18380,#18381,#18382,#18383,#18384,#18385,
#18386,#18387,#18388,#18389,#18390,#18391,#18392,#18393,#18394,#18395,#18396,
#18397,#18398,#18399,#18400,#18401,#18402,#18403,#18404,#18405,#18406,#18407,
#18408,#18409,#18410,#18411,#18412,#18413,#18414,#18415,#18416,#18417,#18418,
#18419,#18420,#18421,#18422,#18423,#18424,#18425,#18426,#18427,#18428,#18429,
#18430,#18431,#18432,#18433,#18434,#18435,#18436,#18437,#18438,#18439,#18440,
#18441,#18442,#18443,#18444,#18445,#18446,#18447,#18448,#18449,#18450,#18451,
#18452,#18453,#18454,#18455,#18456,#18457,#18458,#18459,#18460,#18461,#18462,
#18463,#18464,#18465,#18466,#18467,#18468,#18469,#18470,#18471,#18472,#18473,
#18474,#18475,#18476,#18477,#18478,#18479,#18480,#18481,#18482,#18483,#18484,
#18485,#18486,#18487,#18488,#18489,#18490),.UNSPECIFIED.,.F.,.F.,(4,3,3,
3,3,3,3,3,3,3,3,3,3,3,3,3,3,3,3,3,3,3,3,3,3,3,3,3,3,3,3,3,3,3,3,3,3,3,3,
3,3,3,3,3,3,3,3,3,3,3,3,3,3,3,3,3,3,3,3,3,3,3,4),(204.203522483337,204.361800790967,
204.466746605831,204.57153467083,204.676199201471,204.780797709263,204.885365778675,
204.989938950007,205.094622905074,205.199367968475,205.304295814935,205.360481659328,
205.465427474192,205.570215539191,205.674880069832,205.779478577624,205.884046647036,
205.988619818368,206.093303773436,206.198048836836,206.302976683297,206.359162527688,
206.464108342552,206.568896407551,206.673560938192,206.778159445984,206.882727515396,
206.987300686728,207.091984641796,207.196729705196,207.301657551657,207.357843396049,
207.462789210913,207.567577275912,207.672241806554,207.776840314345,207.881408383758,
207.98598155509,208.090665510158,208.195410573558,208.300338420019,208.35652426441,
208.461470079274,208.566258144273,208.670922674914,208.775521182706,208.880089252118,
208.984662423451,209.089346378518,209.194091441919,209.299019288379,209.355205132771,
209.460150947635,209.564939012634,209.669603543275,209.774202051067,209.878770120479,
209.983343291811,210.088027246879,210.192772310279,210.297700156739,210.353886001131,
210.486707790516),.UNSPECIFIED.);
#801=B_SPLINE_CURVE_WITH_KNOTS('',3,(#18492,#18493,#18494,#18495,#18496,
#18497,#18498,#18499,#18500,#18501,#18502,#18503,#18504,#18505,#18506,#18507,
#18508,#18509,#18510,#18511,#18512,#18513,#18514,#18515,#18516,#18517,#18518,
#18519,#18520,#18521,#18522,#18523,#18524,#18525,#18526,#18527,#18528,#18529,
#18530,#18531,#18532,#18533,#18534,#18535,#18536,#18537,#18538,#18539,#18540,
#18541,#18542,#18543,#18544,#18545,#18546,#18547,#18548,#18549,#18550,#18551,
#18552,#18553,#18554,#18555,#18556,#18557,#18558,#18559,#18560,#18561,#18562,
#18563,#18564,#18565,#18566,#18567,#18568,#18569,#18570,#18571,#18572,#18573,
#18574,#18575,#18576,#18577,#18578,#18579,#18580,#18581,#18582,#18583,#18584,
#18585,#18586,#18587,#18588,#18589,#18590,#18591,#18592,#18593,#18594,#18595,
#18596,#18597,#18598,#18599,#18600,#18601,#18602,#18603,#18604,#18605,#18606,
#18607,#18608,#18609,#18610,#18611,#18612,#18613,#18614,#18615,#18616,#18617,
#18618,#18619,#18620,#18621,#18622,#18623,#18624,#18625,#18626,#18627,#18628,
#18629,#18630,#18631,#18632,#18633,#18634,#18635,#18636,#18637,#18638,#18639,
#18640,#18641,#18642,#18643,#18644,#18645,#18646,#18647,#18648,#18649,#18650,
#18651,#18652,#18653,#18654,#18655,#18656,#18657,#18658,#18659,#18660,#18661,
#18662,#18663,#18664,#18665,#18666,#18667,#18668,#18669,#18670,#18671,#18672,
#18673,#18674,#18675,#18676,#18677,#18678,#18679,#18680,#18681,#18682,#18683,
#18684,#18685,#18686,#18687,#18688,#18689,#18690,#18691,#18692,#18693,#18694,
#18695,#18696,#18697,#18698,#18699,#18700,#18701,#18702,#18703,#18704,#18705,
#18706,#18707,#18708,#18709,#18710,#18711,#18712,#18713,#18714,#18715,#18716,
#18717,#18718,#18719,#18720,#18721,#18722,#18723,#18724,#18725,#18726,#18727,
#18728,#18729,#18730,#18731,#18732,#18733,#18734,#18735,#18736,#18737,#18738,
#18739,#18740,#18741,#18742,#18743,#18744,#18745,#18746,#18747,#18748,#18749,
#18750,#18751,#18752,#18753,#18754,#18755,#18756,#18757,#18758,#18759,#18760,
#18761,#18762,#18763,#18764,#18765,#18766,#18767,#18768,#18769,#18770,#18771,
#18772,#18773,#18774,#18775,#18776,#18777,#18778,#18779,#18780,#18781,#18782,
#18783,#18784,#18785,#18786,#18787,#18788,#18789,#18790,#18791,#18792,#18793,
#18794,#18795,#18796,#18797,#18798,#18799,#18800,#18801,#18802,#18803,#18804,
#18805,#18806,#18807,#18808,#18809,#18810,#18811,#18812,#18813,#18814,#18815,
#18816,#18817,#18818,#18819,#18820,#18821,#18822,#18823,#18824,#18825,#18826,
#18827,#18828,#18829,#18830,#18831,#18832,#18833,#18834,#18835,#18836,#18837,
#18838,#18839,#18840,#18841,#18842,#18843,#18844,#18845,#18846,#18847,#18848,
#18849,#18850,#18851,#18852,#18853,#18854,#18855,#18856,#18857,#18858,#18859,
#18860,#18861,#18862,#18863,#18864,#18865,#18866,#18867,#18868,#18869,#18870,
#18871,#18872,#18873,#18874,#18875,#18876,#18877,#18878,#18879,#18880,#18881,
#18882,#18883,#18884,#18885,#18886,#18887,#18888,#18889,#18890,#18891,#18892,
#18893,#18894,#18895,#18896,#18897,#18898,#18899,#18900,#18901,#18902,#18903,
#18904,#18905,#18906,#18907,#18908,#18909,#18910,#18911,#18912,#18913,#18914,
#18915,#18916,#18917,#18918,#18919,#18920,#18921,#18922,#18923,#18924,#18925,
#18926,#18927,#18928,#18929,#18930,#18931,#18932,#18933,#18934,#18935,#18936,
#18937,#18938,#18939,#18940,#18941,#18942,#18943,#18944,#18945,#18946,#18947,
#18948,#18949,#18950,#18951,#18952,#18953,#18954,#18955,#18956,#18957,#18958,
#18959,#18960,#18961),.UNSPECIFIED.,.F.,.F.,(4,2,2,2,2,2,2,2,2,2,2,2,2,
2,2,2,2,2,2,2,2,2,2,2,2,2,2,2,2,2,2,2,2,2,2,2,2,2,2,2,2,2,2,2,2,2,2,2,2,
2,2,2,2,2,2,2,2,2,2,2,2,2,2,2,2,2,2,2,2,2,2,2,2,2,2,2,2,2,2,2,2,2,2,2,2,
2,2,2,2,2,2,2,2,2,2,2,2,2,2,2,2,2,2,2,2,2,2,2,2,2,2,2,2,2,2,2,2,2,2,2,2,
2,2,2,2,2,2,2,2,2,2,2,2,2,2,2,2,2,2,2,2,2,2,2,2,2,2,2,2,2,2,2,2,2,2,2,2,
2,2,2,2,2,2,2,2,2,2,2,2,2,2,2,2,2,2,2,2,2,2,2,2,2,2,2,2,2,2,2,2,2,2,2,2,
2,2,2,2,2,2,2,2,2,2,2,2,2,2,2,2,2,2,2,2,2,2,2,2,2,2,2,2,2,2,2,2,2,2,2,2,
2,2,2,2,2,4),(-2.51398629788239,-2.46795087027503,-2.45375792511426,-2.44802915902984,
-2.44372066163785,-2.44176833910706,-2.4403018443564,-2.4389248649769,-2.43664237175022,
-2.43076455586678,-2.37620732677608,-2.35512773261379,-2.34767501984731,
-2.34314505555221,-2.34174758160813,-2.34098617084092,-2.34017543526592,
-2.33913733429327,-2.33747475214223,-2.32867022671071,-2.29639307256834,
-2.27006620876583,-2.25472359085531,-2.24555126402546,-2.24293845690623,
-2.24133593971715,-2.23988073387095,-2.23800796090869,-2.2341190923721,
-2.20044650173763,-2.14899255054784,-2.14543282438832,-2.14364879179028,
-2.14221717507587,-2.14131504662893,-2.14050325883575,-2.13945604594684,
-2.13726952002486,-2.12112379858218,-2.11383712146277,-2.07301062995499,
-2.04741343427391,-2.04392878158255,-2.04213721919746,-2.04070351937282,
-2.03905594847783,-2.03624103787606,-2.02622526019384,-2.02422571609486,
-1.96229465709312,-1.95042955722146,-1.94621591151312,-1.94326177926346,
-1.94207804158348,-1.94124441069749,-1.94048395585791,-1.93944539085576,
-1.93738890901078,-1.90102604353356,-1.8707498351434,-1.85533307661067,
-1.84612785235754,-1.84351125960014,-1.84190760244773,-1.84045213619855,
-1.83858011333105,-1.83469673224155,-1.8015428631071,-1.74982927243646,
-1.74421850177414,-1.74270998574529,-1.74180588608246,-1.74099011554124,
-1.73993057960137,-1.73815926555082,-1.72735498866087,-1.70439004597293,
-1.67305654960071,-1.65629095477371,-1.64651143199589,-1.64383890037829,
-1.64222263885693,-1.64076968816644,-1.63892014226971,-1.63515145912288,
-1.58790912082465,-1.56059992226594,-1.55029203425454,-1.54452954770775,
-1.5430070281963,-1.54209976539471,-1.54128475449979,-1.54023095940987,
-1.53795254811452,-1.50134976579041,-1.47114503159617,-1.45582242719179,
-1.44665756377709,-1.44404467412986,-1.44244163736467,-1.4409856518575,
-1.43911144379228,-1.43521802906191,-1.40130362551224,-1.35256430487385,
-1.34502941999764,-1.34336733830977,-1.34242905943818,-1.34161934954842,
-1.34059766170652,-1.33860677522959,-1.32688557014606,-1.2754546390385,
-1.25738389272865,-1.24726459093063,-1.24447149821661,-1.24281226010264,
-1.24136531117254,-1.239581695986,-1.2361375512184,-1.21201628512939,-1.18120307382977,
-1.14632193050641,-1.14401154815011,-1.14295170194368,-1.14213579848125,
-1.14123165945308,-1.13972332033393,-1.13411584544945,-1.08241697174498,
-1.04926714359544,-1.04538330725497,-1.04351098147952,-1.04205524187987,
-1.04045124517652,-1.03783401235416,-1.02862572017281,-1.01320069702563,
-0.982887796839183,-0.957295450767591,-0.946065469682763,-0.94427328013483,
-0.943207602619392,-0.942390908167608,-0.941489893791444,-0.93999533270989,
-0.934533003263245,-0.887610383266269,-0.849571398535599,-0.845659993460124,
-0.843782354890947,-0.842326021382814,-0.840724937130614,-0.838120483254904,
-0.829038137833757,-0.813902253134339,-0.783822569963408,-0.746760700981982,
-0.744489072019817,-0.74343658076552,-0.742621776878917,-0.741713858657482,
-0.740188306727009,-0.734391777268359,-0.723999242427689,-0.696448676037504,
-0.649637519628826,-0.645857546669602,-0.644005798882366,-0.642552643705676,
-0.640937727852791,-0.638271064914987,-0.628553074240353,-0.611931652762077,
-0.580682067616873,-0.559228155728193,-0.556701905803012,-0.546514272292528,
-0.544774254392505,-0.543723952193214,-0.542909480711512,-0.542000435784042,
-0.540469695156486,-0.534614694140527,-0.524073647573948,-0.495787577525803,
-0.449980564436194,-0.446172688183363,-0.444315464396133,-0.442861733823497,
-0.441250000783348,-0.438662442267103,-0.435576713547999,-0.429546323112597,
-0.414289137702652,-0.369351229931412,-0.347390861158746,-0.345105559693886,
-0.344034282753848,-0.34321680111517,-0.342318685981859,-0.340836900981359,
-0.335617083853237,-0.326596388419606,-0.304521875158874,-0.265846398271644,
-0.264246566349837,-0.249331186080131,-0.246425209104387,-0.244583521476723,
-0.243131510861447,-0.24151085964431,-0.238959994599779,-0.229897518825946,
-0.214743514231785,-0.187954762381855,-0.150423878930759,-0.146171892594143,
-0.144755803688894,-0.143960391515718,-0.143227884822282,-0.142207334824263,
-0.14015576801684,-0.126838923942786,-0.105241763439404,-0.0849281950929156,
-0.0507288998778756,-0.0468327651080157,-0.044958088681128,-0.0435021124828918,
-0.0418994628204193,-0.0402501591703931,-0.0378240400501954,-0.028648503744147,
-0.000592063665398865),.UNSPECIFIED.);
#802=B_SPLINE_CURVE_WITH_KNOTS('',3,(#18963,#18964,#18965,#18966,#18967,
#18968,#18969,#18970,#18971,#18972,#18973,#18974,#18975,#18976,#18977,#18978,
#18979,#18980,#18981,#18982,#18983,#18984,#18985,#18986,#18987,#18988,#18989,
#18990,#18991,#18992,#18993,#18994,#18995,#18996,#18997,#18998,#18999,#19000,
#19001,#19002,#19003,#19004,#19005,#19006,#19007,#19008,#19009,#19010,#19011,
#19012,#19013,#19014,#19015,#19016,#19017,#19018,#19019,#19020,#19021,#19022,
#19023,#19024,#19025,#19026,#19027,#19028,#19029,#19030,#19031,#19032,#19033,
#19034,#19035,#19036,#19037,#19038,#19039,#19040,#19041,#19042,#19043,#19044,
#19045,#19046,#19047,#19048,#19049,#19050,#19051,#19052,#19053,#19054,#19055,
#19056,#19057,#19058,#19059,#19060,#19061,#19062,#19063,#19064,#19065,#19066,
#19067,#19068,#19069,#19070,#19071,#19072,#19073,#19074,#19075,#19076,#19077,
#19078,#19079,#19080,#19081,#19082,#19083,#19084,#19085,#19086,#19087,#19088,
#19089,#19090,#19091,#19092,#19093,#19094,#19095,#19096,#19097,#19098,#19099,
#19100,#19101,#19102,#19103,#19104,#19105,#19106,#19107,#19108,#19109,#19110,
#19111,#19112,#19113,#19114,#19115,#19116,#19117,#19118,#19119,#19120,#19121,
#19122,#19123,#19124,#19125,#19126,#19127,#19128,#19129,#19130,#19131,#19132,
#19133,#19134,#19135,#19136,#19137,#19138,#19139,#19140,#19141,#19142,#19143,
#19144,#19145,#19146,#19147,#19148,#19149,#19150,#19151,#19152,#19153,#19154,
#19155,#19156,#19157,#19158,#19159,#19160,#19161,#19162,#19163,#19164,#19165,
#19166,#19167,#19168,#19169,#19170,#19171,#19172,#19173,#19174,#19175,#19176,
#19177,#19178,#19179,#19180,#19181,#19182,#19183,#19184,#19185,#19186,#19187,
#19188,#19189,#19190,#19191,#19192,#19193,#19194,#19195,#19196,#19197,#19198,
#19199,#19200,#19201,#19202,#19203,#19204,#19205,#19206,#19207,#19208,#19209,
#19210,#19211,#19212,#19213,#19214,#19215,#19216,#19217,#19218,#19219,#19220,
#19221,#19222,#19223,#19224,#19225,#19226,#19227,#19228,#19229,#19230,#19231,
#19232,#19233,#19234,#19235,#19236,#19237,#19238,#19239,#19240,#19241,#19242,
#19243,#19244,#19245,#19246,#19247,#19248,#19249,#19250,#19251,#19252,#19253,
#19254,#19255,#19256,#19257,#19258,#19259,#19260,#19261,#19262,#19263,#19264,
#19265,#19266,#19267,#19268,#19269,#19270,#19271,#19272,#19273,#19274,#19275,
#19276,#19277,#19278,#19279,#19280,#19281,#19282,#19283,#19284,#19285,#19286,
#19287,#19288,#19289,#19290,#19291,#19292,#19293,#19294,#19295,#19296,#19297,
#19298,#19299,#19300,#19301,#19302,#19303,#19304,#19305,#19306,#19307,#19308,
#19309,#19310,#19311,#19312,#19313,#19314,#19315,#19316,#19317,#19318,#19319,
#19320,#19321,#19322,#19323,#19324,#19325,#19326,#19327,#19328,#19329,#19330,
#19331,#19332,#19333,#19334,#19335,#19336,#19337,#19338,#19339,#19340,#19341,
#19342,#19343,#19344,#19345,#19346,#19347,#19348,#19349,#19350,#19351,#19352,
#19353,#19354,#19355,#19356,#19357,#19358,#19359,#19360,#19361,#19362,#19363,
#19364,#19365,#19366,#19367,#19368,#19369,#19370,#19371,#19372,#19373,#19374,
#19375,#19376,#19377,#19378,#19379,#19380,#19381,#19382,#19383,#19384,#19385,
#19386,#19387,#19388,#19389,#19390,#19391,#19392,#19393,#19394,#19395,#19396,
#19397,#19398,#19399,#19400,#19401,#19402,#19403,#19404,#19405,#19406,#19407,
#19408,#19409,#19410,#19411,#19412,#19413,#19414,#19415,#19416,#19417,#19418,
#19419,#19420,#19421,#19422,#19423,#19424,#19425,#19426,#19427,#19428,#19429,
#19430,#19431,#19432,#19433,#19434,#19435,#19436,#19437,#19438,#19439,#19440,
#19441,#19442,#19443,#19444),.UNSPECIFIED.,.F.,.F.,(4,2,2,2,2,2,2,2,2,2,
2,2,2,2,2,2,2,2,2,2,2,2,2,2,2,2,2,2,2,2,2,2,2,2,2,2,2,2,2,2,2,2,2,2,2,2,
2,2,2,2,2,2,2,2,2,2,2,2,2,2,2,2,2,2,2,2,2,2,2,2,2,2,2,2,2,2,2,2,2,2,2,2,
2,2,2,2,2,2,2,2,2,2,2,2,2,2,2,2,2,2,2,2,2,2,2,2,2,2,2,2,2,2,2,2,2,2,2,2,
2,2,2,2,2,2,2,2,2,2,2,2,2,2,2,2,2,2,2,2,2,2,2,2,2,2,2,2,2,2,2,2,2,2,2,2,
2,2,2,2,2,2,2,2,2,2,2,2,2,2,2,2,2,2,2,2,2,2,2,2,2,2,2,2,2,2,2,2,2,2,2,2,
2,2,2,2,2,2,2,2,2,2,2,2,2,2,2,2,2,2,2,2,2,2,2,2,2,2,2,2,2,2,2,2,2,2,2,2,
2,2,2,2,2,2,2,2,2,2,2,2,2,2,4),(-2.51309486647585,-2.46452588930045,-2.46094116663356,
-2.45914826323717,-2.4576494174572,-2.4567478098884,-2.45593197253983,-2.45486927608813,
-2.453086102597,-2.4420255352352,-2.43843277892963,-2.43111971628948,-2.405392421698,
-2.38767560925038,-2.36508982731207,-2.36024618075138,-2.35864528251184,
-2.35728744241274,-2.35583828260136,-2.35401780075283,-2.35117926008268,
-2.33730556066251,-2.334453758959,-2.32625480943977,-2.29801301078951,-2.2744626637411,
-2.26500393823296,-2.25960626366736,-2.25810574279304,-2.25720374812444,
-2.25638799578237,-2.25532598790854,-2.25354520754058,-2.24253428624706,
-2.22097714946139,-2.18292362379156,-2.16980775565783,-2.16439254806274,
-2.16031387905904,-2.15840633487012,-2.15694081271484,-2.1555622038298,
-2.15327103465229,-2.1473369659475,-2.14591981266485,-2.14438456107695,
-2.08057895573882,-2.06709187948396,-2.06016038206725,-2.05853246833197,
-2.05760202894418,-2.05679186086151,-2.05576019222634,-2.054118872483,-2.04566050926726,
-1.98635478540625,-1.97116324576591,-1.96205681197062,-1.95945073368042,
-1.95784977531602,-1.95639429613266,-1.95451879930779,-1.95061564964523,
-1.9122884712373,-1.86562962491964,-1.86018177766145,-1.85868902080573,
-1.85778865759155,-1.85697224120178,-1.85590651960106,-1.85411338303643,
-1.84285209157823,-1.81731873832905,-1.78704944468702,-1.77163613179805,
-1.76243298576702,-1.75981699392366,-1.75821370721278,-1.75675857858477,
-1.7548869919427,-1.75100452292647,-1.71785927177196,-1.66615802778751,
-1.66054743981812,-1.65903916937886,-1.65813525603069,-1.65731968091199,
-1.65626043488747,-1.6539520179117,-1.61902442816531,-1.5882746936776,-1.57225488523342,
-1.56279070335583,-1.56014875015394,-1.55853954252568,-1.55708553295307,
-1.5552244118891,-1.55139597138592,-1.54758985539059,-1.50318070305179,
-1.476648339805,-1.46656096278245,-1.46088681024162,-1.45937260904248,-1.45846734449927,
-1.45765207990477,-1.45659525603037,-1.45429992149832,-1.41862252411368,
-1.38812023390852,-1.37241671979743,-1.36308782632622,-1.36045903942732,
-1.35885271605285,-1.35739796783441,-1.35553124698121,-1.35167462769991,
-1.3204085977723,-1.27007144186592,-1.26156056395693,-1.25983660101191,
-1.25888492787562,-1.25807657615387,-1.25707290305206,-1.25510375362371,
-1.24079202067717,-1.21609063419052,-1.16915613609416,-1.16279362666882,
-1.16043543835808,-1.15904342312763,-1.15758332852073,-1.15567692560501,
-1.1516158636112,-1.11588193122916,-1.07805959045072,-1.0625660108618,-1.06040029108135,
-1.05935701981257,-1.05854550079585,-1.05762210306724,-1.05602676657596,
-1.04939948221175,-1.03681228632728,-0.99747920820392,-0.965762754836832,
-0.96189920898257,-0.960031037518745,-0.958576010118798,-0.956970243233074,
-0.9543443313374,-0.945046024365567,-0.929411703607346,-0.898935442968246,
-0.863069605757695,-0.861003928934717,-0.859963008211846,-0.859201916306653,
-0.858368770369099,-0.857187762410253,-0.854250818055072,-0.815658168617676,
-0.769761600799003,-0.763559876006967,-0.761108077076767,-0.75969763367226,
-0.758389399258267,-0.756605539491975,-0.753159061395943,-0.72893837933841,
-0.6980750608891,-0.663372750675305,-0.661060458493613,-0.66000039729537,
-0.65918461428771,-0.658280921010864,-0.656773995080385,-0.651179249914653,
-0.599488007319517,-0.593077098673279,-0.566173045694003,-0.562399896453556,
-0.560549652098457,-0.559096835471611,-0.557481427861126,-0.554811942654126,
-0.545061626370288,-0.528362147765403,-0.468629265392385,-0.464876122725742,
-0.461714294190704,-0.460460154051417,-0.459696633159729,-0.458865475647186,
-0.457695213919508,-0.454824521605239,-0.450763715170569,-0.439517832063242,
-0.387719494778871,-0.385273888980008,-0.378997049002927,-0.365329186619738,
-0.362503240472882,-0.360686132528895,-0.359236618089068,-0.357633641330818,
-0.35499843718957,-0.351827658283479,-0.345566581213642,-0.329474825495522,
-0.294574901946369,-0.263910933857402,-0.261556569363376,-0.260488630919481,
-0.25967163669215,-0.258771830705841,-0.257282562398658,-0.251874872386638,
-0.24244542573165,-0.217008085240243,-0.18719000997461,-0.184706759178928,
-0.180765860424814,-0.165809038263223,-0.162900401956594,-0.161057853269173,
-0.159605686019269,-0.158248603253918,-0.156659059434375,-0.151938552659457,
-0.130901286092268,-0.11320563896908,-0.066909887167199,-0.0626285276468794,
-0.0612084644784653,-0.0604122096964392,-0.0596798623458036,-0.0586609273637555,
-0.0566175285972577,-0.0539782932526428,-0.000592842301724799),
 .UNSPECIFIED.);
#803=B_SPLINE_CURVE_WITH_KNOTS('',3,(#19446,#19447,#19448,#19449,#19450,
#19451,#19452,#19453,#19454,#19455,#19456,#19457,#19458,#19459,#19460,#19461,
#19462,#19463,#19464,#19465,#19466,#19467,#19468,#19469,#19470,#19471,#19472,
#19473,#19474,#19475,#19476,#19477,#19478,#19479,#19480,#19481,#19482,#19483,
#19484,#19485,#19486,#19487,#19488,#19489,#19490,#19491,#19492,#19493,#19494,
#19495,#19496,#19497,#19498,#19499,#19500,#19501,#19502,#19503,#19504,#19505,
#19506,#19507,#19508,#19509,#19510,#19511,#19512,#19513,#19514,#19515,#19516,
#19517,#19518,#19519,#19520,#19521,#19522,#19523,#19524,#19525,#19526,#19527,
#19528,#19529,#19530,#19531,#19532,#19533,#19534,#19535,#19536,#19537,#19538,
#19539,#19540,#19541,#19542,#19543,#19544,#19545,#19546,#19547,#19548,#19549,
#19550,#19551,#19552,#19553,#19554,#19555,#19556,#19557,#19558,#19559,#19560,
#19561,#19562,#19563,#19564,#19565,#19566,#19567,#19568,#19569,#19570,#19571,
#19572,#19573,#19574,#19575,#19576,#19577,#19578,#19579,#19580,#19581,#19582,
#19583,#19584,#19585,#19586,#19587,#19588,#19589,#19590,#19591,#19592,#19593,
#19594,#19595,#19596,#19597,#19598,#19599,#19600,#19601,#19602,#19603,#19604,
#19605,#19606,#19607,#19608,#19609,#19610,#19611,#19612,#19613,#19614,#19615,
#19616,#19617,#19618,#19619,#19620,#19621,#19622,#19623,#19624,#19625,#19626,
#19627,#19628,#19629,#19630,#19631,#19632,#19633,#19634,#19635),
 .UNSPECIFIED.,.F.,.F.,(4,3,3,3,3,3,3,3,3,3,3,3,3,3,3,3,3,3,3,3,3,3,3,3,
3,3,3,3,3,3,3,3,3,3,3,3,3,3,3,3,3,3,3,3,3,3,3,3,3,3,3,3,3,3,3,3,3,3,3,3,
3,3,3,4),(235.619449019234,235.723424947678,235.82736120438,235.93129418189,
236.035333686848,236.139428244564,236.243714282079,236.319588578511,236.42453468062,
236.529323029562,236.63398783797,236.738586619568,236.843154958456,236.947728394564,
237.052412605536,237.157157920198,237.262086008044,237.318269446872,237.423216296437,
237.528005403782,237.632670982987,237.737270542601,237.841839665513,237.946413890446,
238.051098892008,238.155844999439,238.26077387488,238.316950315232,238.421892950261,
238.52667783165,238.631339188293,238.735934529757,238.840499445106,238.945069479249,
239.049750344019,239.154492339076,239.259417184133,239.315631183593,239.420579802777,
239.525370652109,239.630037924636,239.734639146622,239.839209898787,239.943785717648,
240.048472249213,240.153219852705,240.258150155706,240.314312051954,240.419263637437,
240.524057528087,240.628727937091,240.733332352526,240.837906349875,240.942485460475,
241.047175330889,241.151926304909,241.256859991014,241.312992920315,241.419748621657,
241.526327456451,241.63273345532,241.739038016702,241.845270670712,241.902634326414),
 .UNSPECIFIED.);
#804=B_SPLINE_CURVE_WITH_KNOTS('',3,(#19637,#19638,#19639,#19640,#19641,
#19642,#19643,#19644,#19645,#19646,#19647,#19648,#19649,#19650,#19651,#19652,
#19653,#19654,#19655,#19656,#19657,#19658,#19659,#19660,#19661,#19662,#19663,
#19664,#19665,#19666,#19667,#19668,#19669,#19670,#19671,#19672,#19673,#19674,
#19675,#19676,#19677,#19678,#19679,#19680,#19681,#19682,#19683,#19684,#19685,
#19686,#19687,#19688,#19689,#19690,#19691,#19692,#19693,#19694,#19695,#19696,
#19697,#19698,#19699,#19700,#19701,#19702,#19703,#19704,#19705,#19706,#19707,
#19708,#19709,#19710,#19711,#19712,#19713,#19714,#19715,#19716,#19717,#19718,
#19719,#19720,#19721,#19722,#19723,#19724,#19725,#19726,#19727,#19728,#19729,
#19730,#19731,#19732,#19733,#19734,#19735,#19736,#19737,#19738,#19739,#19740,
#19741,#19742,#19743,#19744,#19745,#19746,#19747,#19748,#19749,#19750,#19751,
#19752,#19753,#19754,#19755,#19756,#19757,#19758,#19759,#19760,#19761,#19762,
#19763,#19764,#19765,#19766,#19767,#19768,#19769,#19770,#19771,#19772,#19773,
#19774,#19775,#19776,#19777,#19778,#19779,#19780,#19781,#19782,#19783,#19784,
#19785,#19786,#19787,#19788,#19789,#19790,#19791,#19792,#19793,#19794,#19795,
#19796),.UNSPECIFIED.,.F.,.F.,(4,3,3,3,3,3,3,3,3,3,3,3,3,3,3,3,3,3,3,3,
3,3,3,3,3,3,3,3,3,3,3,3,3,3,3,3,3,3,3,3,3,3,3,3,3,3,3,3,3,3,3,3,3,4),(241.902634326753,
242.017552757131,242.132857082377,242.248701473426,242.311673788675,242.416644276006,
242.521456897853,242.626145699382,242.730768288196,242.83536021486,242.939956985551,
243.044663990786,243.149431827377,243.254381774431,243.310354657036,243.415329956237,
243.520147893875,243.624842722105,243.729471772774,243.834070582838,243.938674645314,
244.043389504012,244.148165524066,244.253124075436,244.309035525397,244.413831203907,
244.518468768063,244.622982970788,244.727431334325,244.831849657905,244.93627369689,
245.040810459789,245.14540920448,245.250193661039,245.307716393758,245.41286648623,
245.517858182872,245.622724415093,245.727523312383,245.832290166372,245.937060222967,
246.041936850911,246.146872475353,246.251985582833,246.306397262118,246.410386347413,
246.514201221025,246.617918810421,246.721576030725,246.825209715847,246.928926859748,
247.032682017607,247.136621574968,247.235465738518),.UNSPECIFIED.);
#805=B_SPLINE_CURVE_WITH_KNOTS('',3,(#19800,#19801,#19802,#19803,#19804,
#19805,#19806,#19807,#19808,#19809,#19810,#19811,#19812,#19813,#19814,#19815,
#19816,#19817,#19818,#19819,#19820,#19821,#19822,#19823,#19824,#19825,#19826,
#19827,#19828,#19829,#19830,#19831,#19832,#19833,#19834,#19835,#19836,#19837,
#19838,#19839,#19840,#19841,#19842,#19843,#19844,#19845,#19846,#19847,#19848,
#19849,#19850,#19851,#19852,#19853,#19854,#19855,#19856,#19857,#19858,#19859,
#19860,#19861,#19862,#19863,#19864,#19865,#19866,#19867,#19868,#19869,#19870,
#19871,#19872,#19873,#19874,#19875,#19876,#19877,#19878,#19879,#19880,#19881,
#19882,#19883,#19884,#19885,#19886,#19887,#19888,#19889,#19890,#19891,#19892,
#19893,#19894,#19895,#19896,#19897,#19898,#19899,#19900,#19901,#19902,#19903,
#19904,#19905,#19906,#19907,#19908,#19909,#19910,#19911,#19912,#19913,#19914,
#19915,#19916,#19917,#19918,#19919,#19920,#19921,#19922,#19923),
 .UNSPECIFIED.,.F.,.F.,(4,3,3,3,3,3,3,3,3,3,3,3,3,3,3,3,3,3,3,3,3,3,3,3,
3,3,3,3,3,3,3,3,3,3,3,3,3,3,3,3,3,4),(241.902634326414,241.999480923579,
242.104630987599,242.20962265607,242.314488860666,242.419287730683,242.524054557789,
242.628824587929,242.733701190235,242.838636789468,242.943749872662,242.99816179194,
243.103254328513,243.208191752163,243.313008759831,243.417761577378,243.522485535044,
243.627215920643,243.7320579726,243.836961863511,243.942047941096,243.9968426603,
244.100644682838,244.204288219948,244.307812192971,244.411272931668,244.514707444671,
244.618152699577,244.721724761877,244.825365012194,244.929211277103,244.995523528661,
245.103416970472,245.214765398791,245.322299074973,245.429730709313,245.537089219953,
245.644403430638,245.751731684544,245.859066936612,245.966474699844,245.994204397022),
 .UNSPECIFIED.);
#806=B_SPLINE_CURVE_WITH_KNOTS('',3,(#19925,#19926,#19927,#19928,#19929,
#19930,#19931,#19932,#19933,#19934,#19935,#19936,#19937,#19938,#19939,#19940,
#19941,#19942,#19943,#19944,#19945,#19946,#19947,#19948,#19949,#19950,#19951,
#19952,#19953,#19954,#19955,#19956,#19957,#19958,#19959,#19960,#19961,#19962,
#19963,#19964,#19965,#19966,#19967,#19968,#19969,#19970,#19971,#19972,#19973,
#19974,#19975,#19976,#19977,#19978,#19979,#19980,#19981,#19982,#19983,#19984,
#19985,#19986,#19987,#19988,#19989,#19990,#19991,#19992,#19993,#19994,#19995,
#19996,#19997,#19998,#19999,#20000,#20001,#20002,#20003,#20004,#20005,#20006,
#20007,#20008,#20009,#20010,#20011,#20012,#20013,#20014,#20015,#20016,#20017,
#20018,#20019,#20020,#20021,#20022,#20023,#20024,#20025,#20026,#20027,#20028,
#20029,#20030,#20031,#20032,#20033,#20034,#20035,#20036,#20037,#20038,#20039,
#20040,#20041,#20042,#20043,#20044,#20045,#20046,#20047,#20048,#20049,#20050,
#20051,#20052,#20053,#20054,#20055,#20056,#20057,#20058,#20059,#20060,#20061,
#20062,#20063,#20064,#20065,#20066,#20067,#20068,#20069,#20070,#20071,#20072,
#20073,#20074,#20075,#20076,#20077,#20078,#20079,#20080,#20081,#20082,#20083,
#20084,#20085,#20086,#20087,#20088,#20089,#20090,#20091,#20092,#20093,#20094,
#20095,#20096,#20097,#20098,#20099,#20100,#20101,#20102,#20103,#20104,#20105,
#20106,#20107,#20108,#20109,#20110,#20111,#20112,#20113,#20114),
 .UNSPECIFIED.,.F.,.F.,(4,3,3,3,3,3,3,3,3,3,3,3,3,3,3,3,3,3,3,3,3,3,3,3,
3,3,3,3,3,3,3,3,3,3,3,3,3,3,3,3,3,3,3,3,3,3,3,3,3,3,3,3,3,3,3,3,3,3,3,3,
3,3,3,4),(235.619449019605,235.736021958153,235.853076834015,235.970735614475,
236.007395713414,236.112344331345,236.217135179442,236.321802450764,236.426403671564,
236.530974422564,236.635550240284,236.740236770748,236.844984373159,236.949914675127,
237.006076581775,237.111028161415,237.21582204618,237.320492449269,237.425096858772,
237.529670850182,237.634249954846,237.738939819366,237.843690787507,237.948624467821,
238.004757450136,238.109681185845,238.214447131041,238.319089587424,238.423666061042,
238.528212168383,238.632763481826,238.737425885531,238.842149538951,238.947056424382,
239.003438318497,239.108408798266,239.213221412623,239.317910206801,239.422532788354,
239.527124707856,239.631721471494,239.736428469887,239.841196299746,239.946146240309,
240.002119186857,240.107094458936,240.211912369256,240.316607170012,240.421236193124,
240.525834975592,240.630439010474,240.735153841768,240.839929834487,240.944888358919,
241.000800055218,241.104319830401,241.207661617074,241.310904203503,241.414085012755,
241.517241378582,241.620474637911,241.723746229367,241.827185633363,241.902634326145),
 .UNSPECIFIED.);
#807=B_SPLINE_CURVE_WITH_KNOTS('',3,(#20116,#20117,#20118,#20119,#20120,
#20121,#20122,#20123,#20124,#20125,#20126,#20127,#20128,#20129,#20130,#20131,
#20132,#20133,#20134,#20135,#20136,#20137,#20138,#20139,#20140,#20141,#20142,
#20143,#20144,#20145,#20146,#20147,#20148,#20149,#20150,#20151,#20152,#20153,
#20154,#20155,#20156,#20157,#20158,#20159,#20160,#20161,#20162,#20163,#20164,
#20165,#20166,#20167,#20168,#20169,#20170,#20171,#20172,#20173,#20174,#20175,
#20176,#20177,#20178,#20179,#20180,#20181,#20182,#20183,#20184,#20185,#20186,
#20187,#20188,#20189,#20190,#20191,#20192,#20193,#20194,#20195,#20196,#20197,
#20198,#20199,#20200,#20201,#20202,#20203,#20204,#20205,#20206,#20207,#20208,
#20209,#20210,#20211,#20212,#20213,#20214,#20215,#20216,#20217,#20218,#20219,
#20220,#20221,#20222,#20223,#20224,#20225,#20226,#20227,#20228,#20229,#20230,
#20231,#20232,#20233,#20234,#20235,#20236,#20237,#20238,#20239,#20240,#20241,
#20242,#20243,#20244,#20245,#20246,#20247,#20248,#20249,#20250,#20251,#20252,
#20253,#20254,#20255,#20256,#20257,#20258,#20259,#20260,#20261,#20262,#20263,
#20264,#20265,#20266,#20267,#20268,#20269,#20270,#20271,#20272,#20273,#20274,
#20275,#20276,#20277,#20278,#20279,#20280,#20281,#20282,#20283,#20284,#20285,
#20286,#20287,#20288,#20289,#20290,#20291,#20292,#20293,#20294,#20295,#20296,
#20297,#20298,#20299,#20300,#20301,#20302,#20303,#20304,#20305,#20306,#20307,
#20308,#20309,#20310,#20311,#20312,#20313,#20314,#20315,#20316,#20317,#20318,
#20319,#20320,#20321,#20322,#20323,#20324,#20325,#20326,#20327,#20328,#20329,
#20330,#20331,#20332,#20333,#20334,#20335,#20336,#20337,#20338,#20339,#20340,
#20341,#20342,#20343,#20344,#20345,#20346,#20347,#20348,#20349,#20350,#20351,
#20352,#20353,#20354,#20355,#20356,#20357,#20358,#20359,#20360,#20361,#20362,
#20363,#20364,#20365,#20366,#20367,#20368,#20369,#20370,#20371,#20372,#20373,
#20374,#20375,#20376,#20377,#20378,#20379,#20380,#20381,#20382,#20383,#20384,
#20385,#20386,#20387,#20388,#20389,#20390,#20391,#20392,#20393,#20394,#20395,
#20396,#20397,#20398,#20399,#20400,#20401,#20402,#20403,#20404,#20405,#20406,
#20407,#20408,#20409,#20410,#20411,#20412,#20413,#20414,#20415,#20416,#20417,
#20418,#20419,#20420,#20421,#20422,#20423,#20424,#20425,#20426,#20427,#20428,
#20429,#20430,#20431,#20432,#20433,#20434,#20435,#20436,#20437,#20438,#20439,
#20440,#20441,#20442,#20443,#20444,#20445,#20446,#20447,#20448,#20449,#20450,
#20451,#20452,#20453,#20454,#20455,#20456,#20457,#20458,#20459,#20460,#20461,
#20462,#20463,#20464,#20465,#20466,#20467,#20468,#20469,#20470,#20471,#20472,
#20473,#20474,#20475,#20476,#20477,#20478,#20479,#20480,#20481,#20482,#20483,
#20484,#20485,#20486,#20487,#20488,#20489,#20490,#20491,#20492,#20493,#20494,
#20495,#20496,#20497,#20498,#20499,#20500,#20501,#20502,#20503,#20504,#20505,
#20506,#20507,#20508,#20509,#20510,#20511,#20512,#20513,#20514,#20515,#20516,
#20517,#20518,#20519,#20520,#20521,#20522,#20523,#20524,#20525,#20526,#20527,
#20528,#20529,#20530,#20531,#20532,#20533,#20534,#20535,#20536,#20537,#20538,
#20539,#20540,#20541,#20542,#20543,#20544,#20545,#20546,#20547,#20548,#20549,
#20550,#20551,#20552,#20553,#20554,#20555,#20556,#20557,#20558,#20559,#20560,
#20561,#20562,#20563,#20564,#20565,#20566,#20567,#20568,#20569,#20570,#20571,
#20572,#20573,#20574,#20575,#20576,#20577,#20578,#20579,#20580,#20581,#20582,
#20583,#20584,#20585,#20586,#20587,#20588,#20589,#20590,#20591,#20592,#20593,
#20594,#20595,#20596,#20597,#20598,#20599,#20600,#20601,#20602,#20603,#20604,
#20605,#20606,#20607,#20608,#20609,#20610,#20611,#20612,#20613,#20614,#20615,
#20616,#20617,#20618,#20619,#20620,#20621,#20622,#20623,#20624,#20625,#20626,
#20627,#20628,#20629,#20630,#20631,#20632,#20633,#20634,#20635,#20636,#20637,
#20638,#20639,#20640,#20641,#20642,#20643,#20644,#20645,#20646,#20647,#20648,
#20649,#20650,#20651,#20652,#20653,#20654,#20655,#20656,#20657,#20658,#20659,
#20660,#20661,#20662,#20663,#20664,#20665,#20666,#20667,#20668,#20669,#20670,
#20671,#20672,#20673,#20674,#20675,#20676,#20677,#20678,#20679,#20680,#20681,
#20682,#20683,#20684,#20685,#20686,#20687,#20688,#20689,#20690,#20691,#20692,
#20693,#20694,#20695,#20696,#20697,#20698,#20699,#20700,#20701,#20702,#20703,
#20704,#20705,#20706,#20707),.UNSPECIFIED.,.F.,.F.,(4,2,2,2,2,2,2,2,2,2,
2,2,2,2,2,2,2,2,2,2,2,2,2,2,2,2,2,2,2,2,2,2,2,2,2,2,2,2,2,2,2,2,2,2,2,2,
2,2,2,2,2,2,2,2,2,2,2,2,2,2,2,2,2,2,2,2,2,2,2,2,2,2,2,2,2,2,2,2,2,2,2,2,
2,2,2,2,2,2,2,2,2,2,2,2,2,2,2,2,2,2,2,2,2,2,2,2,2,2,2,2,2,2,2,2,2,2,2,2,
2,2,2,2,2,2,2,2,2,2,2,2,2,2,2,2,2,2,2,2,2,2,2,2,2,2,2,2,2,2,2,2,2,2,2,2,
2,2,2,2,2,2,2,2,2,2,2,2,2,2,2,2,2,2,2,2,2,2,2,2,2,2,2,2,2,2,2,2,2,2,2,2,
2,2,2,2,2,2,2,2,2,2,2,2,2,2,2,2,2,2,2,2,2,2,2,2,2,2,2,2,2,2,2,2,2,2,2,2,
2,2,2,2,2,2,2,2,2,2,2,2,2,2,2,2,2,2,2,2,2,2,2,2,2,2,2,2,2,2,2,2,2,2,2,2,
2,2,2,2,2,2,2,2,2,2,2,2,2,2,2,2,2,2,2,2,2,2,2,2,2,2,2,2,2,2,2,2,2,4),(-2.50844686278328,
-2.49269359710946,-2.49008558575366,-2.4883622708675,-2.48698020238702,
-2.48554093339258,-2.48387676855305,-2.48104923796445,-2.47052748535395,
-2.46169824884854,-2.40927370879475,-2.39011232208988,-2.3880333482175,
-2.38700899492203,-2.38627765490984,-2.38548735144296,-2.38408995207614,
-2.37997857323955,-2.37897365427641,-2.32263193855691,-2.30281138695002,
-2.29558160206105,-2.29206441235338,-2.28996182551875,-2.28806477277046,
-2.28662885521865,-2.28525843155444,-2.28299955405137,-2.27725042745633,
-2.22172230361342,-2.19202878921717,-2.18914609840988,-2.18797568070041,
-2.18714608395993,-2.18638531331559,-2.18534072643063,-2.18325517163135,
-2.14909405293217,-2.11819372661656,-2.10192373615194,-2.09561856306411,
-2.09243384275858,-2.08977484950361,-2.088176364545,-2.08817427098319,-2.08817217107111,
-2.08817006480479,-2.08816795214411,-2.08816583306421,-2.08816370755129,
-2.08816157559251,-2.08815943717582,-2.08815729225299,-2.08815514079884,
-2.08815298280516,-2.08815081825945,-2.08814864714711,-2.0881464694097,
-2.08814428503242,-2.08814209399277,-2.08813989626466,-2.08813769183457,
-2.08813548069715,-2.08813326282433,-2.08813103816966,-2.08812880668532,
-2.08812656837791,-2.08812432322499,-2.0881220711897,-2.08811981229296,
-2.08811754646833,-2.08811527370018,-2.08811299399686,-2.08666373707491,
-2.08481666097653,-2.08104518969416,-2.03433451508834,-2.00684839706169,
-1.9964792606921,-1.99069713800261,-1.98917561554482,-1.98827014606644,
-1.98745757131758,-1.9864080104069,-1.98414288410256,-1.94725244983937,
-1.91726077027866,-1.90214232785487,-1.89307326998441,-1.89047470587722,
-1.88887768387116,-1.88742533595696,-1.88555324500763,-1.88165489192682,
-1.84324567770113,-1.79685196372753,-1.79142418549507,-1.78993550419921,
-1.7890373084161,-1.78822263806428,-1.78715891620403,-1.78536855488355,
-1.77410780094252,-1.74865370783611,-1.71845208817896,-1.70307401279213,
-1.6938916628575,-1.6912814623574,-1.68968169940482,-1.68822975202871,-1.68636223337577,
-1.68248811662138,-1.64940378717861,-1.59780878021409,-1.59222814442454,
-1.59072481862256,-1.58982324821766,-1.5890093617776,-1.58795173884615,
-1.58564462829548,-1.55106779783426,-1.52029431890468,-1.49841117253796,
-1.49345329273414,-1.49138908764739,-1.48990525784851,-1.48855795832365,
-1.48676178085577,-1.48238408982283,-1.45014957706135,-1.39855283743501,
-1.39296169726821,-1.39145727788409,-1.39055539804282,-1.38974146572909,
-1.38868410010867,-1.38637879858871,-1.35165356876045,-1.32092379656759,
-1.30488127634249,-1.29541287945244,-1.29277407933726,-1.29116768456516,
-1.28971679482699,-1.28786046831306,-1.28404473999148,-1.254718216548,-1.19693448664752,
-1.19329172453027,-1.19196328705032,-1.19118643839055,-1.19036713646807,
-1.18925662110608,-1.18672562130276,-1.15734303138751,-1.13407748154567,
-1.0982284729303,-1.09432909402739,-1.09245613562873,-1.09100294778709,
-1.0894048337026,-1.08680411426573,-1.07772378660507,-1.06258064529406,
-1.03253252345372,-0.995639022139298,-0.993372450542699,-0.992322219882699,
-0.99150913023227,-0.990603083563992,-0.989080588794925,-0.983294653148478,
-0.972919967976401,-0.945402347789396,-0.898720070387428,-0.89494797745694,
-0.893100102700481,-0.891649992693026,-0.890038466985203,-0.88737741597309,
-0.877680028515178,-0.861094004779503,-0.82991036920981,-0.808512175631676,
-0.805846629480951,-0.795801296732919,-0.794071266208014,-0.793025039191454,
-0.792212524494808,-0.791304338142976,-0.789772113086288,-0.783876550087764,
-0.773222830194575,-0.744543315535899,-0.739068822164123,-0.723124995494738,
-0.71540510415052,-0.698774944894874,-0.695771989103465,-0.693902755948108,
-0.692450050601219,-0.690850034129862,-0.688240734129375,-0.679074988119818,
-0.663735488894132,-0.633529878655933,-0.597108125846816,-0.59483199244795,
-0.593779963638399,-0.592966633888785,-0.592061580143386,-0.590543515768746,
-0.584806458302125,-0.574555012695112,-0.547417638352997,-0.50014862611173,
-0.496392404918132,-0.494547696410197,-0.493097959067071,-0.491484665484791,
-0.488815633917845,-0.479033445576717,-0.462244550613607,-0.43090363297541,
-0.397885518314212,-0.395787033605954,-0.394738922216473,-0.393976970327035,
-0.393165350691325,-0.392033481749677,-0.390752245266113,-0.388514951048301,
-0.371187040586769,-0.339478903250186,-0.301097868591413,-0.297192630978884,
-0.295318546281585,-0.293865231833646,-0.292267731171303,-0.28966970043705,
-0.280615696875707,-0.265532762976925,-0.233216036697687,-0.198564908727071,
-0.196256549317674,-0.195198479051473,-0.194406587686545,-0.194403937985589,
-0.194401311447691,-0.194398703853166,-0.19439611503573,-0.194393544745997,
-0.194390992798672,-0.194388458983883,-0.194385943142771,-0.194383445079622,
-0.194380964588035,-0.194378501484192,-0.194376055600439,-0.194373626762146,
-0.194371214753002,-0.194368819396897,-0.194366440572387,-0.194364078053524,
-0.194361731694794,-0.194359401371431,-0.194357086893942,-0.19435478807974,
-0.194352504782314,-0.194350236864088,-0.194347984188797,-0.194345746569172,
-0.194343523870016,-0.194341315909406,-0.194339122571006,-0.194336943742128,
-0.194334779261849,-0.194332622756615,-0.19433046769248,-0.194328326223556,
-0.193423887794132,-0.192463386738545,-0.191009349453049,-0.188334345306307,
-0.163726432554852,-0.130494358594067,-0.101480257205338,-0.0976618852201546,
-0.095802557755683,-0.094348545910109,-0.0927378994912179,-0.0900902939150393,
-0.0805710127471456,-0.0644203342906257,-0.0357172148943006,-0.000592664738489131),
 .UNSPECIFIED.);
#808=B_SPLINE_CURVE_WITH_KNOTS('',3,(#20709,#20710,#20711,#20712,#20713,
#20714,#20715,#20716,#20717,#20718,#20719,#20720,#20721,#20722,#20723,#20724,
#20725,#20726,#20727,#20728,#20729,#20730,#20731,#20732,#20733,#20734,#20735,
#20736,#20737,#20738,#20739,#20740,#20741,#20742,#20743,#20744,#20745,#20746,
#20747,#20748,#20749,#20750,#20751,#20752,#20753,#20754,#20755,#20756,#20757,
#20758,#20759,#20760,#20761,#20762,#20763,#20764,#20765,#20766,#20767,#20768,
#20769,#20770,#20771,#20772,#20773,#20774,#20775,#20776,#20777,#20778,#20779,
#20780,#20781,#20782,#20783,#20784,#20785,#20786,#20787,#20788,#20789,#20790,
#20791,#20792,#20793,#20794,#20795,#20796,#20797,#20798,#20799,#20800,#20801,
#20802,#20803,#20804,#20805,#20806,#20807,#20808,#20809,#20810,#20811,#20812,
#20813,#20814,#20815,#20816,#20817,#20818,#20819,#20820,#20821,#20822,#20823,
#20824,#20825,#20826,#20827,#20828,#20829,#20830,#20831,#20832,#20833,#20834,
#20835,#20836,#20837,#20838,#20839,#20840,#20841,#20842,#20843,#20844,#20845,
#20846,#20847,#20848,#20849,#20850,#20851,#20852,#20853,#20854,#20855,#20856,
#20857,#20858,#20859,#20860,#20861,#20862,#20863,#20864,#20865,#20866,#20867,
#20868,#20869,#20870,#20871,#20872,#20873,#20874,#20875,#20876,#20877,#20878,
#20879,#20880,#20881,#20882,#20883,#20884,#20885,#20886,#20887,#20888,#20889,
#20890,#20891,#20892,#20893,#20894,#20895,#20896,#20897,#20898,#20899,#20900,
#20901,#20902,#20903,#20904,#20905,#20906,#20907,#20908,#20909,#20910,#20911,
#20912,#20913,#20914,#20915,#20916,#20917,#20918,#20919,#20920,#20921,#20922,
#20923,#20924,#20925,#20926,#20927,#20928,#20929,#20930,#20931,#20932,#20933,
#20934,#20935,#20936,#20937,#20938,#20939,#20940,#20941,#20942,#20943,#20944,
#20945,#20946,#20947,#20948,#20949,#20950,#20951,#20952,#20953,#20954,#20955,
#20956,#20957,#20958,#20959,#20960,#20961,#20962,#20963,#20964,#20965,#20966,
#20967,#20968,#20969,#20970,#20971,#20972,#20973,#20974,#20975,#20976,#20977,
#20978,#20979,#20980,#20981,#20982,#20983,#20984,#20985,#20986,#20987,#20988,
#20989,#20990,#20991,#20992,#20993,#20994,#20995,#20996,#20997,#20998,#20999,
#21000,#21001,#21002,#21003,#21004,#21005,#21006,#21007,#21008,#21009,#21010,
#21011,#21012,#21013,#21014,#21015,#21016,#21017,#21018,#21019,#21020,#21021,
#21022,#21023,#21024,#21025,#21026,#21027,#21028,#21029,#21030,#21031,#21032,
#21033,#21034,#21035,#21036,#21037,#21038,#21039,#21040,#21041,#21042,#21043,
#21044,#21045,#21046,#21047,#21048,#21049,#21050,#21051,#21052,#21053,#21054,
#21055,#21056,#21057,#21058,#21059,#21060,#21061,#21062,#21063,#21064,#21065,
#21066,#21067,#21068,#21069,#21070,#21071,#21072,#21073,#21074,#21075,#21076,
#21077,#21078,#21079,#21080,#21081,#21082,#21083,#21084,#21085,#21086,#21087,
#21088,#21089,#21090,#21091,#21092,#21093,#21094,#21095,#21096,#21097,#21098,
#21099,#21100,#21101,#21102,#21103,#21104,#21105,#21106,#21107,#21108,#21109,
#21110,#21111,#21112,#21113,#21114,#21115,#21116,#21117,#21118,#21119,#21120,
#21121,#21122,#21123,#21124,#21125,#21126,#21127,#21128,#21129,#21130,#21131,
#21132,#21133,#21134,#21135,#21136,#21137,#21138,#21139,#21140,#21141,#21142,
#21143,#21144,#21145,#21146,#21147,#21148,#21149,#21150,#21151,#21152,#21153,
#21154,#21155,#21156,#21157,#21158,#21159,#21160,#21161,#21162,#21163,#21164,
#21165,#21166,#21167,#21168,#21169,#21170,#21171,#21172,#21173,#21174,#21175,
#21176,#21177,#21178,#21179,#21180,#21181,#21182,#21183,#21184,#21185,#21186,
#21187,#21188,#21189,#21190,#21191,#21192),.UNSPECIFIED.,.F.,.F.,(4,2,2,
2,2,2,2,2,2,2,2,2,2,2,2,2,2,2,2,2,2,2,2,2,2,2,2,2,2,2,2,2,2,2,2,2,2,2,2,
2,2,2,2,2,2,2,2,2,2,2,2,2,2,2,2,2,2,2,2,2,2,2,2,2,2,2,2,2,2,2,2,2,2,2,2,
2,2,2,2,2,2,2,2,2,2,2,2,2,2,2,2,2,2,2,2,2,2,2,2,2,2,2,2,2,2,2,2,2,2,2,2,
2,2,2,2,2,2,2,2,2,2,2,2,2,2,2,2,2,2,2,2,2,2,2,2,2,2,2,2,2,2,2,2,2,2,2,2,
2,2,2,2,2,2,2,2,2,2,2,2,2,2,2,2,2,2,2,2,2,2,2,2,2,2,2,2,2,2,2,2,2,2,2,2,
2,2,2,2,2,2,2,2,2,2,2,2,2,2,2,2,2,2,2,2,2,2,2,2,2,2,2,2,2,2,2,2,2,2,2,2,
2,2,2,2,2,2,2,2,2,2,2,2,2,2,2,2,2,2,2,2,2,2,4),(-2.51451748014498,-2.51281605016616,
-2.51112153504224,-2.51011910525733,-2.50933438295832,-2.50853123892221,
-2.50759577763298,-2.50598921910066,-2.50071265804853,-2.43820386699382,
-2.42275426919092,-2.41353438027086,-2.41091602920107,-2.40931180366378,
-2.40785615515298,-2.40598436480432,-2.4021031548632,-2.36042595208092,
-2.32978339185942,-2.31806381459503,-2.31388564373787,-2.31188277546981,
-2.31069533939669,-2.30963013725907,-2.30882797316081,-2.30793356974985,
-2.30646860546513,-2.30257562753262,-2.24873238746428,-2.24061865229924,
-2.22371821589601,-2.21388251872479,-2.21120474638526,-2.20958733574491,
-2.2081346443482,-2.20628719739557,-2.20336246847933,-2.18814361314187,
-2.18424700857255,-2.13467158779746,-2.11493228061176,-2.11253938706279,
-2.11119548225122,-2.11028051572967,-2.10940858707538,-2.10861505222497,
-2.10754363488924,-2.10525796284905,-2.07068628877292,-2.03980463626495,
-2.02362316378698,-2.01408937389062,-2.01144012611985,-2.00982896796326,
-2.0083748090838,-2.00651572927726,-2.00269941385288,-1.95705037396175,
-1.92861687067096,-1.91803713685547,-1.91216723084284,-1.91063498547112,
-1.90972550995586,-1.90891096551386,-1.90786098681056,-1.9061223815688,
-1.89596544710767,-1.87582394808309,-1.86972866210272,-1.83926647145265,
-1.82362157076758,-1.8143170350921,-1.81169007767494,-1.81008381726709,
-1.80862843759378,-1.8067599463239,-1.80289621854521,-1.77123819256394,
-1.73176453243519,-1.71918649634105,-1.71256266027901,-1.71096729541546,
-1.7100437379389,-1.70923198229582,-1.70818828567957,-1.70602125087846,
-1.69050152996651,-1.66958925878186,-1.63926702826325,-1.62380030092132,
-1.61457254875713,-1.61195311354543,-1.61034846637739,-1.60889259416414,
-1.60702073847571,-1.60314019665794,-1.56069632060757,-1.53108510546635,
-1.51359606203268,-1.51154530321925,-1.51052476780479,-1.50979211744674,
-1.50899638908513,-1.50757934882004,-1.50332178714741,-1.46623727881674,
-1.44183979188548,-1.42482121508968,-1.41493572369333,-1.41225286546038,
-1.41063406822525,-1.40918120752971,-1.40733501564324,-1.4044151714081,
-1.38928404185894,-1.38795139028439,-1.33062660049781,-1.31376553139023,
-1.31172858472524,-1.31071075924285,-1.30997835801467,-1.30918118672126,
-1.30775733932055,-1.30344932228793,-1.25785940126824,-1.2171369548455,
-1.21323988210491,-1.21136466546735,-1.20990823020054,-1.20830503531544,
-1.20569264837331,-1.19653730570096,-1.18123584184052,-1.15101685903073,
-1.11432623181867,-1.11204740576523,-1.11099334633399,-1.11017810255916,
-1.10927054220857,-1.10774744890466,-1.10198184587937,-1.09166878447475,
-1.0643494981221,-1.0171422841484,-1.01337199237491,-1.01152180083855,-1.01006840821142,
-1.00845172243285,-1.00577864625508,-0.995998936109896,-0.979232241683642,
-0.947863762797864,-0.924854021013472,-0.914056234885205,-0.912284849432861,
-0.91122513042845,-0.910409132582326,-0.909504679679514,-0.907995364834063,
-0.902379201757033,-0.850674081855965,-0.817525186560206,-0.813640778523217,
-0.811768152790026,-0.810312169114916,-0.808707892487975,-0.806090178075104,
-0.796879938141076,-0.781451404656237,-0.751132663914669,-0.725548825271818,
-0.714307085208493,-0.712514118145953,-0.71144812175965,-0.710631268781825,
-0.709730172278738,-0.708235672675589,-0.702775705085686,-0.655911952764586,
-0.617793122243397,-0.613882863709909,-0.612005260178234,-0.610548725540387,
-0.60894719013894,-0.606341485594939,-0.597249598935944,-0.582092821239112,
-0.551993247914644,-0.514967319096778,-0.512695704590364,-0.51164311067651,
-0.510828179271047,-0.509920066255509,-0.508394071355859,-0.502594508459982,
-0.492195024529594,-0.464607160059865,-0.417833124275506,-0.414049560375358,
-0.412196913027027,-0.410781802732475,-0.409212482696472,-0.407573839880407,
-0.405173646659386,-0.400927396223008,-0.366828311922889,-0.325473031412894,
-0.314706415372037,-0.312936709286618,-0.311877541517773,-0.311061693701066,
-0.310157108311761,-0.308646926398554,-0.30302028997174,-0.251324038314476,
-0.218195101883811,-0.214306882080081,-0.212433630198597,-0.211016651966711,
-0.209458889563924,-0.20783588102246,-0.205473467782535,-0.201321584235745,
-0.192246664524157,-0.164335347075445,-0.118213306621763,-0.113931713909945,
-0.11251151817116,-0.111715175874615,-0.110982727684619,-0.109963631395247,
-0.107919860740196,-0.0907425573702373,-0.0254247460849162,-0.0166005098880669,
-0.0137791124022887,-0.012113383123493,-0.0106716896885479,-0.00928464804163324,
-0.00755312043015414,-0.00448544266794431,-0.000592058400578167),
 .UNSPECIFIED.);
#809=B_SPLINE_CURVE_WITH_KNOTS('',3,(#21194,#21195,#21196,#21197,#21198,
#21199,#21200,#21201,#21202,#21203,#21204,#21205,#21206,#21207,#21208,#21209,
#21210,#21211,#21212,#21213,#21214,#21215,#21216,#21217,#21218,#21219,#21220,
#21221,#21222,#21223,#21224,#21225,#21226,#21227,#21228,#21229,#21230,#21231,
#21232,#21233,#21234,#21235,#21236,#21237,#21238,#21239,#21240,#21241,#21242,
#21243,#21244,#21245,#21246,#21247,#21248,#21249,#21250,#21251,#21252,#21253,
#21254,#21255,#21256,#21257,#21258,#21259,#21260,#21261,#21262,#21263,#21264,
#21265,#21266,#21267,#21268,#21269,#21270,#21271,#21272,#21273,#21274,#21275,
#21276,#21277,#21278,#21279,#21280,#21281,#21282,#21283,#21284,#21285,#21286,
#21287,#21288,#21289,#21290,#21291,#21292,#21293,#21294,#21295,#21296,#21297,
#21298,#21299,#21300,#21301,#21302,#21303,#21304,#21305,#21306,#21307,#21308,
#21309,#21310,#21311,#21312,#21313,#21314,#21315,#21316,#21317,#21318,#21319,
#21320,#21321,#21322,#21323,#21324,#21325,#21326,#21327,#21328,#21329,#21330,
#21331,#21332,#21333,#21334,#21335,#21336,#21337,#21338,#21339,#21340,#21341,
#21342,#21343,#21344,#21345,#21346,#21347,#21348,#21349,#21350,#21351,#21352,
#21353,#21354,#21355,#21356,#21357,#21358,#21359,#21360,#21361,#21362,#21363,
#21364,#21365,#21366,#21367,#21368,#21369,#21370,#21371,#21372,#21373,#21374,
#21375,#21376,#21377,#21378,#21379,#21380,#21381,#21382,#21383,#21384,#21385,
#21386,#21387,#21388,#21389,#21390,#21391,#21392,#21393,#21394,#21395,#21396,
#21397,#21398,#21399,#21400,#21401,#21402,#21403,#21404,#21405,#21406,#21407,
#21408,#21409,#21410,#21411,#21412,#21413,#21414,#21415,#21416,#21417,#21418,
#21419,#21420,#21421,#21422,#21423,#21424,#21425,#21426,#21427,#21428,#21429,
#21430,#21431,#21432,#21433,#21434,#21435,#21436,#21437,#21438,#21439,#21440,
#21441,#21442,#21443,#21444,#21445,#21446,#21447,#21448,#21449,#21450,#21451,
#21452,#21453,#21454,#21455,#21456,#21457,#21458,#21459,#21460,#21461,#21462,
#21463,#21464,#21465,#21466,#21467,#21468,#21469,#21470,#21471,#21472,#21473,
#21474,#21475,#21476,#21477,#21478,#21479,#21480,#21481,#21482,#21483,#21484,
#21485,#21486,#21487,#21488,#21489,#21490,#21491,#21492,#21493,#21494,#21495,
#21496,#21497,#21498,#21499,#21500,#21501,#21502,#21503,#21504,#21505,#21506,
#21507,#21508,#21509,#21510,#21511,#21512,#21513,#21514,#21515,#21516,#21517,
#21518,#21519,#21520,#21521,#21522,#21523,#21524,#21525,#21526,#21527,#21528,
#21529,#21530,#21531,#21532,#21533,#21534,#21535,#21536,#21537,#21538,#21539,
#21540,#21541,#21542,#21543,#21544,#21545,#21546,#21547,#21548,#21549,#21550,
#21551,#21552,#21553,#21554,#21555,#21556,#21557,#21558,#21559,#21560,#21561,
#21562,#21563,#21564,#21565,#21566,#21567,#21568,#21569,#21570,#21571,#21572,
#21573,#21574,#21575,#21576,#21577,#21578,#21579,#21580,#21581,#21582,#21583,
#21584,#21585,#21586,#21587,#21588,#21589,#21590,#21591,#21592,#21593,#21594,
#21595,#21596,#21597,#21598,#21599,#21600,#21601,#21602,#21603,#21604,#21605,
#21606,#21607,#21608,#21609,#21610,#21611,#21612,#21613,#21614,#21615,#21616,
#21617,#21618,#21619,#21620,#21621,#21622,#21623,#21624,#21625,#21626,#21627,
#21628,#21629,#21630,#21631,#21632,#21633,#21634,#21635,#21636,#21637,#21638,
#21639,#21640,#21641,#21642,#21643,#21644,#21645,#21646,#21647,#21648,#21649,
#21650,#21651,#21652,#21653,#21654,#21655,#21656,#21657,#21658,#21659,#21660,
#21661,#21662,#21663,#21664,#21665,#21666,#21667,#21668,#21669,#21670,#21671,
#21672,#21673,#21674,#21675,#21676,#21677,#21678,#21679,#21680,#21681,#21682,
#21683,#21684,#21685,#21686,#21687,#21688,#21689,#21690,#21691,#21692,#21693,
#21694,#21695,#21696,#21697,#21698,#21699,#21700,#21701,#21702,#21703,#21704,
#21705,#21706,#21707,#21708,#21709,#21710,#21711,#21712,#21713,#21714,#21715,
#21716,#21717,#21718,#21719,#21720,#21721,#21722,#21723,#21724,#21725,#21726,
#21727,#21728,#21729,#21730,#21731),.UNSPECIFIED.,.F.,.F.,(4,2,2,2,2,2,
2,2,2,2,2,2,2,2,2,2,2,2,2,2,2,2,2,2,2,2,2,2,2,2,2,2,2,2,2,2,2,2,2,2,2,2,
2,2,2,2,2,2,2,2,2,2,2,2,2,2,2,2,2,2,2,2,2,2,2,2,2,2,2,2,2,2,2,2,2,2,2,2,
2,2,2,2,2,2,2,2,2,2,2,2,2,2,2,2,2,2,2,2,2,2,2,2,2,2,2,2,2,2,2,2,2,2,2,2,
2,2,2,2,2,2,2,2,2,2,2,2,2,2,2,2,2,2,2,2,2,2,2,2,2,2,2,2,2,2,2,2,2,2,2,2,
2,2,2,2,2,2,2,2,2,2,2,2,2,2,2,2,2,2,2,2,2,2,2,2,2,2,2,2,2,2,2,2,2,2,2,2,
2,2,2,2,2,2,2,2,2,2,2,2,2,2,2,2,2,2,2,2,2,2,2,2,2,2,2,2,2,2,2,2,2,2,2,2,
2,2,2,2,2,2,2,2,2,2,2,2,2,2,2,2,2,2,2,2,2,2,2,2,2,2,2,2,2,2,2,2,2,2,2,2,
2,2,2,2,2,2,2,2,2,2,4),(-2.51337701081457,-2.44175496188814,-2.43232013167534,
-2.42691106705794,-2.42542187443154,-2.4245222114906,-2.42370540418666,
-2.422637803107,-2.42083854640493,-2.40945366880344,-2.38403577169911,-2.33627303079072,
-2.33126759941285,-2.3285694654559,-2.32680669341505,-2.32514847326009,
-2.32513968378661,-2.32513062619519,-2.32512128988085,-2.32511166368,-2.32510173584106,
-2.32509149399477,-2.32508092509959,-2.32507001540138,-2.32505875038494,
-2.3250471147153,-2.32503509218982,-2.32502266565727,-2.32500981697094,
-2.32499652691343,-2.3249827750869,-2.32496853985471,-2.32495379823724,
-2.32493852580531,-2.32492269656457,-2.32490628282391,-2.32488925506893,
-2.32487158181167,-2.32485460570236,-2.32343193866557,-2.32155744886606,
-2.31765931856103,-2.28301565004191,-2.23486676217071,-2.22751227007412,
-2.22586333200029,-2.22492827553432,-2.2241187287339,-2.22309386349109,
-2.22108661600093,-2.20897206153336,-2.19667625325695,-2.18340034720444,
-2.1705284005456,-2.13525484307865,-2.1309361846584,-2.12850745587442,-2.12685732122389,
-2.12527894809992,-2.12527638253071,-2.12527381140904,-2.12527123473,-2.12526865245837,
-2.12526606455742,-2.12526347100091,-2.12526087176631,-2.12525826683488,
-2.12383743314929,-2.12198603083567,-2.11820571215948,-2.07138824939126,
-2.04383786312378,-2.03344494286484,-2.02764946809671,-2.02612438352324,
-2.02521678446522,-2.02440229137655,-2.02335024192047,-2.02107970375484,
-1.98409026661811,-1.95403300340289,-1.9388849465808,-1.92979715559465,
-1.92719273570985,-1.9255920100286,-1.92413622479654,-1.92225960568385,
-1.91835146735431,-1.88025662741589,-1.83337358987405,-1.82791425729708,
-1.82642027044494,-1.8255195560909,-1.82470309695526,-1.82363768674076,
-1.82184586508555,-1.81061543093734,-1.78504896347642,-1.75477371264236,
-1.73935595049575,-1.73015053686047,-1.72753409021477,-1.7259305648945,
-1.7244752460035,-1.72260345146334,-1.71872068439475,-1.68558826879106,
-1.63388601061939,-1.62825470498433,-1.62674437656348,-1.62583992724974,
-1.6250243539895,-1.62396575204902,-1.62219744047129,-1.6114512541093,-1.6074487561025,
-1.60023750005035,-1.56836135826275,-1.53287156310491,-1.52881747805682,
-1.52691240211694,-1.52545248796916,-1.52406001135835,-1.52169949866923,
-1.51538385695729,-1.46749362985565,-1.44476620087261,-1.43437243572969,
-1.4285761170391,-1.42705065311463,-1.42614279782867,-1.42532805385597,
-1.42427565286181,-1.42200425147217,-1.38507969267971,-1.35498717312345,
-1.33980202010157,-1.33069728992017,-1.32809064791164,-1.3264891187462,
-1.32503297288439,-1.32315640929157,-1.31925028299771,-1.28373035405147,
-1.2568487800976,-1.23026014804358,-1.22790305777441,-1.22683463808489,
-1.22601759816784,-1.22511809574486,-1.22363006178803,-1.21823465894979,
-1.20883484843506,-1.18516764214781,-1.13675914105684,-1.13318962580626,
-1.12929649643632,-1.12742252236514,-1.12596676095213,-1.12436401360257,
-1.12175169260301,-1.11258986543445,-1.09727104272567,-1.06704575803358,
-1.03042666948668,-1.02814843632754,-1.02709475331427,-1.02627984542228,
-1.0253727079959,-1.02385043168163,-1.01808916334942,-1.00778523665731,
-0.980492200535458,-0.933282303576771,-0.929514228888169,-0.927664944807788,
-0.926212182325873,-0.924596112064336,-0.921923855420353,-0.912144958699017,
-0.895377393069233,-0.864016021147467,-0.840970858773963,-0.830235678913826,
-0.828467925237498,-0.827409501255432,-0.826593969118352,-0.825689453552467,
-0.824178781859182,-0.818543501620052,-0.80855460774344,-0.78241196238822,
-0.737497024983468,-0.733079692343254,-0.729979966827759,-0.728100113551347,
-0.726639294218764,-0.72505503853134,-0.722525611942107,-0.714153855801022,
-0.700607919723632,-0.644693830842097,-0.642315277417697,-0.630576911641671,
-0.628585388550131,-0.627563678257295,-0.626754108467323,-0.625816167135859,
-0.624155122414832,-0.6166320182895,-0.567958280853421,-0.53402057135248,
-0.530127586891729,-0.528253629259245,-0.526797856906971,-0.525195073556982,
-0.522582639860281,-0.513419870160197,-0.498098939934887,-0.467871775514895,
-0.43126357593716,-0.429207007670072,-0.428168379694435,-0.427407867547,
-0.426591323531362,-0.425449245758386,-0.424149242383244,-0.421866934738057,
-0.403882436285767,-0.362607584903254,-0.334182778948562,-0.330378163671569,
-0.328521578285634,-0.32706791515303,-0.325455813320718,-0.32280158310927,
-0.313213181689532,-0.296899260920132,-0.243764744231135,-0.240237139387362,
-0.230882634924572,-0.22918786178731,-0.22813976010179,-0.227327639154328,
-0.226566885683579,-0.225185861025886,-0.220767167053036,-0.213575914891285,
-0.187113952443034,-0.138082375652246,-0.131803064687726,-0.129456507495738,
-0.128066671179677,-0.126605443410526,-0.124691895206008,-0.120593875903446,
-0.0835466320727342,-0.0586127139958924,-0.0515117633699154,-0.046961085874668,
-0.0316015195739975,-0.0294403800752858,-0.0283979762831173,-0.0275865095537347,
-0.0268252214746157,-0.0259135823220781,-0.0245776849928189,-0.0192352210050872,
-0.000591821998673919),.UNSPECIFIED.);
#810=B_SPLINE_CURVE_WITH_KNOTS('',3,(#21733,#21734,#21735,#21736,#21737,
#21738,#21739,#21740,#21741,#21742,#21743,#21744,#21745,#21746,#21747,#21748,
#21749,#21750,#21751,#21752,#21753,#21754,#21755,#21756,#21757,#21758,#21759,
#21760,#21761,#21762,#21763,#21764,#21765,#21766,#21767,#21768,#21769,#21770,
#21771,#21772,#21773,#21774,#21775,#21776,#21777,#21778,#21779,#21780,#21781,
#21782,#21783,#21784,#21785,#21786,#21787,#21788,#21789,#21790,#21791,#21792,
#21793,#21794,#21795,#21796,#21797,#21798,#21799,#21800,#21801,#21802,#21803,
#21804,#21805,#21806,#21807,#21808,#21809,#21810,#21811,#21812,#21813,#21814,
#21815,#21816,#21817,#21818,#21819,#21820,#21821,#21822,#21823,#21824,#21825,
#21826,#21827,#21828,#21829,#21830,#21831,#21832,#21833,#21834,#21835,#21836,
#21837,#21838,#21839,#21840,#21841,#21842,#21843,#21844,#21845,#21846,#21847,
#21848,#21849,#21850,#21851,#21852,#21853,#21854,#21855,#21856,#21857,#21858,
#21859,#21860,#21861,#21862,#21863,#21864,#21865,#21866,#21867,#21868,#21869,
#21870,#21871,#21872,#21873,#21874,#21875,#21876,#21877,#21878,#21879,#21880,
#21881,#21882,#21883,#21884,#21885,#21886,#21887,#21888,#21889,#21890,#21891,
#21892,#21893,#21894,#21895,#21896,#21897,#21898,#21899,#21900,#21901,#21902,
#21903,#21904,#21905,#21906,#21907,#21908,#21909,#21910,#21911,#21912,#21913,
#21914,#21915,#21916,#21917,#21918,#21919,#21920,#21921,#21922),
 .UNSPECIFIED.,.F.,.F.,(4,3,3,3,3,3,3,3,3,3,3,3,3,3,3,3,3,3,3,3,3,3,3,3,
3,3,3,3,3,3,3,3,3,3,3,3,3,3,3,3,3,3,3,3,3,3,3,3,3,3,3,3,3,3,3,3,3,3,3,3,
3,3,3,4),(191.637151868978,191.750774088638,191.864712447052,191.979141592408,
192.065437505541,192.170383320405,192.275171385404,192.379835916045,192.484434423837,
192.589002493249,192.693575664582,192.798259619649,192.90300468305,193.00793252951,
193.064118373902,193.169064188766,193.273852253765,193.378516784406,193.483115292198,
193.58768336161,193.692256532943,193.79694048801,193.901685551411,194.006613397871,
194.062799242263,194.167745057127,194.272533122126,194.377197652767,194.481796160559,
194.586364229971,194.690937401303,194.79562135637,194.900366419771,195.005294266231,
195.061480110623,195.166425925487,195.271213990486,195.375878521127,195.480477028919,
195.585045098331,195.689618269664,195.794302224731,195.899047288131,196.003975134592,
196.060160978984,196.165106793848,196.269894858847,196.374559389488,196.47915789728,
196.583725966692,196.688299138025,196.792983093092,196.897728156493,197.002656002953,
197.058841847345,197.166528763385,197.269778351084,197.372930295233,197.476022111771,
197.579091227138,197.682228012493,197.785405386153,197.888722207365,197.920337175666),
 .UNSPECIFIED.);
#811=B_SPLINE_CURVE_WITH_KNOTS('',3,(#21924,#21925,#21926,#21927,#21928,
#21929,#21930,#21931,#21932,#21933),.UNSPECIFIED.,.F.,.F.,(4,1,1,1,1,1,
1,4),(185.353966561798,186.073352295377,187.072033163737,188.070714032098,
189.069394900459,190.06807576882,191.06675663718,191.637151868978),
 .UNSPECIFIED.);
#812=B_SPLINE_CURVE_WITH_KNOTS('',3,(#21935,#21936,#21937,#21938,#21939,
#21940,#21941,#21942,#21943,#21944,#21945,#21946,#21947,#21948,#21949,#21950,
#21951,#21952,#21953,#21954,#21955,#21956,#21957,#21958,#21959,#21960,#21961,
#21962,#21963,#21964,#21965,#21966,#21967,#21968,#21969,#21970,#21971,#21972,
#21973,#21974,#21975,#21976,#21977,#21978,#21979,#21980,#21981,#21982,#21983,
#21984,#21985,#21986,#21987,#21988,#21989,#21990,#21991,#21992,#21993,#21994,
#21995,#21996,#21997,#21998,#21999,#22000,#22001,#22002,#22003,#22004,#22005,
#22006,#22007,#22008,#22009,#22010,#22011,#22012,#22013,#22014,#22015,#22016,
#22017,#22018,#22019,#22020,#22021,#22022,#22023,#22024,#22025,#22026,#22027,
#22028,#22029,#22030,#22031,#22032,#22033,#22034,#22035,#22036,#22037,#22038,
#22039,#22040,#22041,#22042,#22043,#22044,#22045,#22046,#22047,#22048,#22049,
#22050,#22051,#22052,#22053,#22054,#22055,#22056,#22057,#22058,#22059,#22060,
#22061,#22062,#22063,#22064,#22065,#22066,#22067,#22068,#22069,#22070,#22071,
#22072,#22073,#22074,#22075,#22076,#22077,#22078,#22079,#22080,#22081,#22082,
#22083,#22084,#22085,#22086,#22087,#22088,#22089,#22090,#22091,#22092,#22093,
#22094,#22095,#22096,#22097,#22098,#22099,#22100,#22101,#22102,#22103,#22104,
#22105,#22106,#22107,#22108,#22109,#22110,#22111,#22112,#22113,#22114,#22115,
#22116,#22117,#22118,#22119,#22120,#22121,#22122,#22123,#22124,#22125,#22126,
#22127,#22128,#22129,#22130,#22131,#22132,#22133,#22134,#22135,#22136,#22137,
#22138,#22139,#22140,#22141,#22142,#22143,#22144,#22145,#22146,#22147,#22148,
#22149,#22150,#22151,#22152,#22153,#22154,#22155,#22156,#22157,#22158,#22159,
#22160,#22161,#22162,#22163,#22164,#22165,#22166,#22167,#22168,#22169,#22170,
#22171,#22172,#22173,#22174,#22175,#22176,#22177,#22178,#22179,#22180,#22181,
#22182,#22183,#22184,#22185,#22186,#22187,#22188,#22189,#22190,#22191,#22192,
#22193,#22194,#22195,#22196,#22197,#22198,#22199,#22200,#22201,#22202,#22203,
#22204,#22205,#22206,#22207,#22208,#22209,#22210,#22211,#22212,#22213,#22214,
#22215,#22216,#22217,#22218,#22219,#22220,#22221,#22222,#22223,#22224,#22225,
#22226,#22227,#22228,#22229,#22230,#22231,#22232,#22233,#22234,#22235,#22236,
#22237,#22238,#22239,#22240,#22241,#22242,#22243,#22244,#22245,#22246,#22247,
#22248,#22249,#22250,#22251,#22252,#22253,#22254,#22255,#22256,#22257,#22258,
#22259,#22260,#22261,#22262,#22263,#22264,#22265,#22266,#22267,#22268,#22269,
#22270,#22271,#22272,#22273,#22274,#22275,#22276,#22277,#22278,#22279,#22280,
#22281,#22282,#22283,#22284,#22285,#22286,#22287,#22288,#22289,#22290,#22291,
#22292,#22293,#22294,#22295,#22296,#22297,#22298,#22299,#22300,#22301,#22302,
#22303,#22304,#22305,#22306,#22307,#22308,#22309,#22310,#22311,#22312,#22313,
#22314,#22315,#22316,#22317,#22318,#22319,#22320,#22321,#22322,#22323,#22324,
#22325,#22326,#22327,#22328,#22329,#22330,#22331,#22332,#22333,#22334,#22335,
#22336,#22337,#22338,#22339,#22340,#22341,#22342,#22343,#22344,#22345,#22346,
#22347,#22348,#22349,#22350,#22351,#22352,#22353,#22354,#22355,#22356,#22357,
#22358,#22359,#22360,#22361,#22362,#22363,#22364,#22365,#22366,#22367,#22368,
#22369,#22370,#22371,#22372,#22373,#22374,#22375,#22376,#22377,#22378,#22379,
#22380,#22381,#22382,#22383,#22384,#22385,#22386,#22387,#22388,#22389,#22390,
#22391,#22392,#22393,#22394,#22395,#22396,#22397,#22398,#22399,#22400,#22401,
#22402,#22403,#22404,#22405,#22406,#22407,#22408),.UNSPECIFIED.,.F.,.F.,
(4,2,2,2,2,2,2,2,2,2,2,2,2,2,2,2,2,2,2,2,2,2,2,2,2,2,2,2,2,2,2,2,2,2,2,
2,2,2,2,2,2,2,2,2,2,2,2,2,2,2,2,2,2,2,2,2,2,2,2,2,2,2,2,2,2,2,2,2,2,2,2,
2,2,2,2,2,2,2,2,2,2,2,2,2,2,2,2,2,2,2,2,2,2,2,2,2,2,2,2,2,2,2,2,2,2,2,2,
2,2,2,2,2,2,2,2,2,2,2,2,2,2,2,2,2,2,2,2,2,2,2,2,2,2,2,2,2,2,2,2,2,2,2,2,
2,2,2,2,2,2,2,2,2,2,2,2,2,2,2,2,2,2,2,2,2,2,2,2,2,2,2,2,2,2,2,2,2,2,2,2,
2,2,2,2,2,2,2,2,2,2,2,2,2,2,2,2,2,2,2,2,2,2,2,2,2,2,2,2,2,2,2,2,2,2,2,2,
2,2,2,2,2,2,2,2,2,2,2,2,2,2,2,2,2,2,2,2,2,4),(-2.51299292533393,-2.46610032634122,
-2.46206378997104,-2.46011041784798,-2.45850469333273,-2.45757913799288,
-2.4567682118256,-2.45572898942691,-2.45358302022776,-2.43863427872868,
-2.43316037388253,-2.40673806167597,-2.38893652783773,-2.36566745758289,
-2.36093429796256,-2.35934391675669,-2.35798712656598,-2.35653568341548,
-2.35469615275721,-2.35179637727749,-2.33697269141598,-2.32547217752391,
-2.29699651997549,-2.27462371193185,-2.2655322000705,-2.26028687978431,
-2.25880080711061,-2.25790189603071,-2.25708496729721,-2.2560161327386,
-2.25365587296462,-2.22451387920756,-2.16999360416562,-2.16480385946966,
-2.16086376694101,-2.15898225384938,-2.15752056097361,-2.15613353016986,
-2.15379957661019,-2.14760046125139,-2.09710347535054,-2.07485550658659,
-2.06142571189698,-2.05944847028688,-2.05844328900751,-2.0577128102949,
-2.05679240390574,-2.05520987130727,-2.04955943588014,-2.04653170144409,
-1.98701560576162,-1.97182627808625,-1.96272074299377,-1.96011471053441,
-1.95851373520106,-1.95705821089759,-1.95518261419357,-1.95127910466021,
-1.91303016559547,-1.86629553548218,-1.8608438570258,-1.85935070707653,
-1.85845024074039,-1.85763382537925,-1.85656823109102,-1.85477558022048,
-1.84352510351551,-1.81798063684283,-1.78770996798438,-1.77229553056732,
-1.76309182924484,-1.76047573615312,-1.758872399353,-1.75741723310318,-1.75554560904556,
-1.75166310211164,-1.71852209800046,-1.66682131944643,-1.66120458745397,
-1.65969571875036,-1.6587916564594,-1.6579760929404,-1.65691705506076,-1.6546098411465,
-1.61957674401776,-1.5888612071534,-1.57288577854611,-1.56344045462846,
-1.56080029019318,-1.55919145338704,-1.55773731249577,-1.55587537643359,
-1.55204295474933,-1.52218890243156,-1.48035045393073,-1.46247803346655,
-1.46041977583916,-1.45939796528743,-1.45866539178634,-1.45787074520855,
-1.45645808246911,-1.45263812095128,-1.44841242693519,-1.38677694363034,
-1.37232739742528,-1.36354746496801,-1.36097460841757,-1.35938084450656,
-1.35792311275027,-1.35606353015883,-1.35213968277445,-1.34847991301223,
-1.30448661852658,-1.26659330698944,-1.26329337279937,-1.2608540115656,
-1.2597588675079,-1.25894074574546,-1.25815682943634,-1.25679763219949,
-1.25258907853114,-1.22532319393729,-1.20364082273283,-1.16616660489521,
-1.16225731661163,-1.16038034418743,-1.1589243723157,-1.15732352944667,
-1.15471911733276,-1.14563340123966,-1.13048851089312,-1.10040561445415,
-1.06338078137792,-1.06110997146444,-1.06005777661735,-1.05924316570366,
-1.05833542247115,-1.05681007670588,-1.05101330486018,-1.04061918806097,
-1.01305002369911,-0.966280312953325,-0.962501154673286,-0.960649818816324,
-0.959196992760356,-0.957582448703555,-0.954916413668964,-0.945200863852007,
-0.928583773945686,-0.897341724027673,-0.875902743865246,-0.873242016439939,
-0.863169666209752,-0.861435962530015,-0.860387647753016,-0.859573594058342,
-0.858663778337828,-0.857129004969654,-0.851226035918646,-0.840561660960375,
-0.811855754216749,-0.808721060416394,-0.766794006787699,-0.762913985947473,
-0.761042791253477,-0.759587615216392,-0.757983919675891,-0.755366455331668,
-0.74614997146241,-0.730704019666438,-0.7003806679752,-0.676933827109281,
-0.66377556885267,-0.661698076332219,-0.660672476293721,-0.659862788128503,
-0.658928060004274,-0.657280907945926,-0.649953497122562,-0.635361763496325,
-0.627958062434114,-0.591352052038193,-0.58191173820703,-0.566209770861689,
-0.563255205789475,-0.561398929389737,-0.559945579242589,-0.55833389742747,
-0.555680526470597,-0.546097031080555,-0.529793288114636,-0.470390524506826,
-0.463447520394626,-0.461763543492189,-0.460810381162685,-0.46000988678922,
-0.459011838063871,-0.457069756412612,-0.443622053739423,-0.421490555613157,
-0.370842893860754,-0.364652952795936,-0.362320399412465,-0.360933427717102,
-0.359471225114624,-0.357588124787432,-0.353632377656631,-0.348422104912957,
-0.293861808142017,-0.26473991407143,-0.262378762688631,-0.261309605297285,
-0.260492467645774,-0.259593359841965,-0.258107041695583,-0.252729151400296,
-0.243371670503992,-0.217523700028426,-0.18705412150265,-0.167107334113529,
-0.163940212793613,-0.16204038194702,-0.16057638547168,-0.159222387948782,
-0.157677014250814,-0.153394738580995,-0.132342780601224,-0.114548811848656,
-0.0676986060079104,-0.0634446307204431,-0.0620282532650802,-0.0612327688530294,
-0.0605002554972148,-0.059479786098308,-0.0574287014922809,-0.0399052997808067,
-0.000592787106899905),.UNSPECIFIED.);
#813=B_SPLINE_CURVE_WITH_KNOTS('',3,(#22410,#22411,#22412,#22413,#22414,
#22415,#22416,#22417,#22418,#22419,#22420,#22421,#22422,#22423,#22424,#22425,
#22426,#22427,#22428,#22429,#22430,#22431,#22432,#22433,#22434,#22435,#22436,
#22437,#22438,#22439,#22440,#22441,#22442,#22443,#22444,#22445,#22446,#22447,
#22448,#22449,#22450,#22451,#22452,#22453,#22454,#22455,#22456,#22457,#22458,
#22459,#22460,#22461,#22462,#22463,#22464,#22465,#22466,#22467,#22468,#22469,
#22470,#22471,#22472,#22473,#22474,#22475,#22476,#22477,#22478,#22479,#22480,
#22481,#22482,#22483,#22484,#22485,#22486,#22487,#22488,#22489,#22490,#22491,
#22492,#22493,#22494,#22495,#22496,#22497,#22498,#22499,#22500,#22501,#22502,
#22503,#22504,#22505,#22506,#22507,#22508,#22509,#22510,#22511,#22512,#22513,
#22514,#22515,#22516,#22517,#22518,#22519,#22520,#22521,#22522,#22523,#22524,
#22525,#22526,#22527,#22528,#22529,#22530,#22531,#22532,#22533,#22534,#22535,
#22536,#22537,#22538,#22539,#22540,#22541,#22542,#22543,#22544,#22545,#22546,
#22547,#22548,#22549,#22550,#22551,#22552,#22553,#22554,#22555,#22556,#22557,
#22558,#22559,#22560,#22561,#22562,#22563,#22564,#22565,#22566,#22567,#22568,
#22569,#22570,#22571,#22572,#22573,#22574,#22575,#22576,#22577,#22578,#22579,
#22580,#22581,#22582,#22583,#22584,#22585,#22586,#22587,#22588,#22589,#22590,
#22591,#22592,#22593,#22594,#22595,#22596,#22597,#22598,#22599),
 .UNSPECIFIED.,.F.,.F.,(4,3,3,3,3,3,3,3,3,3,3,3,3,3,3,3,3,3,3,3,3,3,3,3,
3,3,3,3,3,3,3,3,3,3,3,3,3,3,3,3,3,3,3,3,3,3,3,3,3,3,3,3,3,3,3,3,3,3,3,3,
3,3,3,4),(166.504410640259,166.610530706907,166.716694140663,166.823018116949,
166.929429397535,167.036059350254,167.098415796522,167.203361611386,167.308149676385,
167.412814207026,167.517412714818,167.62198078423,167.726553955562,167.831237910629,
167.93598297403,168.04091082049,168.097096664883,168.202042479747,168.306830544746,
168.411495075388,168.516093583179,168.620661652592,168.725234823924,168.829918778992,
168.934663842393,169.039591688853,169.095777533244,169.200723348108,169.305511413107,
169.410175943748,169.51477445154,169.619342520952,169.723915692285,169.828599647352,
169.933344710753,170.038272557213,170.094458401605,170.199404216469,170.304192281468,
170.408856812109,170.513455319901,170.618023389313,170.722596560645,170.827280515712,
170.932025579113,171.036953425573,171.093139269965,171.198085084829,171.302873149828,
171.407537680469,171.512136188261,171.616704257673,171.721277429005,171.825961384073,
171.930706447474,172.035634293934,172.091820138326,172.196174855182,172.300380791839,
172.404474543733,172.508507006465,172.61250123859,172.716536906099,172.787595947439),
 .UNSPECIFIED.);
#814=B_SPLINE_CURVE_WITH_KNOTS('',3,(#22601,#22602,#22603,#22604,#22605,
#22606,#22607,#22608,#22609,#22610),.UNSPECIFIED.,.F.,.F.,(4,1,1,1,1,1,
1,4),(160.221234148943,161.106330586358,162.105011454719,163.103692323079,
164.10237319144,165.101054059801,166.099734928162,166.504404121023),
 .UNSPECIFIED.);
#815=B_SPLINE_CURVE_WITH_KNOTS('',3,(#22612,#22613,#22614,#22615,#22616,
#22617,#22618,#22619,#22620,#22621,#22622,#22623,#22624,#22625,#22626,#22627,
#22628,#22629,#22630,#22631,#22632,#22633,#22634,#22635,#22636,#22637,#22638,
#22639,#22640,#22641,#22642,#22643,#22644,#22645,#22646,#22647,#22648,#22649,
#22650,#22651,#22652,#22653,#22654,#22655,#22656,#22657,#22658,#22659,#22660,
#22661,#22662,#22663,#22664,#22665,#22666,#22667,#22668,#22669,#22670,#22671,
#22672,#22673,#22674,#22675,#22676,#22677,#22678,#22679,#22680,#22681,#22682,
#22683,#22684,#22685,#22686,#22687,#22688,#22689,#22690,#22691,#22692,#22693,
#22694,#22695,#22696,#22697,#22698,#22699,#22700,#22701,#22702,#22703,#22704,
#22705,#22706,#22707,#22708,#22709,#22710,#22711,#22712,#22713,#22714,#22715,
#22716,#22717,#22718,#22719,#22720,#22721,#22722,#22723,#22724,#22725,#22726,
#22727,#22728,#22729,#22730,#22731,#22732,#22733,#22734,#22735,#22736,#22737,
#22738,#22739,#22740,#22741,#22742,#22743,#22744,#22745,#22746,#22747,#22748,
#22749,#22750,#22751,#22752,#22753,#22754,#22755,#22756,#22757,#22758,#22759,
#22760,#22761,#22762,#22763,#22764,#22765,#22766,#22767,#22768,#22769,#22770,
#22771,#22772,#22773,#22774,#22775,#22776,#22777,#22778,#22779,#22780,#22781,
#22782,#22783,#22784,#22785,#22786,#22787,#22788,#22789,#22790,#22791,#22792,
#22793,#22794,#22795,#22796,#22797,#22798,#22799,#22800,#22801),
 .UNSPECIFIED.,.F.,.F.,(4,3,3,3,3,3,3,3,3,3,3,3,3,3,3,3,3,3,3,3,3,3,3,3,
3,3,3,3,3,3,3,3,3,3,3,3,3,3,3,3,3,3,3,3,3,3,3,3,3,3,3,3,3,3,3,3,3,3,3,3,
3,3,3,4),(153.9380400259,154.098367385836,154.115564507833,154.220510322697,
154.325298387696,154.429962918337,154.534561426129,154.639129495541,154.743702666873,
154.84838662194,154.953131685341,155.058059531801,155.114245376193,155.219191191057,
155.323979256056,155.428643786697,155.533242294489,155.637810363901,155.742383535233,
155.847067490301,155.951812553701,156.056740400161,156.112926244554,156.217872059418,
156.322660124417,156.427324655059,156.53192316285,156.636491232262,156.741064403595,
156.845748358663,156.950493422063,157.055421268524,157.111607112915,157.216552927779,
157.321340992778,157.426005523419,157.530604031211,157.635172100623,157.739745271955,
157.844429227023,157.949174290423,158.054102136884,158.110287981276,158.21523379614,
158.320021861139,158.42468639178,158.529284899572,158.633852968984,158.738426140316,
158.843110095383,158.947855158784,159.052783005244,159.108968849636,159.2139146645,
159.318702729499,159.42336726014,159.527965767932,159.632533837343,159.737107008676,
159.841790963743,159.946536027144,160.051463873604,160.107649717997,160.22122533308),
 .UNSPECIFIED.);
#816=B_SPLINE_CURVE_WITH_KNOTS('',3,(#22803,#22804,#22805,#22806,#22807,
#22808,#22809,#22810,#22811,#22812,#22813,#22814,#22815,#22816,#22817,#22818,
#22819,#22820,#22821,#22822,#22823,#22824,#22825,#22826,#22827,#22828,#22829,
#22830,#22831,#22832,#22833,#22834,#22835,#22836,#22837,#22838,#22839,#22840,
#22841,#22842,#22843,#22844,#22845,#22846,#22847,#22848,#22849,#22850,#22851,
#22852,#22853,#22854,#22855,#22856,#22857,#22858,#22859,#22860,#22861,#22862,
#22863,#22864,#22865,#22866,#22867,#22868,#22869,#22870,#22871,#22872,#22873,
#22874,#22875,#22876,#22877,#22878,#22879,#22880,#22881,#22882,#22883,#22884,
#22885,#22886,#22887,#22888,#22889,#22890,#22891,#22892,#22893,#22894,#22895,
#22896,#22897,#22898,#22899,#22900,#22901,#22902,#22903,#22904,#22905,#22906,
#22907,#22908,#22909,#22910,#22911,#22912,#22913,#22914,#22915,#22916,#22917,
#22918,#22919,#22920,#22921,#22922,#22923,#22924,#22925,#22926,#22927,#22928,
#22929,#22930,#22931,#22932,#22933,#22934,#22935,#22936,#22937,#22938,#22939,
#22940,#22941,#22942,#22943,#22944,#22945,#22946,#22947,#22948,#22949,#22950,
#22951,#22952,#22953,#22954,#22955,#22956,#22957,#22958,#22959,#22960,#22961,
#22962,#22963,#22964,#22965,#22966,#22967,#22968,#22969,#22970,#22971,#22972,
#22973,#22974,#22975,#22976,#22977,#22978,#22979,#22980,#22981,#22982,#22983,
#22984,#22985,#22986,#22987,#22988,#22989,#22990,#22991,#22992,#22993,#22994,
#22995,#22996,#22997,#22998,#22999,#23000,#23001,#23002,#23003,#23004,#23005,
#23006,#23007,#23008,#23009,#23010,#23011,#23012,#23013,#23014,#23015,#23016,
#23017,#23018,#23019,#23020,#23021,#23022,#23023,#23024,#23025,#23026,#23027,
#23028,#23029,#23030,#23031,#23032,#23033,#23034,#23035,#23036,#23037,#23038,
#23039,#23040,#23041,#23042,#23043,#23044,#23045,#23046,#23047,#23048,#23049,
#23050,#23051,#23052,#23053,#23054,#23055,#23056,#23057,#23058,#23059,#23060,
#23061,#23062,#23063,#23064,#23065,#23066,#23067,#23068,#23069,#23070,#23071,
#23072,#23073,#23074,#23075,#23076,#23077,#23078,#23079,#23080,#23081,#23082,
#23083,#23084,#23085,#23086,#23087,#23088,#23089,#23090,#23091,#23092,#23093,
#23094,#23095,#23096,#23097,#23098,#23099,#23100,#23101,#23102,#23103,#23104,
#23105,#23106,#23107,#23108,#23109,#23110,#23111,#23112,#23113,#23114,#23115,
#23116,#23117,#23118,#23119,#23120,#23121,#23122,#23123,#23124,#23125,#23126,
#23127,#23128,#23129,#23130,#23131,#23132,#23133,#23134,#23135,#23136,#23137,
#23138,#23139,#23140,#23141,#23142,#23143,#23144,#23145,#23146,#23147,#23148,
#23149,#23150,#23151,#23152,#23153,#23154,#23155,#23156,#23157,#23158,#23159,
#23160,#23161,#23162,#23163,#23164,#23165,#23166,#23167,#23168,#23169,#23170,
#23171,#23172,#23173,#23174,#23175,#23176,#23177,#23178,#23179,#23180,#23181,
#23182,#23183,#23184,#23185,#23186,#23187,#23188,#23189,#23190,#23191,#23192,
#23193,#23194,#23195,#23196,#23197,#23198,#23199,#23200,#23201,#23202,#23203,
#23204,#23205,#23206,#23207,#23208,#23209,#23210,#23211,#23212,#23213,#23214,
#23215,#23216,#23217,#23218,#23219,#23220,#23221,#23222,#23223,#23224,#23225,
#23226,#23227,#23228,#23229,#23230,#23231,#23232,#23233,#23234,#23235,#23236,
#23237,#23238,#23239,#23240,#23241,#23242,#23243,#23244,#23245,#23246,#23247,
#23248,#23249,#23250,#23251,#23252,#23253,#23254,#23255,#23256,#23257,#23258,
#23259,#23260,#23261,#23262,#23263,#23264,#23265,#23266,#23267,#23268,#23269,
#23270,#23271,#23272,#23273,#23274),.UNSPECIFIED.,.F.,.F.,(4,2,2,2,2,2,
2,2,2,2,2,2,2,2,2,2,2,2,2,2,2,2,2,2,2,2,2,2,2,2,2,2,2,2,2,2,2,2,2,2,2,2,
2,2,2,2,2,2,2,2,2,2,2,2,2,2,2,2,2,2,2,2,2,2,2,2,2,2,2,2,2,2,2,2,2,2,2,2,
2,2,2,2,2,2,2,2,2,2,2,2,2,2,2,2,2,2,2,2,2,2,2,2,2,2,2,2,2,2,2,2,2,2,2,2,
2,2,2,2,2,2,2,2,2,2,2,2,2,2,2,2,2,2,2,2,2,2,2,2,2,2,2,2,2,2,2,2,2,2,2,2,
2,2,2,2,2,2,2,2,2,2,2,2,2,2,2,2,2,2,2,2,2,2,2,2,2,2,2,2,2,2,2,2,2,2,2,2,
2,2,2,2,2,2,2,2,2,2,2,2,2,2,2,2,2,2,2,2,2,2,2,2,2,2,2,2,2,2,2,2,2,2,2,2,
2,2,2,2,2,2,2,2,2,2,2,2,2,4),(-2.51391341080619,-2.46179105637164,-2.45646047624814,
-2.45239245541763,-2.45048498056078,-2.44902500250497,-2.44763380211385,
-2.44527872354363,-2.43893617240994,-2.39141999370173,-2.37440683007866,
-2.35421939631866,-2.35143874649784,-2.35053108790662,-2.34977064764138,
-2.34895871525468,-2.34791023253071,-2.34621361432944,-2.33681950298222,
-2.33334898385338,-2.32150584311304,-2.27609323468591,-2.26253190319611,
-2.25698556062711,-2.25278659141177,-2.25085436174359,-2.24939073407475,
-2.24800742062708,-2.24569302364923,-2.23961207572437,-2.18732651562046,
-2.15666978477067,-2.15222637690514,-2.15083815367759,-2.15007715390696,
-2.14926570876715,-2.14822215420747,-2.14605451854881,-2.13049721943133,
-2.0759995059429,-2.06266279375167,-2.05718217169216,-2.0530229400672,-2.05109815612437,
-2.04963563271675,-2.0482499910716,-2.04592361493768,-2.03976769426212,
-1.98854620835413,-1.95419984125791,-1.95177623722019,-1.95068398276447,
-1.94986628644607,-1.94896953730749,-1.94749336834567,-1.9437121983998,
-1.8891145568725,-1.85787475887526,-1.85341249799428,-1.85143189730792,
-1.84996054334067,-1.84859078761762,-1.84671278233194,-1.84197255977692,
-1.83982448374706,-1.79110790555178,-1.76763721775764,-1.7582844284931,
-1.75290927375168,-1.75142339841012,-1.75052449763613,-1.74970750080907,
-1.74863847358257,-1.74627737467739,-1.71795847904892,-1.66650674285726,
-1.65542918680646,-1.65264275372697,-1.6510015031532,-1.64955323703508,
-1.64774577847719,-1.6449501826694,-1.64007628583328,-1.59189649948304,
-1.56805296809368,-1.55861239011388,-1.55320103597566,-1.55171167186411,
-1.55081199953163,-1.5499952504192,-1.54892781446164,-1.54657527710547,
-1.52075940821706,-1.49122308519841,-1.4605940037698,-1.45461941460919,
-1.45239318426608,-1.45087478567476,-1.44939701878785,-1.44762559290574,
-1.44323236780215,-1.44043069598607,-1.39183491897399,-1.36827757995644,
-1.358904164305,-1.35352041311632,-1.35203365696884,-1.35113453176544,-1.35031754991976,
-1.34924883499607,-1.3468895942435,-1.31959018242947,-1.28267587884756,
-1.25727988501442,-1.25414780973755,-1.25225844314356,-1.25079624427474,
-1.24921648202506,-1.24670710396124,-1.23851607656586,-1.22536318988242,
-1.17234525530424,-1.15505807771875,-1.15305816416419,-1.15203397286243,
-1.15127713800862,-1.15043982362538,-1.14923746533013,-1.14616637531344,
-1.13105285439884,-1.10103987751716,-1.05816979468867,-1.05430245608908,
-1.052433558414,-1.05097846103737,-1.04937312003295,-1.04674904577157,-1.03746901211778,
-1.02187699205744,-0.991434534160672,-0.972458603521345,-0.955369730963324,
-0.953155366604645,-0.952113862259828,-0.951300595898236,-0.950386668261615,
-0.948833788722708,-0.942724154853327,-0.931526244234803,-0.901683171377436,
-0.858486132769825,-0.854624265048591,-0.85275649199072,-0.851301589884239,
-0.849695773340386,-0.847069353598386,-0.837764840218069,-0.822115738278513,
-0.791628926051631,-0.755804523715857,-0.753510010816469,-0.752453308612617,
-0.75163802963243,-0.750732623601054,-0.749217922912605,-0.743538833003712,
-0.733440720432717,-0.706869236547874,-0.662549343293129,-0.658379109069224,
-0.655141656053671,-0.653221349920203,-0.651754195660049,-0.650187604366442,
-0.647737995076812,-0.640067070216302,-0.585133087501146,-0.556159397042375,
-0.55379800434309,-0.552728805350092,-0.551911664501675,-0.551012583969879,
-0.549526376038066,-0.544149575082301,-0.53479471213359,-0.511317746976424,
-0.462636720749346,-0.460430115401939,-0.455729234910676,-0.453857713395475,
-0.452489465921522,-0.451016678662117,-0.449028796616842,-0.444629193742244,
-0.438693255864835,-0.423772615512908,-0.373589266652928,-0.356206879713412,
-0.354204538545188,-0.35317969231942,-0.352422660527237,-0.351585447213904,
-0.350383794618626,-0.347467516921108,-0.312517156781276,-0.277940832295828,
-0.272439533961448,-0.258198572823757,-0.255335144968495,-0.253506498620078,
-0.25205585472538,-0.250427366546338,-0.247871253947722,-0.238625569207456,
-0.223047109894977,-0.190779511911257,-0.185486372018215,-0.156726573020153,
-0.154364801535007,-0.153295506971903,-0.15247832517276,-0.151579234129652,
-0.150645996444047,-0.147597909679877,-0.11342651764459,-0.100055177249121,
-0.0874958998967663,-0.0595261843350611,-0.0557308786672539,-0.0538760753636376,
-0.0524225515501624,-0.0508093135378623,-0.0491448044903754,-0.0466820551587498,
-0.037302115107823,-0.000592337695832264),.UNSPECIFIED.);
#817=B_SPLINE_CURVE_WITH_KNOTS('',3,(#23276,#23277,#23278,#23279,#23280,
#23281,#23282,#23283,#23284,#23285,#23286,#23287,#23288,#23289,#23290,#23291,
#23292,#23293,#23294,#23295,#23296,#23297,#23298,#23299,#23300,#23301,#23302,
#23303,#23304,#23305,#23306,#23307,#23308,#23309,#23310,#23311,#23312,#23313,
#23314,#23315,#23316,#23317,#23318,#23319,#23320,#23321,#23322,#23323,#23324,
#23325,#23326,#23327,#23328,#23329,#23330,#23331,#23332,#23333,#23334,#23335,
#23336,#23337,#23338,#23339,#23340,#23341,#23342,#23343,#23344,#23345,#23346,
#23347,#23348,#23349,#23350,#23351,#23352,#23353,#23354,#23355,#23356,#23357,
#23358,#23359,#23360,#23361,#23362,#23363,#23364,#23365,#23366,#23367,#23368,
#23369,#23370,#23371,#23372,#23373,#23374,#23375,#23376,#23377,#23378,#23379,
#23380,#23381,#23382,#23383,#23384,#23385,#23386,#23387,#23388,#23389,#23390,
#23391,#23392,#23393,#23394,#23395,#23396,#23397,#23398,#23399,#23400,#23401,
#23402,#23403,#23404,#23405,#23406,#23407,#23408,#23409,#23410,#23411,#23412,
#23413,#23414,#23415,#23416,#23417,#23418,#23419,#23420,#23421,#23422,#23423,
#23424,#23425,#23426,#23427,#23428,#23429,#23430,#23431,#23432,#23433,#23434,
#23435,#23436,#23437,#23438,#23439,#23440,#23441,#23442,#23443,#23444,#23445,
#23446,#23447,#23448,#23449,#23450,#23451,#23452,#23453,#23454,#23455,#23456,
#23457,#23458,#23459,#23460,#23461,#23462,#23463,#23464,#23465,#23466,#23467,
#23468,#23469,#23470,#23471,#23472,#23473,#23474,#23475,#23476,#23477,#23478,
#23479,#23480,#23481,#23482,#23483,#23484,#23485,#23486,#23487,#23488,#23489,
#23490,#23491,#23492,#23493,#23494,#23495,#23496,#23497,#23498,#23499,#23500,
#23501,#23502,#23503,#23504,#23505,#23506,#23507,#23508,#23509,#23510,#23511,
#23512,#23513,#23514,#23515,#23516,#23517,#23518,#23519,#23520,#23521,#23522,
#23523,#23524,#23525,#23526,#23527,#23528,#23529,#23530,#23531,#23532,#23533,
#23534,#23535,#23536,#23537,#23538,#23539,#23540,#23541,#23542,#23543,#23544,
#23545,#23546,#23547,#23548,#23549,#23550,#23551,#23552,#23553,#23554,#23555,
#23556,#23557,#23558,#23559,#23560,#23561,#23562,#23563,#23564,#23565,#23566,
#23567,#23568,#23569,#23570,#23571,#23572,#23573,#23574,#23575,#23576,#23577,
#23578,#23579,#23580,#23581,#23582,#23583,#23584,#23585,#23586,#23587,#23588,
#23589,#23590,#23591,#23592,#23593,#23594,#23595,#23596,#23597,#23598,#23599,
#23600,#23601,#23602,#23603,#23604,#23605,#23606,#23607,#23608,#23609,#23610,
#23611,#23612,#23613,#23614,#23615,#23616,#23617,#23618,#23619,#23620,#23621,
#23622,#23623,#23624,#23625,#23626,#23627,#23628,#23629,#23630,#23631,#23632,
#23633,#23634,#23635,#23636,#23637,#23638,#23639,#23640,#23641,#23642,#23643,
#23644,#23645,#23646,#23647,#23648,#23649,#23650,#23651,#23652,#23653,#23654,
#23655,#23656,#23657,#23658,#23659,#23660,#23661,#23662,#23663,#23664,#23665,
#23666,#23667,#23668,#23669,#23670,#23671,#23672,#23673,#23674,#23675,#23676,
#23677,#23678,#23679,#23680,#23681,#23682,#23683,#23684,#23685,#23686,#23687,
#23688,#23689,#23690,#23691,#23692,#23693,#23694,#23695,#23696,#23697,#23698,
#23699,#23700,#23701,#23702,#23703,#23704,#23705,#23706,#23707,#23708,#23709,
#23710,#23711,#23712,#23713,#23714,#23715,#23716,#23717,#23718,#23719,#23720,
#23721,#23722,#23723,#23724,#23725,#23726,#23727,#23728,#23729,#23730,#23731,
#23732,#23733,#23734,#23735,#23736,#23737,#23738,#23739,#23740,#23741,#23742,
#23743,#23744,#23745,#23746,#23747,#23748,#23749),.UNSPECIFIED.,.F.,.F.,
(4,2,2,2,2,2,2,2,2,2,2,2,2,2,2,2,2,2,2,2,2,2,2,2,2,2,2,2,2,2,2,2,2,2,2,
2,2,2,2,2,2,2,2,2,2,2,2,2,2,2,2,2,2,2,2,2,2,2,2,2,2,2,2,2,2,2,2,2,2,2,2,
2,2,2,2,2,2,2,2,2,2,2,2,2,2,2,2,2,2,2,2,2,2,2,2,2,2,2,2,2,2,2,2,2,2,2,2,
2,2,2,2,2,2,2,2,2,2,2,2,2,2,2,2,2,2,2,2,2,2,2,2,2,2,2,2,2,2,2,2,2,2,2,2,
2,2,2,2,2,2,2,2,2,2,2,2,2,2,2,2,2,2,2,2,2,2,2,2,2,2,2,2,2,2,2,2,2,2,2,2,
2,2,2,2,2,2,2,2,2,2,2,2,2,2,2,2,2,2,2,2,2,2,2,2,2,2,2,2,2,2,2,2,2,2,2,2,
2,2,2,2,2,2,2,2,2,2,2,2,2,2,2,2,2,2,2,2,2,4),(-2.51356825422661,-2.47394218197505,
-2.47035764364301,-2.46856460930196,-2.46746334599422,-2.46644534921851,
-2.46571328584953,-2.46491694785596,-2.46349574152554,-2.45920389941625,
-2.42128676523049,-2.40237491188082,-2.37511750803352,-2.36979029470891,
-2.36814327223351,-2.36654227980619,-2.36508628863625,-2.36320945561377,
-2.35930105980408,-2.32289862526151,-2.28907209137147,-2.27592950555056,
-2.27140987911008,-2.26831759641163,-2.26738442327779,-2.26648543088389,
-2.26566838390759,-2.26459933535138,-2.26223836622955,-2.23422475439631,
-2.19372428850427,-2.17337512531339,-2.16947772407708,-2.16757294700741,
-2.16611318093781,-2.16472078445636,-2.16236025783666,-2.1559841076186,
-2.1097009288288,-2.07387810337846,-2.07066336847685,-2.06829608724467,
-2.06720164898327,-2.06638356620263,-2.06548769629021,-2.06401569760017,
-2.05932580979843,-1.99590980774065,-1.98049688165391,-1.97129367007065,
-1.96867751474784,-1.96707409719654,-1.96561882973147,-1.96374703638707,
-1.95986403677172,-1.92670244367806,-1.87499047400447,-1.86939589912413,
-1.86788903030803,-1.86698537756707,-1.86616963333975,-1.86510963264811,
-1.86279749107987,-1.82812447199477,-1.79728582954517,-1.78115424267524,
-1.77164224225226,-1.76899549189785,-1.76738512136143,-1.76593120010981,
-1.76407176928262,-1.76025240985229,-1.75656512302494,-1.70816707242092,
-1.68446523734727,-1.67505730941136,-1.66965913119662,-1.66817086172729,
-1.66727132983777,-1.66645433909318,-1.66538609431153,-1.6630298117515,
-1.63680898624427,-1.58401010853708,-1.57225570299218,-1.56941475437926,
-1.56776125692786,-1.56631416819616,-1.56452374344591,-1.56178359544932,
-1.55679881985351,-1.5086302796843,-1.4847696108149,-1.47532438259311,-1.46991086762184,
-1.46842113896675,-1.46752129367456,-1.46670442100115,-1.46563686821688,
-1.46328425094685,-1.43193736664937,-1.42669060984774,-1.39869983371182,
-1.38199428027506,-1.37224012200973,-1.36957014727232,-1.36795455237303,
-1.36650163688166,-1.36465136212075,-1.36087848773287,-1.31380889220081,
-1.27512274021726,-1.2717908044124,-1.26933268834605,-1.26823396891744,
-1.26741516102899,-1.26652106997336,-1.26505733380767,-1.26043511541086,
-1.25725185627739,-1.242305402245,-1.19354591972506,-1.17394496003048,-1.17079245707546,
-1.16889693523588,-1.16743362307259,-1.16585627364041,-1.16335844265841,
-1.1552722249205,-1.14234597843094,-1.09189387336379,-1.08656929456985,
-1.07157226112248,-1.0694239703701,-1.06838407636168,-1.06757284006429,
-1.06664716301918,-1.06504178248724,-1.05828655798903,-1.0453447488131,
-1.02040556202218,-0.974696250056967,-0.970884046106176,-0.969025901865425,
-0.967571990442836,-0.965960610073872,-0.963309858028534,-0.953758560199666,
-0.937532620694539,-0.906590565463561,-0.872113286393838,-0.869825951878624,
-0.868754255298571,-0.867936692823698,-0.867038745940872,-0.86555777966523,
-0.860235373081425,-0.851011934353765,-0.828091080754851,-0.778598776251994,
-0.772342415381426,-0.769999493465719,-0.768610404681683,-0.767148934905921,
-0.765233361386714,-0.761124413032057,-0.723669009395699,-0.683510118705204,
-0.671886725918484,-0.669901835467375,-0.668881545756867,-0.668072073851384,
-0.667133077089268,-0.665467273505235,-0.657874530018301,-0.608920538508744,
-0.605638840734015,-0.575273825582681,-0.571426086081437,-0.569560977684702,
-0.568106278805076,-0.566498780814453,-0.563865274570097,-0.554490583410462,
-0.538678736710341,-0.478971156066348,-0.477469801850242,-0.47142031050116,
-0.469818005080321,-0.468883558823451,-0.468081159595123,-0.467058149499422,
-0.464994804736573,-0.44689685800373,-0.40601053555134,-0.37547381796058,
-0.371628188459321,-0.369763309381278,-0.368308432541423,-0.368305850660745,
-0.36830327472084,-0.368300704708948,-0.368298140574993,-0.366719169944355,
-0.364178851443436,-0.361154211920972,-0.355288743722237,-0.340618973668368,
-0.304955982196178,-0.283209580502759,-0.272292806438492,-0.270515768706503,
-0.269454487671194,-0.268638384959143,-0.267735008714936,-0.266230061381181,
-0.260658779533736,-0.208943657690746,-0.175765854248469,-0.171883522994864,
-0.170011501897731,-0.168555811528997,-0.167200257655818,-0.16497475149422,
-0.158580379106579,-0.14903515131864,-0.127500661488512,-0.0983596945928476,
-0.0731308756767082,-0.0707796542191637,-0.0697122651376716,-0.0688953219904742,
-0.0679951803681352,-0.066504506316771,-0.0610826183693228,-0.014973403458735,
-0.00059288335019173),.UNSPECIFIED.);
#818=B_SPLINE_CURVE_WITH_KNOTS('',3,(#23751,#23752,#23753,#23754,#23755,
#23756,#23757,#23758,#23759,#23760,#23761,#23762,#23763,#23764,#23765,#23766,
#23767,#23768,#23769,#23770,#23771,#23772,#23773,#23774,#23775,#23776,#23777,
#23778,#23779,#23780,#23781,#23782,#23783,#23784,#23785,#23786,#23787,#23788,
#23789,#23790,#23791,#23792,#23793,#23794,#23795,#23796,#23797,#23798,#23799,
#23800,#23801,#23802,#23803,#23804,#23805,#23806,#23807,#23808,#23809,#23810,
#23811,#23812,#23813,#23814,#23815,#23816,#23817,#23818,#23819,#23820,#23821,
#23822,#23823,#23824,#23825,#23826,#23827,#23828,#23829,#23830,#23831,#23832,
#23833,#23834,#23835,#23836,#23837,#23838,#23839,#23840,#23841,#23842,#23843,
#23844,#23845,#23846,#23847,#23848,#23849,#23850,#23851,#23852,#23853,#23854,
#23855,#23856,#23857,#23858,#23859,#23860,#23861,#23862,#23863,#23864,#23865,
#23866,#23867,#23868,#23869,#23870,#23871,#23872,#23873,#23874,#23875,#23876,
#23877,#23878,#23879,#23880,#23881,#23882,#23883,#23884,#23885,#23886,#23887,
#23888,#23889,#23890,#23891,#23892,#23893,#23894,#23895,#23896,#23897,#23898,
#23899,#23900,#23901,#23902,#23903,#23904,#23905,#23906,#23907,#23908,#23909,
#23910,#23911,#23912,#23913,#23914,#23915,#23916,#23917,#23918,#23919,#23920,
#23921,#23922,#23923,#23924,#23925,#23926,#23927,#23928,#23929,#23930,#23931,
#23932,#23933,#23934,#23935,#23936,#23937,#23938,#23939,#23940,#23941,#23942,
#23943,#23944,#23945,#23946,#23947,#23948,#23949,#23950,#23951,#23952,#23953,
#23954,#23955,#23956,#23957,#23958,#23959,#23960,#23961,#23962,#23963,#23964,
#23965,#23966,#23967,#23968,#23969,#23970,#23971,#23972,#23973,#23974,#23975,
#23976,#23977,#23978,#23979,#23980,#23981,#23982,#23983,#23984,#23985,#23986,
#23987,#23988,#23989,#23990,#23991,#23992,#23993,#23994,#23995,#23996,#23997,
#23998,#23999,#24000,#24001,#24002,#24003,#24004,#24005,#24006,#24007,#24008,
#24009,#24010,#24011,#24012,#24013,#24014,#24015,#24016,#24017,#24018,#24019,
#24020,#24021,#24022,#24023,#24024,#24025,#24026,#24027,#24028,#24029,#24030,
#24031,#24032,#24033,#24034,#24035,#24036,#24037,#24038,#24039,#24040,#24041,
#24042,#24043,#24044,#24045,#24046,#24047,#24048,#24049,#24050,#24051,#24052,
#24053,#24054,#24055,#24056,#24057,#24058,#24059,#24060,#24061,#24062,#24063,
#24064,#24065,#24066,#24067,#24068,#24069,#24070,#24071,#24072,#24073,#24074,
#24075,#24076,#24077,#24078,#24079,#24080,#24081,#24082,#24083,#24084,#24085,
#24086,#24087,#24088,#24089,#24090,#24091,#24092,#24093,#24094,#24095,#24096,
#24097,#24098,#24099,#24100,#24101,#24102,#24103,#24104,#24105,#24106,#24107,
#24108,#24109,#24110,#24111,#24112,#24113,#24114,#24115,#24116,#24117,#24118,
#24119,#24120,#24121,#24122,#24123,#24124,#24125,#24126,#24127,#24128,#24129,
#24130,#24131,#24132,#24133,#24134,#24135,#24136,#24137,#24138,#24139,#24140,
#24141,#24142,#24143,#24144,#24145,#24146,#24147,#24148,#24149,#24150,#24151,
#24152,#24153,#24154,#24155,#24156,#24157,#24158,#24159,#24160,#24161,#24162,
#24163,#24164,#24165,#24166,#24167,#24168,#24169,#24170,#24171,#24172,#24173,
#24174,#24175,#24176,#24177,#24178,#24179,#24180,#24181,#24182,#24183,#24184,
#24185,#24186,#24187,#24188,#24189,#24190,#24191,#24192,#24193,#24194,#24195,
#24196,#24197,#24198,#24199,#24200,#24201,#24202,#24203,#24204,#24205,#24206,
#24207,#24208,#24209,#24210,#24211,#24212,#24213,#24214,#24215,#24216,#24217,
#24218,#24219,#24220,#24221,#24222,#24223,#24224,#24225,#24226,#24227,#24228,
#24229,#24230,#24231,#24232,#24233,#24234,#24235,#24236,#24237,#24238,#24239,
#24240,#24241,#24242,#24243,#24244,#24245,#24246,#24247,#24248,#24249,#24250,
#24251,#24252,#24253,#24254,#24255,#24256,#24257,#24258,#24259,#24260,#24261,
#24262,#24263,#24264,#24265,#24266,#24267,#24268,#24269,#24270,#24271,#24272,
#24273,#24274,#24275,#24276,#24277,#24278,#24279,#24280,#24281,#24282,#24283,
#24284,#24285,#24286,#24287,#24288,#24289,#24290,#24291,#24292),
 .UNSPECIFIED.,.F.,.F.,(4,2,2,2,2,2,2,2,2,2,2,2,2,2,2,2,2,2,2,2,2,2,2,2,
2,2,2,2,2,2,2,2,2,2,2,2,2,2,2,2,2,2,2,2,2,2,2,2,2,2,2,2,2,2,2,2,2,2,2,2,
2,2,2,2,2,2,2,2,2,2,2,2,2,2,2,2,2,2,2,2,2,2,2,2,2,2,2,2,2,2,2,2,2,2,2,2,
2,2,2,2,2,2,2,2,2,2,2,2,2,2,2,2,2,2,2,2,2,2,2,2,2,2,2,2,2,2,2,2,2,2,2,2,
2,2,2,2,2,2,2,2,2,2,2,2,2,2,2,2,2,2,2,2,2,2,2,2,2,2,2,2,2,2,2,2,2,2,2,2,
2,2,2,2,2,2,2,2,2,2,2,2,2,2,2,2,2,2,2,2,2,2,2,2,2,2,2,2,2,2,2,2,2,2,2,2,
2,2,2,2,2,2,2,2,2,2,2,2,2,2,2,2,2,2,2,2,2,2,2,2,2,2,2,2,2,2,2,2,2,2,2,2,
2,2,2,2,2,2,2,2,2,2,2,2,2,2,2,2,2,2,2,2,2,2,2,2,2,2,2,2,2,2,4),(-2.51318058552356,
-2.49534092889612,-2.48754131701959,-2.48526379985214,-2.48367623155305,
-2.48232029791119,-2.480869105159,-2.47902670392536,-2.47611614204028,-2.46110366271849,
-2.45719216229731,-2.4482463481611,-2.41465704566012,-2.38634278217323,
-2.38383158492869,-2.38272372698508,-2.3819039748108,-2.38112477548954,
-2.37978800445029,-2.37609803990247,-2.37524392204819,-2.33016470889085,
-2.30324810779577,-2.29308957097751,-2.28637664838568,-2.28405597765139,
-2.28270176040486,-2.28124666331771,-2.27937141888137,-2.27546792034526,
-2.23801034675361,-2.19055472552387,-2.18506878635465,-2.18357266925265,
-2.18267171609894,-2.18185577671024,-2.18079202416924,-2.17900509632798,
-2.16786519214015,-2.16437661174598,-2.15434279719327,-2.1132390026198,
-2.09696724467837,-2.09065782633207,-2.08746979911785,-2.08480910481439,
-2.08320752016455,-2.0832054331407,-2.08320333982577,-2.08320124020769,
-2.08319913426817,-2.08319702195549,-2.08319490324864,-2.08319277812535,
-2.08319064655953,-2.08318850854315,-2.08318636404106,-2.0831842130326,
-2.0831820555194,-2.08317989145589,-2.08317772080522,-2.08317554354486,
-2.08317335968841,-2.08317116920818,-2.08316897204192,-2.08316676816492,
-2.08316455755618,-2.0831623402143,-2.08316011610567,-2.08315788522021,
-2.08315564752342,-2.08315340300327,-2.08315115160638,-2.08314889327832,
-2.08314662805286,-2.08314435592246,-2.08169224444141,-2.07984155320643,
-2.07606278056042,-2.0292704157726,-2.00172461431719,-1.99133372423346,
-1.98553967116006,-1.98401508285565,-1.98310780279515,-1.98229361223924,
-1.9812419748891,-1.97897240728259,-1.94202195080193,-1.91196687912686,
-1.89681340039215,-1.88772415087907,-1.88512020222295,-1.88351995625251,
-1.88206473245219,-1.88018901309947,-1.87628339030214,-1.83776640312309,
-1.79131134701107,-1.78587434794294,-1.78438285874438,-1.78348291167112,
-1.78266662643691,-1.78160074787566,-1.77980663951805,-1.76851896269361,
-1.74301947834166,-1.71275854981441,-1.69735044221196,-1.68815014341382,
-1.68553483348406,-1.6839319377448,-1.68247714628894,-1.68060596857258,
-1.67672425828234,-1.64354873583983,-1.59182459669076,-1.58627733888035,
-1.58477522626193,-1.58387282123464,-1.58305708060438,-1.58199559583834,
-1.58021677907269,-1.56924845026757,-1.56766416131119,-1.56144581662258,
-1.55533910553312,-1.5154984543267,-1.49850617663551,-1.48863362841935,
-1.48595324239052,-1.4843357298402,-1.48288388999399,-1.48103881481722,
-1.47812038107284,-1.46298891176632,-1.45911271195835,-1.40502627474109,
-1.3931350771096,-1.38676476843716,-1.38519031651931,-1.38427171525415,
-1.3834596094917,-1.38240918883224,-1.38020604855366,-1.3634991266006,-1.3161611418744,
-1.29893642924169,-1.28896746900223,-1.28627799879721,-1.28465837988368,
-1.28320679838385,-1.28136498019625,-1.2784574540511,-1.26350586866066,
-1.2595644555537,-1.25707920268081,-1.19818496567701,-1.18769553955751,
-1.1859402499901,-1.18488554711709,-1.18407060456433,-1.18316425345828,
-1.18164509823361,-1.17591641972404,-1.16569378427659,-1.13866659953425,
-1.09500224789981,-1.09139448151434,-1.08743691617553,-1.0855708355205,
-1.08411214328927,-1.0825215256938,-1.07996298772627,-1.07131957188705,
-1.05717343852155,-0.997553406806989,-0.987875418513911,-0.986162710283493,
-0.985120517427023,-0.984307130637433,-0.983393530613857,-0.981842248098768,
-0.975751869820542,-0.96460444933425,-0.934845820278877,-0.89147750456786,
-0.88762127482329,-0.885754554977527,-0.884299722786788,-0.88269322044028,
-0.880063945258876,-0.870731355925798,-0.855017281231994,-0.824478255646457,
-0.788802633804009,-0.786506373492071,-0.785449312819604,-0.784633951202238,
-0.783728664988438,-0.782214624289928,-0.776543228298057,-0.766464519659003,
-0.739968165316298,-0.695543863200072,-0.691719000764627,-0.687902830832579,
-0.686044019862492,-0.684590160279556,-0.682979424836922,-0.680331081846468,
-0.670802852433895,-0.65463063542025,-0.623732438967976,-0.589139203738715,
-0.586852593937324,-0.585781106660395,-0.584963645398563,-0.584065746903173,
-0.582584728297276,-0.577260750486654,-0.568033153939062,-0.545093120873518,
-0.495637588274032,-0.489380288351041,-0.487037363823574,-0.485648373281111,
-0.484187079863851,-0.482271858869356,-0.478164135434446,-0.440742043267341,
-0.401882958403301,-0.38902711823129,-0.386987443148679,-0.385955469221269,
-0.385167502629641,-0.384263583410721,-0.383303794109438,-0.381851407165306,
-0.379180597538454,-0.354647661989461,-0.322872841020084,-0.292366122780154,
-0.288521935163989,-0.286657595045587,-0.2852030665876,-0.283595320016953,
-0.280960410859299,-0.271570321804609,-0.255722155692761,-0.225827442850909,
-0.213778914816316,-0.189793851315745,-0.187453506656475,-0.186388247083305,
-0.185588426080104,-0.184710696221019,-0.183309708626243,-0.181624394564604,
-0.178335755906451,-0.170007143365875,-0.13587047045507,-0.0927143190723946,
-0.0888514489127676,-0.0869834940039257,-0.0855285859264952,-0.083922900606705,
-0.0812970083287391,-0.0719975956823138,-0.0563602581642413,-0.000592940430143267),
 .UNSPECIFIED.);
#819=B_SPLINE_CURVE_WITH_KNOTS('',3,(#24294,#24295,#24296,#24297,#24298,
#24299,#24300,#24301,#24302,#24303,#24304,#24305,#24306,#24307,#24308,#24309,
#24310,#24311,#24312,#24313,#24314,#24315,#24316,#24317,#24318,#24319,#24320,
#24321,#24322,#24323,#24324,#24325,#24326,#24327,#24328,#24329,#24330,#24331,
#24332,#24333,#24334,#24335,#24336,#24337,#24338,#24339,#24340,#24341,#24342,
#24343,#24344,#24345,#24346,#24347,#24348,#24349,#24350,#24351,#24352,#24353,
#24354,#24355,#24356,#24357,#24358,#24359,#24360,#24361,#24362,#24363,#24364,
#24365,#24366,#24367,#24368,#24369,#24370,#24371,#24372,#24373,#24374,#24375,
#24376,#24377,#24378,#24379,#24380,#24381,#24382,#24383,#24384,#24385,#24386,
#24387,#24388,#24389,#24390,#24391,#24392,#24393,#24394,#24395,#24396,#24397,
#24398,#24399,#24400,#24401,#24402,#24403,#24404,#24405,#24406,#24407,#24408,
#24409,#24410,#24411,#24412,#24413,#24414,#24415,#24416,#24417,#24418,#24419,
#24420,#24421,#24422,#24423,#24424,#24425,#24426,#24427,#24428,#24429,#24430,
#24431,#24432,#24433,#24434,#24435,#24436,#24437,#24438,#24439,#24440,#24441,
#24442,#24443,#24444,#24445,#24446,#24447,#24448,#24449,#24450,#24451,#24452,
#24453,#24454,#24455,#24456,#24457,#24458,#24459,#24460,#24461,#24462,#24463,
#24464,#24465,#24466,#24467,#24468,#24469,#24470,#24471,#24472,#24473,#24474,
#24475,#24476,#24477,#24478,#24479,#24480,#24481,#24482,#24483),
 .UNSPECIFIED.,.F.,.F.,(4,3,3,3,3,3,3,3,3,3,3,3,3,3,3,3,3,3,3,3,3,3,3,3,
3,3,3,3,3,3,3,3,3,3,3,3,3,3,3,3,3,3,3,3,3,3,3,3,3,3,3,3,3,3,3,3,3,3,3,3,
3,3,3,4),(109.955742875643,110.100021482593,110.17360629996,110.278552114824,
110.383340179823,110.488004710464,110.592603218256,110.697171287668,110.801744459001,
110.906428414068,111.011173477469,111.116101323929,111.17228716832,111.277232983184,
111.382021048183,111.486685578824,111.591284086616,111.695852156028,111.80042532736,
111.905109282428,112.009854345828,112.114782192288,112.170968036681,112.275913851545,
112.380701916544,112.485366447186,112.589964954977,112.694533024389,112.799106195722,
112.90379015079,113.00853521419,113.113463060651,113.169648905042,113.274594719906,
113.379382784905,113.484047315546,113.588645823338,113.69321389275,113.797787064082,
113.90247101915,114.00721608255,114.112143929011,114.168329773403,114.273275588267,
114.378063653266,114.482728183907,114.587326691699,114.691894761111,114.796467932443,
114.90115188751,115.005896950911,115.110824797371,115.167010641763,115.271956456627,
115.376744521626,115.481409052267,115.586007560059,115.69057562947,115.795148800803,
115.89983275587,116.004577819271,116.109505665731,116.165691510124,116.238928182823),
 .UNSPECIFIED.);
#820=B_SPLINE_CURVE_WITH_KNOTS('',3,(#24485,#24486,#24487,#24488,#24489,
#24490,#24491,#24492,#24493,#24494,#24495,#24496,#24497,#24498,#24499,#24500,
#24501,#24502,#24503,#24504,#24505,#24506,#24507,#24508,#24509,#24510,#24511,
#24512,#24513,#24514,#24515,#24516,#24517,#24518,#24519,#24520,#24521,#24522,
#24523,#24524,#24525,#24526,#24527,#24528,#24529,#24530,#24531,#24532,#24533,
#24534,#24535,#24536,#24537,#24538,#24539,#24540,#24541,#24542,#24543,#24544,
#24545,#24546,#24547,#24548,#24549,#24550,#24551,#24552,#24553,#24554,#24555,
#24556,#24557,#24558,#24559,#24560,#24561,#24562,#24563,#24564,#24565,#24566,
#24567,#24568,#24569,#24570,#24571,#24572,#24573,#24574,#24575,#24576,#24577,
#24578,#24579,#24580,#24581,#24582,#24583,#24584,#24585,#24586,#24587,#24588,
#24589,#24590,#24591,#24592,#24593,#24594,#24595,#24596,#24597,#24598,#24599,
#24600,#24601,#24602,#24603,#24604,#24605,#24606,#24607,#24608,#24609,#24610,
#24611,#24612,#24613,#24614,#24615,#24616,#24617,#24618,#24619,#24620,#24621,
#24622,#24623,#24624,#24625,#24626,#24627,#24628,#24629,#24630,#24631,#24632,
#24633,#24634,#24635,#24636,#24637,#24638,#24639,#24640,#24641,#24642,#24643,
#24644,#24645,#24646,#24647,#24648,#24649,#24650,#24651,#24652,#24653,#24654,
#24655,#24656,#24657,#24658,#24659,#24660,#24661,#24662,#24663,#24664,#24665,
#24666,#24667,#24668,#24669,#24670,#24671,#24672,#24673,#24674,#24675,#24676,
#24677,#24678,#24679,#24680,#24681,#24682,#24683,#24684,#24685,#24686,#24687,
#24688,#24689,#24690,#24691,#24692,#24693,#24694,#24695,#24696,#24697,#24698,
#24699,#24700,#24701,#24702,#24703,#24704,#24705,#24706,#24707,#24708,#24709,
#24710,#24711,#24712,#24713,#24714,#24715,#24716,#24717,#24718,#24719,#24720,
#24721,#24722,#24723,#24724,#24725,#24726,#24727,#24728,#24729,#24730,#24731,
#24732,#24733,#24734,#24735,#24736,#24737,#24738,#24739,#24740,#24741,#24742,
#24743,#24744,#24745,#24746,#24747,#24748,#24749,#24750,#24751,#24752,#24753,
#24754,#24755,#24756,#24757,#24758,#24759,#24760,#24761,#24762,#24763,#24764,
#24765,#24766,#24767,#24768,#24769,#24770,#24771,#24772,#24773,#24774,#24775,
#24776,#24777,#24778,#24779,#24780,#24781,#24782,#24783,#24784,#24785,#24786,
#24787,#24788,#24789,#24790,#24791,#24792,#24793,#24794,#24795,#24796,#24797,
#24798,#24799,#24800,#24801,#24802,#24803,#24804,#24805,#24806,#24807,#24808,
#24809,#24810,#24811,#24812,#24813,#24814,#24815,#24816,#24817,#24818,#24819,
#24820,#24821,#24822,#24823,#24824,#24825,#24826,#24827,#24828,#24829,#24830,
#24831,#24832,#24833,#24834,#24835,#24836,#24837,#24838,#24839,#24840,#24841,
#24842,#24843,#24844,#24845,#24846,#24847,#24848,#24849,#24850,#24851,#24852,
#24853,#24854,#24855,#24856,#24857,#24858,#24859,#24860,#24861,#24862,#24863,
#24864,#24865,#24866,#24867,#24868,#24869,#24870,#24871,#24872,#24873,#24874,
#24875,#24876,#24877,#24878,#24879,#24880,#24881,#24882,#24883,#24884,#24885,
#24886,#24887,#24888,#24889,#24890,#24891,#24892,#24893,#24894,#24895,#24896,
#24897,#24898,#24899,#24900,#24901,#24902,#24903,#24904,#24905,#24906,#24907,
#24908,#24909,#24910,#24911,#24912,#24913,#24914,#24915,#24916,#24917,#24918,
#24919,#24920,#24921,#24922,#24923,#24924,#24925,#24926,#24927,#24928,#24929,
#24930,#24931,#24932,#24933,#24934,#24935,#24936,#24937,#24938,#24939,#24940,
#24941,#24942,#24943,#24944),.UNSPECIFIED.,.F.,.F.,(4,2,2,2,2,2,2,2,2,2,
2,2,2,2,2,2,2,2,2,2,2,2,2,2,2,2,2,2,2,2,2,2,2,2,2,2,2,2,2,2,2,2,2,2,2,2,
2,2,2,2,2,2,2,2,2,2,2,2,2,2,2,2,2,2,2,2,2,2,2,2,2,2,2,2,2,2,2,2,2,2,2,2,
2,2,2,2,2,2,2,2,2,2,2,2,2,2,2,2,2,2,2,2,2,2,2,2,2,2,2,2,2,2,2,2,2,2,2,2,
2,2,2,2,2,2,2,2,2,2,2,2,2,2,2,2,2,2,2,2,2,2,2,2,2,2,2,2,2,2,2,2,2,2,2,2,
2,2,2,2,2,2,2,2,2,2,2,2,2,2,2,2,2,2,2,2,2,2,2,2,2,2,2,2,2,2,2,2,2,2,2,2,
2,2,2,2,2,2,2,2,2,2,2,2,2,2,2,2,2,2,2,2,2,2,2,2,2,2,2,2,2,2,2,2,2,2,2,2,
2,2,2,4),(-2.51385589383474,-2.4728953440402,-2.46356778281143,-2.46111336745769,
-2.45945262149794,-2.45784219742815,-2.45638892076038,-2.45453127252685,
-2.45071897222209,-2.40504719134649,-2.38668747924314,-2.36264631260151,
-2.35959871399723,-2.35866578942519,-2.3577670380385,-2.3569502149354,-2.3558814657657,
-2.35352118364814,-2.32459373769145,-2.29654575680122,-2.27463584481604,
-2.26689192179572,-2.26146401312443,-2.25981092590806,-2.25820581745774,
-2.25675124292062,-2.25488345237392,-2.25101997570405,-2.21924373342984,
-2.17928482583811,-2.1671699136665,-2.16073726948799,-2.15915968220089,
-2.15823322510564,-2.15742249621327,-2.15638482491187,-2.1542465136086,
-2.1395065492948,-2.08577624589031,-2.07140004749863,-2.06268103618726,
-2.06019187668445,-2.05857393964201,-2.05712216952763,-2.0552777984127,
-2.05236169027266,-2.04772232155495,-1.99953853325816,-1.97570526743478,
-1.96626767744714,-1.96085778159424,-1.95936870277049,-1.95846917893778,
-1.95765254775973,-1.95658524340341,-1.95478663059995,-1.9434099790743,
-1.91799120439229,-1.88772694968919,-1.87231927551921,-1.86311865031507,
-1.86050296187752,-1.85889977370593,-1.85744467721869,-1.8555730516855,
-1.85169021162132,-1.81850809897601,-1.76677185779097,-1.76122507661614,
-1.75972280899328,-1.75882025373135,-1.75800433728985,-1.75694257068182,
-1.75516316811648,-1.74418804933658,-1.72136985290494,-1.6900611230536,
-1.67332130951317,-1.66355328482702,-1.66088229386068,-1.65926664241411,
-1.65781403399879,-1.65596464115179,-1.65219528178667,-1.60502639272108,
-1.57768490415826,-1.5673668522046,-1.56160077034645,-1.56007818673895,
-1.55917105812497,-1.55835628651143,-1.55730295681437,-1.55502614719526,
-1.51836052359748,-1.48818810323082,-1.47290003241031,-1.46375083867949,
-1.46113996585804,-1.45953764543231,-1.45808196835307,-1.45620767716562,
-1.45231234645534,-1.41813850482374,-1.36961995146683,-1.36214511310618,
-1.360487451742,-1.35955029536359,-1.35874070175038,-1.35771806198026,-1.35572203363081,
-1.34386172073376,-1.32341833564824,-1.30132878670211,-1.26646888227994,
-1.26243306022236,-1.26053145396173,-1.2590719992533,-1.2574828237227,-1.25493158618636,
-1.24635937654294,-1.2323723237916,-1.17374781362434,-1.16292588504123,
-1.16115357533532,-1.16009370333893,-1.15927782947073,-1.1583737770197,
-1.15686569843996,-1.15126049009605,-1.09956352502326,-1.06641374910587,
-1.06253008648706,-1.06065785035423,-1.05920218307705,-1.05759826871704,
-1.05498117624992,-1.04577343891089,-1.0303494043819,-1.00003819826751,
-0.974444529098934,-0.963217064323069,-0.961425058549284,-0.960359461856212,
-0.959542812311369,-0.958641829059151,-0.957147280329022,-0.951684571195959,
-0.904750996535913,-0.866727930669484,-0.862816770061061,-0.860939234965246,
-0.859482975563456,-0.857881966587124,-0.855277621240369,-0.846195514747425,
-0.83105989349639,-0.800981321099322,-0.763922464213916,-0.761650962621176,
-0.760598526628658,-0.759783763875141,-0.758875889670408,-0.757350407703591,
-0.751554097394565,-0.74116190298647,-0.713611560223404,-0.666802986407777,
-0.663023968231003,-0.661172465233725,-0.65971940029886,-0.658104479717108,
-0.655437565964306,-0.645716002822019,-0.629085730864907,-0.59783019688253,
-0.576207046348278,-0.575397576877177,-0.563810623372752,-0.56182706548919,
-0.560807109344381,-0.559997719658555,-0.559058610687896,-0.557392093929252,
-0.54978748685632,-0.500782696499861,-0.467264820523939,-0.463377021456817,
-0.461504146732965,-0.460048586572978,-0.458445400808202,-0.455830875924833,
-0.446813068080903,-0.431760931719797,-0.374633846899037,-0.363951823021318,
-0.36218656076733,-0.361128799619181,-0.360313275574986,-0.359408221056493,
-0.357925848431869,-0.352588311743646,-0.301104387464563,-0.267469121873336,
-0.263579616080021,-0.26170632064315,-0.260250612210734,-0.258647443819501,
-0.25603335505551,-0.247877716442591,-0.23441891968878,-0.192651306027249,
-0.164825144212551,-0.162463942226863,-0.161394754082083,-0.160577589612655,
-0.159678448732992,-0.158745138479979,-0.155696271316655,-0.13363858630103,
-0.116108180047193,-0.0714612329704776,-0.0674035483814212,-0.0637812269603037,
-0.061936393232011,-0.0604840607567945,-0.0588652913045161,-0.0561811721654837,
-0.0530004676672074,-0.0467122517117062,-0.000592615563380933),
 .UNSPECIFIED.);
#821=B_SPLINE_CURVE_WITH_KNOTS('',3,(#24946,#24947,#24948,#24949,#24950,
#24951,#24952,#24953,#24954,#24955,#24956,#24957,#24958,#24959,#24960,#24961,
#24962,#24963,#24964,#24965,#24966,#24967,#24968,#24969,#24970,#24971,#24972,
#24973,#24974,#24975,#24976,#24977,#24978,#24979,#24980,#24981,#24982,#24983,
#24984,#24985,#24986,#24987,#24988,#24989,#24990,#24991,#24992,#24993,#24994,
#24995,#24996,#24997,#24998,#24999,#25000,#25001,#25002,#25003,#25004,#25005,
#25006,#25007,#25008,#25009,#25010,#25011,#25012,#25013,#25014,#25015,#25016,
#25017,#25018,#25019,#25020,#25021,#25022,#25023,#25024,#25025,#25026,#25027,
#25028,#25029,#25030,#25031,#25032,#25033,#25034,#25035,#25036,#25037,#25038,
#25039,#25040,#25041,#25042,#25043,#25044,#25045,#25046,#25047,#25048,#25049,
#25050,#25051,#25052,#25053,#25054,#25055,#25056,#25057,#25058,#25059,#25060,
#25061,#25062,#25063,#25064,#25065,#25066,#25067,#25068,#25069,#25070,#25071,
#25072,#25073,#25074,#25075,#25076,#25077,#25078,#25079,#25080,#25081,#25082,
#25083,#25084,#25085,#25086,#25087,#25088,#25089,#25090,#25091,#25092,#25093,
#25094,#25095,#25096,#25097,#25098,#25099,#25100,#25101,#25102,#25103,#25104,
#25105,#25106,#25107,#25108,#25109,#25110,#25111,#25112,#25113,#25114,#25115,
#25116,#25117,#25118,#25119,#25120,#25121,#25122,#25123,#25124,#25125,#25126,
#25127,#25128,#25129,#25130,#25131,#25132,#25133,#25134,#25135,#25136,#25137,
#25138,#25139,#25140,#25141,#25142,#25143,#25144,#25145,#25146,#25147,#25148,
#25149,#25150,#25151,#25152,#25153,#25154,#25155,#25156,#25157,#25158,#25159,
#25160,#25161,#25162,#25163,#25164,#25165,#25166,#25167,#25168,#25169,#25170,
#25171,#25172,#25173,#25174,#25175,#25176,#25177,#25178,#25179,#25180,#25181,
#25182,#25183,#25184,#25185,#25186,#25187,#25188,#25189,#25190,#25191,#25192,
#25193,#25194,#25195,#25196,#25197,#25198,#25199,#25200,#25201,#25202,#25203,
#25204,#25205,#25206,#25207,#25208,#25209,#25210,#25211,#25212,#25213,#25214,
#25215,#25216,#25217,#25218,#25219,#25220,#25221,#25222,#25223,#25224,#25225,
#25226,#25227,#25228,#25229,#25230,#25231,#25232,#25233,#25234,#25235,#25236,
#25237,#25238,#25239,#25240,#25241,#25242,#25243,#25244,#25245,#25246,#25247,
#25248,#25249,#25250,#25251,#25252,#25253,#25254,#25255,#25256,#25257,#25258,
#25259,#25260,#25261,#25262,#25263,#25264,#25265,#25266,#25267,#25268,#25269,
#25270,#25271,#25272,#25273,#25274,#25275,#25276,#25277,#25278,#25279,#25280,
#25281,#25282,#25283,#25284,#25285,#25286,#25287,#25288,#25289,#25290,#25291,
#25292,#25293,#25294,#25295,#25296,#25297,#25298,#25299,#25300,#25301,#25302,
#25303,#25304,#25305,#25306,#25307,#25308,#25309,#25310,#25311,#25312,#25313,
#25314,#25315,#25316,#25317,#25318,#25319,#25320,#25321,#25322,#25323,#25324,
#25325,#25326,#25327,#25328,#25329,#25330,#25331,#25332,#25333,#25334,#25335,
#25336,#25337,#25338,#25339,#25340,#25341,#25342,#25343,#25344,#25345,#25346,
#25347,#25348,#25349,#25350,#25351,#25352,#25353,#25354,#25355,#25356,#25357,
#25358,#25359,#25360,#25361,#25362,#25363,#25364,#25365,#25366,#25367,#25368,
#25369,#25370,#25371,#25372,#25373,#25374,#25375,#25376,#25377,#25378,#25379,
#25380,#25381,#25382,#25383,#25384,#25385,#25386,#25387,#25388,#25389,#25390,
#25391,#25392,#25393,#25394,#25395,#25396,#25397,#25398,#25399,#25400,#25401,
#25402,#25403,#25404,#25405,#25406,#25407,#25408,#25409,#25410,#25411,#25412,
#25413,#25414,#25415,#25416,#25417,#25418,#25419,#25420,#25421,#25422,#25423,
#25424,#25425,#25426,#25427,#25428,#25429,#25430,#25431,#25432,#25433,#25434,
#25435,#25436,#25437,#25438,#25439,#25440,#25441,#25442,#25443,#25444,#25445,
#25446,#25447,#25448,#25449),.UNSPECIFIED.,.F.,.F.,(4,2,2,2,2,2,2,2,2,2,
2,2,2,2,2,2,2,2,2,2,2,2,2,2,2,2,2,2,2,2,2,2,2,2,2,2,2,2,2,2,2,2,2,2,2,2,
2,2,2,2,2,2,2,2,2,2,2,2,2,2,2,2,2,2,2,2,2,2,2,2,2,2,2,2,2,2,2,2,2,2,2,2,
2,2,2,2,2,2,2,2,2,2,2,2,2,2,2,2,2,2,2,2,2,2,2,2,2,2,2,2,2,2,2,2,2,2,2,2,
2,2,2,2,2,2,2,2,2,2,2,2,2,2,2,2,2,2,2,2,2,2,2,2,2,2,2,2,2,2,2,2,2,2,2,2,
2,2,2,2,2,2,2,2,2,2,2,2,2,2,2,2,2,2,2,2,2,2,2,2,2,2,2,2,2,2,2,2,2,2,2,2,
2,2,2,2,2,2,2,2,2,2,2,2,2,2,2,2,2,2,2,2,2,2,2,2,2,2,2,2,2,2,2,2,2,2,2,2,
2,2,2,2,2,2,2,2,2,2,2,2,2,2,2,2,2,2,2,2,2,2,2,2,2,4),(-2.51289715151977,
-2.47972640089436,-2.4768752173438,-2.47545123771563,-2.47450337870612,
-2.47359423931493,-2.4727802537463,-2.47173133266218,-2.46999518265789,
-2.45987087398384,-2.43689502740499,-2.42524062078833,-2.41514200848716,
-2.38743176820728,-2.37826035077444,-2.37562763474891,-2.37402071742516,
-2.37256660773301,-2.370702343459,-2.36685666586062,-2.32290528012821,-2.29115758319708,
-2.2817425175326,-2.27636157504926,-2.27487764146156,-2.27397247433261,
-2.27315741957376,-2.27210102859931,-2.27033967033494,-2.259725047596,-2.24629664299976,
-2.2005665046346,-2.18686447011953,-2.17857500778693,-2.17596069937408,
-2.17435786716931,-2.17290277256296,-2.17103069948715,-2.16714530157488,
-2.13374945859055,-2.08201329160179,-2.07667048902124,-2.07519211461073,
-2.07428815772761,-2.07347267626837,-2.07241372771533,-2.07010664154477,
-2.0350864889324,-2.00549111007562,-1.98876800224782,-1.97900711171298,
-1.97633688797576,-1.97472146276348,-1.97326890526985,-1.97141936813974,
-1.96764898339249,-1.92052813144785,-1.89315895174763,-1.88283174289908,
-1.87706212037299,-1.87553927054924,-1.87463211338769,-1.87381740569389,
-1.87276427629076,-1.87048834849328,-1.83356479458625,-1.803483209101,-1.78063170329132,
-1.77722809410557,-1.77545331755989,-1.77414629985647,-1.7727319081527,
-1.77025958348092,-1.76411053959124,-1.71785832347955,-1.67958101061963,
-1.67664572735292,-1.67546506617423,-1.67463205509275,-1.67387100196087,
-1.6728300235922,-1.6707639031627,-1.63497248436216,-1.60450792182737,-1.58885237755332,
-1.57954411197088,-1.57691735353388,-1.57531147709936,-1.57385661652084,
-1.57198903045255,-1.56812803289837,-1.52486435117493,-1.49502140709829,
-1.4838389281787,-1.477735840258,-1.47618352669626,-1.47526973319552,-1.47445644884759,
-1.47341475113685,-1.47170360939251,-1.46205251553749,-1.45888924903372,
-1.40401450461822,-1.38885922138649,-1.37976796394562,-1.37716298134187,
-1.3755620018936,-1.37410604651243,-1.37222929335983,-1.3683211868747,-1.33201926574934,
-1.29816507435623,-1.28497179813062,-1.27812818553261,-1.27651628052509,
-1.2755892835107,-1.2747784578422,-1.27374115624603,-1.27160529590393,-1.25694088016128,
-1.23050686048361,-1.18600387191342,-1.18209736062994,-1.17833424367952,
-1.17648607169198,-1.17503357716437,-1.17341717887167,-1.17074292618847,
-1.16094066541488,-1.14411634756192,-1.11271303806091,-1.08943276810935,
-1.07903834866974,-1.07728790477791,-1.07623463406456,-1.07541989458437,
-1.07451277982174,-1.07299018083451,-1.06722351048025,-1.05690526936063,
-1.02956790520883,-0.982441725275819,-0.978672216904429,-0.976822830780169,
-0.975370263585332,-0.973754695043602,-0.971083927791218,-0.961317750343273,
-0.944579525204524,-0.913243976293078,-0.890366723660837,-0.879427532941609,
-0.877649906380281,-0.876588675830873,-0.875772854335678,-0.874870052571093,
-0.873366628446128,-0.867807256263376,-0.816106831082813,-0.782940911764785,
-0.779058324616186,-0.777186712484757,-0.775731577407039,-0.774128297051813,
-0.771512346654275,-0.762309723954097,-0.746895326883556,-0.716598503404048,
-0.690990207577226,-0.679780807210232,-0.677990136832804,-0.676925131933392,
-0.676108814817793,-0.67520806739347,-0.673713630647349,-0.668248308879818,
-0.621237503132578,-0.583327360996343,-0.579418492049704,-0.577541818563347,
-0.576086121810634,-0.574485624990618,-0.571881873711318,-0.562799443690345,
-0.54766097574086,-0.517586744244526,-0.480561134962328,-0.478290693298444,
-0.477238689433416,-0.476424235318645,-0.47551667661698,-0.473991662449225,
-0.468196401982876,-0.457805276146846,-0.430247531516478,-0.383481798468726,
-0.379701893144844,-0.377850623335885,-0.376398046389941,-0.37492107837684,
-0.372466840650849,-0.369569347572885,-0.364041484016353,-0.350541511930078,
-0.294915708414671,-0.292086570921313,-0.280457542112901,-0.278472121437683,
-0.277451899961462,-0.276642658933393,-0.275704131002375,-0.274039656527685,
-0.266461282860458,-0.217573750587891,-0.183930882811766,-0.180043669558134,
-0.17817116608226,-0.176715934090724,-0.176698684454885,-0.176682067532365,
-0.1766660547917,-0.176650619204641,-0.176635735227564,-0.176621378708022,
-0.176607526789569,-0.176594157831531,-0.176581251341022,-0.176568787887566,
-0.176556749046612,-0.176545117334244,-0.176533876138712,-0.176523009688158,
-0.176512502997364,-0.176502341813206,-0.176492512568804,-0.176483002346398,
-0.176473798843879,-0.176464890344472,-0.174808911736105,-0.171925382564298,
-0.168396814929211,-0.161141469404808,-0.141239909810671,-0.0830116117044468,
-0.0794416450292309,-0.0781226243214013,-0.0773465217319725,-0.0765241265629663,
-0.075403103231885,-0.072821025816527,-0.0410478306117794,-0.000592895662585235),
 .UNSPECIFIED.);
#822=B_SPLINE_CURVE_WITH_KNOTS('',3,(#25451,#25452,#25453,#25454,#25455,
#25456,#25457,#25458,#25459,#25460,#25461,#25462,#25463,#25464,#25465,#25466,
#25467,#25468,#25469,#25470,#25471,#25472,#25473,#25474,#25475,#25476,#25477,
#25478,#25479,#25480,#25481,#25482,#25483,#25484,#25485,#25486,#25487,#25488,
#25489,#25490,#25491,#25492,#25493,#25494,#25495,#25496,#25497,#25498,#25499,
#25500,#25501,#25502,#25503,#25504,#25505,#25506,#25507,#25508,#25509,#25510,
#25511,#25512,#25513,#25514,#25515,#25516,#25517,#25518,#25519,#25520,#25521,
#25522,#25523,#25524,#25525,#25526,#25527,#25528,#25529,#25530,#25531,#25532,
#25533,#25534,#25535,#25536,#25537,#25538,#25539,#25540,#25541,#25542,#25543,
#25544,#25545,#25546,#25547,#25548,#25549,#25550,#25551,#25552,#25553,#25554,
#25555,#25556,#25557,#25558,#25559,#25560,#25561,#25562,#25563,#25564,#25565,
#25566,#25567,#25568,#25569,#25570,#25571,#25572,#25573,#25574,#25575,#25576,
#25577,#25578,#25579,#25580,#25581,#25582,#25583,#25584,#25585,#25586,#25587,
#25588,#25589,#25590,#25591,#25592,#25593,#25594,#25595,#25596,#25597,#25598,
#25599,#25600,#25601,#25602,#25603,#25604,#25605,#25606,#25607,#25608,#25609,
#25610,#25611,#25612,#25613,#25614,#25615,#25616,#25617,#25618,#25619,#25620,
#25621,#25622,#25623,#25624,#25625,#25626,#25627,#25628,#25629,#25630,#25631,
#25632,#25633,#25634,#25635,#25636,#25637,#25638,#25639,#25640),
 .UNSPECIFIED.,.F.,.F.,(4,3,3,3,3,3,3,3,3,3,3,3,3,3,3,3,3,3,3,3,3,3,3,3,
3,3,3,3,3,3,3,3,3,3,3,3,3,3,3,3,3,3,3,3,3,3,3,3,3,3,3,3,3,3,3,3,3,3,3,3,
3,3,3,4),(78.5398163397452,78.6441703164354,78.7485007550361,78.852843436871,
78.9573058341078,79.0618360039011,79.1665532872366,79.2144993807763,79.3194451956405,
79.4242332606396,79.5288977912809,79.6334962990726,79.7380643684846,79.8426375398172,
79.9473214948844,80.0520665582851,80.1569944047453,80.213180249137,80.3181260640012,
80.422914129,80.5275786596412,80.6321771674329,80.7367452368449,80.8413184081774,
80.9460023632446,81.0507474266453,81.1556752731056,81.2118611174978,81.3168069323619,
81.4215949973606,81.5262595280019,81.6308580357935,81.7354261052054,81.8399992765384,
81.9446832316056,82.0494282950062,82.1543561414665,82.2105419858585,82.3154878007227,
82.4202758657216,82.5249403963629,82.6295389041546,82.7341069735665,82.8386801448994,
82.9433640999666,83.0481091633673,83.1530370098276,83.2092228542193,83.3141686690836,
83.4189567340828,83.5236212647241,83.6282197725159,83.7327878419278,83.8373610132607,
83.9420449683279,84.0467900317286,84.1517178781889,84.20790372258,84.3139463242525,
84.4198215071954,84.5255441086588,84.6311761129126,84.736764788714,84.8230016469248),
 .UNSPECIFIED.);
#823=B_SPLINE_CURVE_WITH_KNOTS('',3,(#25642,#25643,#25644,#25645,#25646,
#25647,#25648,#25649,#25650,#25651,#25652,#25653,#25654,#25655,#25656,#25657,
#25658,#25659,#25660,#25661,#25662,#25663,#25664,#25665,#25666,#25667,#25668,
#25669,#25670,#25671,#25672,#25673,#25674,#25675,#25676,#25677,#25678,#25679,
#25680,#25681,#25682,#25683,#25684,#25685,#25686,#25687,#25688,#25689,#25690,
#25691,#25692,#25693,#25694,#25695,#25696,#25697,#25698,#25699,#25700,#25701,
#25702,#25703,#25704,#25705,#25706,#25707,#25708,#25709,#25710,#25711,#25712,
#25713,#25714,#25715,#25716,#25717,#25718,#25719,#25720,#25721,#25722,#25723,
#25724,#25725,#25726,#25727,#25728,#25729,#25730,#25731,#25732,#25733,#25734,
#25735,#25736,#25737,#25738,#25739,#25740,#25741,#25742,#25743,#25744,#25745,
#25746,#25747,#25748,#25749,#25750,#25751,#25752,#25753,#25754,#25755,#25756,
#25757,#25758,#25759,#25760,#25761,#25762,#25763,#25764,#25765,#25766,#25767,
#25768,#25769,#25770,#25771,#25772,#25773,#25774,#25775,#25776,#25777,#25778,
#25779,#25780,#25781,#25782,#25783,#25784,#25785,#25786,#25787,#25788,#25789,
#25790,#25791,#25792,#25793,#25794,#25795,#25796,#25797,#25798,#25799,#25800,
#25801,#25802,#25803,#25804,#25805,#25806,#25807,#25808,#25809,#25810,#25811,
#25812,#25813,#25814,#25815,#25816,#25817,#25818,#25819,#25820,#25821,#25822,
#25823,#25824,#25825,#25826,#25827,#25828,#25829,#25830,#25831),
 .UNSPECIFIED.,.F.,.F.,(4,3,3,3,3,3,3,3,3,3,3,3,3,3,3,3,3,3,3,3,3,3,3,3,
3,3,3,3,3,3,3,3,3,3,3,3,3,3,3,3,3,3,3,3,3,3,3,3,3,3,3,3,3,3,3,3,3,3,3,3,
3,3,3,4),(72.2566313277358,72.361007636202,72.4686834530033,72.5727829330681,
72.6768214388177,72.7808353386096,72.8848609619492,72.9890000281572,73.0932076440146,
73.1975874607193,73.2224141706118,73.3273599854761,73.4321480504749,73.5368125811162,
73.6414110889079,73.74597915832,73.8505523296524,73.9552362847196,74.0599813481202,
74.1649091945805,74.2210950389725,74.3260408538366,74.4308289188352,74.5354934494765,
74.6400919572682,74.7446600266802,74.8492331980132,74.9539171530804,75.058662216481,
75.1635900629414,75.2197759073333,75.3247217221975,75.4295097871962,75.5341743178374,
75.6387728256293,75.7433408950412,75.8479140663737,75.9525980214409,76.0573430848416,
76.1622709313019,76.218456775694,76.3234025905581,76.4281906555569,76.5328551861981,
76.6374536939898,76.7420217634016,76.8465949347344,76.9512788898016,77.0560239532023,
77.1609517996625,77.2171376440548,77.322083458919,77.4268715239178,77.5315360545591,
77.6361345623507,77.7407026317626,77.8452758030951,77.9499597581623,78.0547048215629,
78.1596326680231,78.2158185124155,78.3402426631434,78.4633027052255,78.5398163393914),
 .UNSPECIFIED.);
#824=B_SPLINE_CURVE_WITH_KNOTS('',3,(#25833,#25834,#25835,#25836,#25837,
#25838,#25839,#25840,#25841,#25842,#25843),.UNSPECIFIED.,.F.,.F.,(4,1,1,
1,1,1,1,1,4),(65.9734480974445,66.2316480920865,67.2303289604472,68.229009828808,
69.2276906971688,70.2263715655295,71.2250524338903,72.223733302251,72.2566310325656),
 .UNSPECIFIED.);
#825=B_SPLINE_CURVE_WITH_KNOTS('',3,(#25845,#25846,#25847,#25848,#25849,
#25850,#25851,#25852,#25853,#25854,#25855,#25856,#25857,#25858,#25859,#25860,
#25861,#25862,#25863,#25864,#25865,#25866,#25867,#25868,#25869,#25870,#25871,
#25872,#25873,#25874,#25875,#25876,#25877,#25878,#25879,#25880,#25881,#25882,
#25883,#25884,#25885,#25886,#25887,#25888,#25889,#25890,#25891,#25892,#25893,
#25894,#25895,#25896,#25897,#25898,#25899,#25900,#25901,#25902,#25903,#25904,
#25905,#25906,#25907,#25908,#25909,#25910,#25911,#25912,#25913,#25914,#25915,
#25916,#25917,#25918,#25919,#25920,#25921,#25922,#25923,#25924,#25925,#25926,
#25927,#25928,#25929,#25930,#25931,#25932,#25933,#25934,#25935,#25936,#25937,
#25938,#25939,#25940,#25941,#25942,#25943,#25944,#25945,#25946,#25947,#25948,
#25949,#25950,#25951,#25952,#25953,#25954,#25955,#25956,#25957,#25958,#25959,
#25960,#25961,#25962,#25963,#25964,#25965,#25966,#25967,#25968,#25969,#25970,
#25971,#25972,#25973,#25974,#25975,#25976,#25977,#25978,#25979,#25980,#25981,
#25982,#25983,#25984,#25985,#25986,#25987,#25988,#25989,#25990,#25991,#25992,
#25993,#25994,#25995,#25996,#25997,#25998,#25999,#26000,#26001,#26002,#26003,
#26004,#26005,#26006,#26007,#26008,#26009,#26010,#26011,#26012,#26013,#26014,
#26015,#26016,#26017,#26018,#26019,#26020,#26021,#26022,#26023,#26024,#26025,
#26026,#26027,#26028,#26029,#26030,#26031,#26032,#26033,#26034,#26035,#26036,
#26037,#26038,#26039,#26040,#26041,#26042,#26043,#26044,#26045,#26046,#26047,
#26048,#26049,#26050,#26051,#26052,#26053,#26054,#26055,#26056,#26057,#26058,
#26059,#26060,#26061,#26062,#26063,#26064,#26065,#26066,#26067,#26068,#26069,
#26070,#26071,#26072,#26073,#26074,#26075,#26076,#26077,#26078,#26079,#26080,
#26081,#26082,#26083,#26084,#26085,#26086,#26087,#26088,#26089,#26090,#26091,
#26092,#26093,#26094,#26095,#26096,#26097,#26098,#26099,#26100,#26101,#26102,
#26103,#26104,#26105,#26106,#26107,#26108,#26109,#26110,#26111,#26112,#26113,
#26114,#26115,#26116,#26117,#26118,#26119,#26120,#26121,#26122,#26123,#26124,
#26125,#26126,#26127,#26128,#26129,#26130,#26131,#26132,#26133,#26134,#26135,
#26136,#26137,#26138,#26139,#26140,#26141,#26142,#26143,#26144,#26145,#26146,
#26147,#26148,#26149,#26150,#26151,#26152,#26153,#26154,#26155,#26156,#26157,
#26158,#26159,#26160,#26161,#26162,#26163,#26164,#26165,#26166,#26167,#26168,
#26169,#26170,#26171,#26172,#26173,#26174,#26175,#26176,#26177,#26178,#26179,
#26180,#26181,#26182,#26183,#26184,#26185,#26186,#26187,#26188,#26189,#26190,
#26191,#26192,#26193,#26194,#26195,#26196,#26197,#26198,#26199,#26200,#26201,
#26202,#26203,#26204,#26205,#26206,#26207,#26208,#26209,#26210,#26211,#26212,
#26213,#26214,#26215,#26216,#26217,#26218,#26219,#26220,#26221,#26222,#26223,
#26224,#26225,#26226,#26227,#26228,#26229,#26230,#26231,#26232,#26233,#26234,
#26235,#26236,#26237,#26238,#26239,#26240,#26241,#26242,#26243,#26244,#26245,
#26246,#26247,#26248,#26249,#26250,#26251,#26252,#26253,#26254,#26255,#26256,
#26257,#26258,#26259,#26260,#26261,#26262,#26263,#26264,#26265,#26266,#26267,
#26268,#26269,#26270,#26271,#26272,#26273,#26274,#26275,#26276,#26277,#26278,
#26279,#26280,#26281,#26282,#26283,#26284,#26285,#26286,#26287,#26288,#26289,
#26290,#26291,#26292,#26293,#26294,#26295,#26296,#26297,#26298,#26299,#26300,
#26301,#26302,#26303,#26304,#26305,#26306,#26307,#26308,#26309,#26310,#26311,
#26312,#26313,#26314),.UNSPECIFIED.,.F.,.F.,(4,2,2,2,2,2,2,2,2,2,2,2,2,
2,2,2,2,2,2,2,2,2,2,2,2,2,2,2,2,2,2,2,2,2,2,2,2,2,2,2,2,2,2,2,2,2,2,2,2,
2,2,2,2,2,2,2,2,2,2,2,2,2,2,2,2,2,2,2,2,2,2,2,2,2,2,2,2,2,2,2,2,2,2,2,2,
2,2,2,2,2,2,2,2,2,2,2,2,2,2,2,2,2,2,2,2,2,2,2,2,2,2,2,2,2,2,2,2,2,2,2,2,
2,2,2,2,2,2,2,2,2,2,2,2,2,2,2,2,2,2,2,2,2,2,2,2,2,2,2,2,2,2,2,2,2,2,2,2,
2,2,2,2,2,2,2,2,2,2,2,2,2,2,2,2,2,2,2,2,2,2,2,2,2,2,2,2,2,2,2,2,2,2,2,2,
2,2,2,2,2,2,2,2,2,2,2,2,2,2,2,2,2,2,2,2,2,2,2,2,2,2,2,2,2,2,2,2,2,2,2,2,
2,2,2,2,2,4),(-2.51416891162704,-2.48112270253285,-2.47186008798328,-2.46943928752675,
-2.46779239009978,-2.46619153174604,-2.46473569892957,-2.46285912126152,
-2.45895144398875,-2.4200747924581,-2.3996149906461,-2.37391068630378,-2.36858079106766,
-2.36706981317024,-2.36616532792609,-2.36534996776999,-2.36429196677082,
-2.36207219254794,-2.32414945231398,-2.29061359006509,-2.27200515469304,
-2.26877725039748,-2.26733773690969,-2.26586997598837,-2.26449431452899,
-2.26221985462322,-2.256394743407,-2.21543503076707,-2.17397878663389,-2.16903892556346,
-2.1674653268296,-2.16653967575371,-2.16572866133809,-2.16468932009309,
-2.16254308567906,-2.14759180221069,-2.14209604215475,-2.09393030920172,
-2.07965863482546,-2.07098620890914,-2.06849689389138,-2.06688088309571,
-2.06542837744966,-2.06357969908709,-2.05981383516076,-2.01251557648366,
-1.98525906830234,-1.97496842007012,-1.96921324341968,-1.96769166551787,
-1.96678477093518,-1.96596995787136,-1.96491624380949,-1.96263734014924,
-1.92603178272515,-1.8958405270843,-1.88052852510911,-1.87136896766193,
-1.86875708210059,-1.86715455330332,-1.86569895822228,-1.8638251532161,
-1.85993221462304,-1.82597341276369,-1.77728992516677,-1.76976838612602,
-1.76810753649167,-1.7671696881328,-1.76636018550611,-1.76533854769543,
-1.76334712711815,-1.75160843290355,-1.74898896811829,-1.74125508505489,
-1.72642761673244,-1.6962056936859,-1.68085816534065,-1.67168285245546,
-1.66906916991145,-1.66746611052446,-1.66601040886064,-1.66413699295306,
-1.66024677170934,-1.62633665827277,-1.57760219289598,-1.5700677892355,
-1.56840591323352,-1.56746776586281,-1.5666581789851,-1.56563665861495,
-1.56364613505438,-1.55192789941672,-1.54934855957861,-1.52697197490935,
-1.49665820613985,-1.48119809749935,-1.47197366045526,-1.46935485770892,
-1.46775053282128,-1.46629491033399,-1.46442331601354,-1.46054310021216,
-1.41879944532561,-1.38989265679177,-1.3710613131453,-1.368983545232,-1.3679576737996,
-1.36722444284156,-1.36643134282357,-1.36502693662354,-1.36086526791762,
-1.31984189903675,-1.27488666430804,-1.27067183813501,-1.26873627636904,
-1.26727176775314,-1.26588883628996,-1.26357797155384,-1.25752231947305,
-1.22495740135979,-1.19145095654736,-1.18666365140535,-1.17143598408825,
-1.16927945211793,-1.16823793600518,-1.16742653848506,-1.16650190127689,
-1.16490119778426,-1.15820638732285,-1.14543283256662,-1.13269258449123,
-1.07755754527285,-1.07173958921664,-1.06946598452273,-1.06809028017392,
-1.06662204527329,-1.06466208733977,-1.06031489260978,-1.05452168404084,
-1.04010480592576,-0.978680353774963,-0.975736221608437,-0.973868883035947,
-0.970164949376239,-0.968825262300434,-0.968045034186847,-0.967224737471353,
-0.96611700916113,-0.963609719510077,-0.935553159304165,-0.898137150389062,
-0.890914222607529,-0.873991319715326,-0.870967677952838,-0.869090028091327,
-0.86763352473352,-0.866032091453499,-0.863426705226515,-0.854337454798115,
-0.839186541994366,-0.809092250677893,-0.772054981788037,-0.769783350459396,
-0.768730772434134,-0.767915863734272,-0.767007787432175,-0.765481879268838,
-0.759682938413996,-0.749284896909411,-0.721704884042302,-0.674919046907078,
-0.671138479929674,-0.669286461572267,-0.66783310339603,-0.666217971562694,
-0.663550974227376,-0.653832008059458,-0.637209168153602,-0.605955943969575,
-0.572391827746307,-0.570293766106476,-0.569244586849225,-0.568481256768335,
-0.567649779227091,-0.566478168594516,-0.56359972742884,-0.542478475642401,
-0.477843504409794,-0.472271215811136,-0.47003870833555,-0.468670737969772,
-0.467197544666218,-0.465207876070659,-0.460696951540999,-0.454628024984922,
-0.439232901114029,-0.408972928124254,-0.372503523125898,-0.370448004676696,
-0.369409613902607,-0.368649135420992,-0.367815310540694,-0.36665477269793,
-0.363863429954477,-0.359892400164121,-0.349002675361108,-0.312057429386215,
-0.275580973259992,-0.271672066872095,-0.269794921876307,-0.268338658432807,
-0.266737336061764,-0.26413178674946,-0.255038522276201,-0.239877597092108,
-0.192686910300566,-0.187704220519794,-0.17257470970358,-0.17042161555553,
-0.169380754104277,-0.168569397249749,-0.167807880252338,-0.166413887879585,
-0.161947025489448,-0.154623662908096,-0.131234738674594,-0.0790727568882605,
-0.0729821347089623,-0.0706658145245276,-0.0692818555094672,-0.0678179147098098,
-0.0658858994621991,-0.0616898857032018,-0.0208011237217479,-0.000592836805715096),
 .UNSPECIFIED.);
#826=B_SPLINE_CURVE_WITH_KNOTS('',3,(#26316,#26317,#26318,#26319,#26320,
#26321,#26322,#26323,#26324,#26325,#26326,#26327,#26328,#26329,#26330,#26331,
#26332,#26333,#26334,#26335,#26336,#26337,#26338,#26339,#26340,#26341,#26342,
#26343,#26344,#26345,#26346,#26347,#26348,#26349,#26350,#26351,#26352,#26353,
#26354,#26355,#26356,#26357,#26358,#26359,#26360,#26361,#26362,#26363,#26364,
#26365,#26366,#26367,#26368,#26369,#26370,#26371,#26372,#26373,#26374,#26375,
#26376,#26377,#26378,#26379,#26380,#26381,#26382,#26383,#26384,#26385,#26386,
#26387,#26388,#26389,#26390,#26391,#26392,#26393,#26394,#26395,#26396,#26397,
#26398,#26399,#26400,#26401,#26402,#26403,#26404,#26405,#26406,#26407,#26408,
#26409,#26410,#26411,#26412,#26413,#26414,#26415,#26416,#26417,#26418,#26419,
#26420,#26421,#26422,#26423,#26424,#26425,#26426,#26427,#26428,#26429,#26430,
#26431,#26432,#26433,#26434,#26435,#26436,#26437,#26438,#26439,#26440,#26441,
#26442,#26443,#26444,#26445,#26446,#26447,#26448,#26449,#26450,#26451,#26452,
#26453,#26454,#26455,#26456,#26457,#26458,#26459,#26460,#26461,#26462,#26463,
#26464,#26465,#26466,#26467,#26468,#26469,#26470,#26471,#26472,#26473,#26474,
#26475,#26476,#26477,#26478,#26479,#26480,#26481,#26482,#26483,#26484,#26485,
#26486,#26487,#26488,#26489,#26490,#26491,#26492,#26493,#26494,#26495,#26496,
#26497,#26498,#26499,#26500,#26501,#26502),.UNSPECIFIED.,.F.,.F.,(4,3,3,
3,3,3,3,3,3,3,3,3,3,3,3,3,3,3,3,3,3,3,3,3,3,3,3,3,3,3,3,3,3,3,3,3,3,3,3,
3,3,3,3,3,3,3,3,3,3,3,3,3,3,3,3,3,3,3,3,3,3,3,4),(47.1238898038472,47.2567115932322,
47.3616574080963,47.4664454730952,47.5711100037364,47.6757085115281,47.7802765809401,
47.8848497522726,47.9895337073398,48.0942787707405,48.1992066172007,48.255392461593,
48.3603382764572,48.465126341456,48.5697908720972,48.6743893798889,48.7789574493009,
48.8835306206336,48.9882145757009,49.0929596391015,49.1978874855618,49.2540733299537,
49.3590191448179,49.4638072098166,49.5684717404579,49.6730702482496,49.7776383176615,
49.8822114889942,49.9868954440615,50.0916405074622,50.1965683539224,50.2527541983145,
50.3577000131787,50.4624880781775,50.5671526088188,50.6717511166105,50.7763191860225,
50.8808923573552,50.9855763124224,51.0903213758231,51.1952492222833,51.2514350666752,
51.3563808815394,51.4611689465382,51.5658334771794,51.6704319849711,51.7750000543831,
51.8795732257158,51.984257180783,52.0890022441837,52.193930090644,52.250115935036,
52.3550617499002,52.459849814899,52.5645143455403,52.6691128533319,52.7736809227439,
52.8782540940765,52.9829380491437,53.0876831125444,53.1926109590046,53.2487968033967,
53.4070751110268),.UNSPECIFIED.);
#827=B_SPLINE_CURVE_WITH_KNOTS('',3,(#26504,#26505,#26506,#26507,#26508,
#26509,#26510,#26511,#26512,#26513,#26514,#26515,#26516,#26517,#26518,#26519,
#26520,#26521,#26522,#26523,#26524,#26525,#26526,#26527,#26528,#26529,#26530,
#26531,#26532,#26533,#26534,#26535,#26536,#26537,#26538,#26539,#26540,#26541,
#26542,#26543,#26544,#26545,#26546,#26547,#26548,#26549,#26550,#26551,#26552,
#26553,#26554,#26555,#26556,#26557,#26558,#26559,#26560,#26561,#26562,#26563,
#26564,#26565,#26566,#26567,#26568,#26569,#26570,#26571,#26572,#26573,#26574,
#26575,#26576,#26577,#26578,#26579,#26580,#26581,#26582,#26583,#26584,#26585,
#26586,#26587,#26588,#26589,#26590,#26591,#26592,#26593,#26594,#26595,#26596,
#26597,#26598,#26599,#26600,#26601,#26602,#26603,#26604,#26605,#26606,#26607,
#26608,#26609,#26610,#26611,#26612,#26613,#26614,#26615,#26616,#26617,#26618,
#26619,#26620,#26621,#26622,#26623,#26624,#26625,#26626,#26627,#26628,#26629,
#26630,#26631,#26632,#26633,#26634,#26635,#26636,#26637,#26638,#26639,#26640,
#26641,#26642,#26643,#26644,#26645,#26646,#26647,#26648,#26649,#26650,#26651,
#26652,#26653,#26654,#26655,#26656,#26657,#26658,#26659,#26660,#26661,#26662,
#26663,#26664,#26665,#26666,#26667,#26668,#26669,#26670,#26671,#26672,#26673,
#26674,#26675,#26676,#26677,#26678,#26679,#26680,#26681,#26682,#26683,#26684,
#26685,#26686,#26687,#26688,#26689,#26690,#26691,#26692,#26693,#26694,#26695,
#26696,#26697,#26698,#26699,#26700,#26701,#26702,#26703,#26704,#26705,#26706,
#26707,#26708,#26709,#26710,#26711,#26712,#26713,#26714,#26715,#26716,#26717,
#26718,#26719,#26720,#26721,#26722,#26723,#26724,#26725,#26726,#26727,#26728,
#26729,#26730,#26731,#26732,#26733,#26734,#26735,#26736,#26737,#26738,#26739,
#26740,#26741,#26742,#26743,#26744,#26745,#26746,#26747,#26748,#26749,#26750,
#26751,#26752,#26753,#26754,#26755,#26756,#26757,#26758,#26759,#26760,#26761,
#26762,#26763,#26764,#26765,#26766,#26767,#26768,#26769,#26770,#26771,#26772,
#26773,#26774,#26775,#26776,#26777,#26778,#26779,#26780,#26781,#26782,#26783,
#26784,#26785,#26786,#26787,#26788,#26789,#26790,#26791,#26792,#26793,#26794,
#26795,#26796,#26797,#26798,#26799,#26800,#26801,#26802,#26803,#26804,#26805,
#26806,#26807,#26808,#26809,#26810,#26811,#26812,#26813,#26814,#26815,#26816,
#26817,#26818,#26819,#26820,#26821,#26822,#26823,#26824,#26825,#26826,#26827,
#26828,#26829,#26830,#26831,#26832,#26833,#26834,#26835,#26836,#26837,#26838,
#26839,#26840,#26841,#26842,#26843,#26844,#26845,#26846,#26847,#26848,#26849,
#26850,#26851,#26852,#26853,#26854,#26855,#26856,#26857,#26858,#26859,#26860,
#26861,#26862,#26863,#26864,#26865,#26866,#26867,#26868,#26869,#26870,#26871,
#26872,#26873,#26874,#26875,#26876,#26877,#26878,#26879,#26880,#26881,#26882,
#26883,#26884,#26885,#26886,#26887,#26888,#26889,#26890,#26891,#26892,#26893,
#26894,#26895,#26896,#26897,#26898,#26899,#26900,#26901,#26902,#26903,#26904,
#26905,#26906,#26907,#26908,#26909,#26910,#26911,#26912,#26913,#26914,#26915,
#26916,#26917,#26918,#26919,#26920,#26921,#26922,#26923,#26924,#26925,#26926,
#26927,#26928,#26929,#26930,#26931,#26932,#26933,#26934,#26935,#26936,#26937,
#26938,#26939,#26940,#26941,#26942,#26943,#26944,#26945,#26946,#26947,#26948,
#26949,#26950,#26951,#26952,#26953,#26954,#26955,#26956,#26957,#26958,#26959,
#26960,#26961,#26962,#26963,#26964,#26965,#26966,#26967,#26968,#26969,#26970,
#26971,#26972,#26973),.UNSPECIFIED.,.F.,.F.,(4,2,2,2,2,2,2,2,2,2,2,2,2,
2,2,2,2,2,2,2,2,2,2,2,2,2,2,2,2,2,2,2,2,2,2,2,2,2,2,2,2,2,2,2,2,2,2,2,2,
2,2,2,2,2,2,2,2,2,2,2,2,2,2,2,2,2,2,2,2,2,2,2,2,2,2,2,2,2,2,2,2,2,2,2,2,
2,2,2,2,2,2,2,2,2,2,2,2,2,2,2,2,2,2,2,2,2,2,2,2,2,2,2,2,2,2,2,2,2,2,2,2,
2,2,2,2,2,2,2,2,2,2,2,2,2,2,2,2,2,2,2,2,2,2,2,2,2,2,2,2,2,2,2,2,2,2,2,2,
2,2,2,2,2,2,2,2,2,2,2,2,2,2,2,2,2,2,2,2,2,2,2,2,2,2,2,2,2,2,2,2,2,2,2,2,
2,2,2,2,2,2,2,2,2,2,2,2,2,2,2,2,2,2,2,2,2,2,2,2,2,2,2,2,2,2,2,2,2,2,2,2,
2,2,2,2,2,4),(-2.5139883673475,-2.46796189057673,-2.45376184525105,-2.44803099167605,
-2.44372121743481,-2.44176862456714,-2.44030205188033,-2.43892509066694,
-2.43664284139591,-2.4307668503137,-2.37618862860514,-2.35506701823993,
-2.34765131853795,-2.34313811010895,-2.34174248311774,-2.34098116445121,
-2.34017030178535,-2.33913114717567,-2.33746514750599,-2.32860442250549,
-2.29627776636585,-2.26977167225771,-2.25461853545282,-2.24552863384444,
-2.24292407356314,-2.24132336089935,-2.23986765289813,-2.2379912253208,
-2.23408382122551,-2.19522871381193,-2.14906705702404,-2.14546636955356,
-2.1436675682756,-2.14223632790328,-2.14132913532577,-2.14051821451748,
-2.13947927204239,-2.13733481994395,-2.12242954689244,-2.11385539126091,
-2.07301147089012,-2.04741353437713,-2.04392886096236,-2.04213729394979,
-2.04070359332995,-2.03905602474411,-2.03624112604167,-2.02622546872829,
-2.02422581088746,-1.9622947201022,-1.95042962099684,-1.94621597514117,
-1.94326184262198,-1.9420781046726,-1.94124447354048,-1.9404840184286,-1.93944545298245,
-1.93738897003632,-1.90102614388073,-1.87074992148099,-1.85533314684365,
-1.84612791497397,-1.84351132092197,-1.84190766315403,-1.84045219646113,
-1.83858017318179,-1.83469679180234,-1.80154296690654,-1.74982937259077,
-1.74421856611467,-1.74271004643852,-1.74180594577909,-1.74099017516398,
-1.73993064020917,-1.73815933010255,-1.72735514048054,-1.70439012884219,
-1.67305662256649,-1.65629101659279,-1.64651148847798,-1.64383895580823,
-1.64222269372535,-1.64076974257636,-1.63892019615758,-1.63515151215182,
-1.58790917442322,-1.56059997381375,-1.55029208664757,-1.54452960001577,
-1.54300708017979,-1.54209981712395,-1.54128480595519,-1.54023101044057,
-1.5379525979515,-1.50134984868042,-1.47114510260012,-1.45582248480633,
-1.44665761493957,-1.44404472411244,-1.44244168675724,-1.44098570080046,
-1.43911149227542,-1.43521807701067,-1.40130370261824,-1.3525643572676,
-1.34502946737985,-1.34336738498775,-1.34242910577765,-1.34161939562965,
-1.34059770749452,-1.33860682053732,-1.32688561431306,-1.27545468040192,
-1.25738393664283,-1.24726463514544,-1.24447154191107,-1.24281230335258,
-1.24136535394898,-1.23958173806679,-1.23613759159561,-1.21201629567094,
-1.18120306699415,-1.14632197293124,-1.14401158940787,-1.14295174278235,
-1.14213583904628,-1.14123169975911,-1.13972336029486,-1.13411588506325,
-1.08241699620839,-1.04926718253818,-1.0453833455229,-1.04351101926021,
-1.04205527920723,-1.04045128192738,-1.03783404798626,-1.02862574995025,
-1.01320071476077,-0.982887803774222,-0.957295620588936,-0.946065516060176,
-0.944273320188244,-0.943207640651296,-0.942390945689695,-0.941489931865512,
-0.939995374066424,-0.934533082180191,-0.887611238046503,-0.849571437427456,
-0.845660028620719,-0.843782388966488,-0.842326054927193,-0.840724970402151,
-0.838120516777198,-0.829038179088114,-0.813902313534164,-0.783822644632941,
-0.746760732518862,-0.74448910253652,-0.743436610889292,-0.74262180673222,
-0.741713888237294,-0.740188335900028,-0.73439180546879,-0.723999269245736,
-0.696448691938276,-0.649637548726214,-0.645857574530095,-0.644005826143996,
-0.642552670498336,-0.640937754123617,-0.638271090318463,-0.62855309630134,
-0.611931668473617,-0.580682077105611,-0.559228038624472,-0.556703510775538,
-0.54651443390152,-0.544774340432485,-0.54372401574617,-0.542909541035049,
-0.542000508113727,-0.540469822111087,-0.53461543681671,-0.524075957486153,
-0.49579602973353,-0.44998021110871,-0.446172559634251,-0.444315380009893,
-0.442861654297179,-0.441249896171482,-0.438662228264077,-0.435576340281137,
-0.429545520260564,-0.414286797838816,-0.369349975765009,-0.347390837687695,
-0.345105554082086,-0.344034280513075,-0.343216799199853,-0.342318682001304,
-0.340836888481372,-0.335616987926469,-0.326596094793215,-0.304520764377662,
-0.265845573130727,-0.264252023667119,-0.249331763160838,-0.246425483574686,
-0.244583703065853,-0.243131681925652,-0.241511084198875,-0.238960219779077,
-0.229898875729598,-0.214747461188375,-0.187955806428541,-0.150423863246312,
-0.146171888935498,-0.144755801385972,-0.143960389335609,-0.143227882326773,
-0.142207331236432,-0.140155759901981,-0.126838913437522,-0.105241758511448,
-0.084928191612275,-0.0507289004174123,-0.0468327649219579,-0.0449580880292513,
-0.0435021114150737,-0.0418994612384761,-0.0402501570404879,-0.0378240370510129,
-0.028648498628005,-0.000592063050680485),.UNSPECIFIED.);
#828=B_SPLINE_CURVE_WITH_KNOTS('',3,(#26974,#26975,#26976,#26977,#26978,
#26979,#26980,#26981,#26982,#26983,#26984,#26985,#26986,#26987,#26988,#26989,
#26990,#26991,#26992,#26993,#26994,#26995,#26996,#26997,#26998,#26999,#27000,
#27001,#27002,#27003,#27004,#27005,#27006,#27007,#27008,#27009,#27010,#27011,
#27012,#27013,#27014,#27015,#27016,#27017,#27018,#27019,#27020,#27021,#27022,
#27023,#27024,#27025,#27026,#27027,#27028,#27029,#27030,#27031,#27032,#27033,
#27034,#27035,#27036,#27037,#27038,#27039,#27040,#27041,#27042,#27043,#27044,
#27045,#27046,#27047,#27048,#27049,#27050,#27051,#27052,#27053,#27054,#27055,
#27056,#27057,#27058,#27059,#27060,#27061,#27062,#27063,#27064,#27065,#27066,
#27067,#27068,#27069,#27070,#27071,#27072,#27073,#27074,#27075,#27076,#27077,
#27078,#27079,#27080,#27081,#27082,#27083,#27084,#27085,#27086,#27087,#27088,
#27089,#27090,#27091,#27092,#27093,#27094,#27095,#27096,#27097,#27098,#27099,
#27100,#27101,#27102,#27103,#27104,#27105,#27106,#27107,#27108,#27109,#27110,
#27111,#27112,#27113,#27114,#27115,#27116,#27117,#27118,#27119,#27120,#27121,
#27122,#27123,#27124,#27125,#27126,#27127,#27128,#27129,#27130,#27131,#27132,
#27133,#27134,#27135,#27136,#27137,#27138,#27139,#27140,#27141,#27142,#27143,
#27144,#27145,#27146,#27147,#27148,#27149,#27150,#27151,#27152,#27153,#27154,
#27155,#27156,#27157,#27158,#27159,#27160,#27161,#27162,#27163,#27164,#27165,
#27166,#27167,#27168,#27169,#27170,#27171,#27172,#27173,#27174,#27175,#27176,
#27177,#27178,#27179,#27180,#27181,#27182,#27183,#27184,#27185,#27186,#27187,
#27188,#27189,#27190,#27191,#27192,#27193,#27194,#27195,#27196,#27197,#27198,
#27199,#27200,#27201,#27202,#27203,#27204,#27205,#27206,#27207,#27208,#27209,
#27210,#27211,#27212,#27213,#27214,#27215,#27216,#27217,#27218,#27219,#27220,
#27221,#27222,#27223,#27224,#27225,#27226,#27227,#27228,#27229,#27230,#27231,
#27232,#27233,#27234,#27235,#27236,#27237,#27238,#27239,#27240,#27241,#27242,
#27243,#27244,#27245,#27246,#27247,#27248,#27249,#27250,#27251,#27252,#27253,
#27254,#27255,#27256,#27257,#27258,#27259,#27260,#27261,#27262,#27263,#27264,
#27265,#27266,#27267,#27268,#27269,#27270,#27271,#27272,#27273,#27274,#27275,
#27276,#27277,#27278,#27279,#27280,#27281,#27282,#27283,#27284,#27285,#27286,
#27287,#27288,#27289,#27290,#27291,#27292,#27293,#27294,#27295,#27296,#27297,
#27298,#27299,#27300,#27301,#27302,#27303,#27304,#27305,#27306,#27307,#27308,
#27309,#27310,#27311,#27312,#27313,#27314,#27315,#27316,#27317,#27318,#27319,
#27320,#27321,#27322,#27323,#27324,#27325,#27326,#27327,#27328,#27329,#27330,
#27331,#27332,#27333,#27334,#27335,#27336,#27337,#27338,#27339,#27340,#27341,
#27342,#27343,#27344,#27345,#27346,#27347,#27348,#27349,#27350,#27351,#27352,
#27353,#27354,#27355,#27356,#27357,#27358,#27359,#27360,#27361,#27362,#27363,
#27364,#27365,#27366,#27367,#27368,#27369,#27370,#27371,#27372,#27373,#27374,
#27375,#27376,#27377,#27378,#27379,#27380,#27381,#27382,#27383,#27384,#27385,
#27386,#27387,#27388,#27389,#27390,#27391,#27392,#27393,#27394,#27395,#27396,
#27397,#27398,#27399,#27400,#27401,#27402,#27403,#27404,#27405,#27406,#27407,
#27408,#27409,#27410,#27411,#27412,#27413,#27414,#27415,#27416,#27417,#27418,
#27419,#27420,#27421,#27422,#27423,#27424,#27425,#27426,#27427,#27428,#27429,
#27430,#27431,#27432,#27433,#27434,#27435,#27436,#27437,#27438,#27439,#27440,
#27441,#27442,#27443,#27444,#27445,#27446,#27447,#27448,#27449,#27450,#27451,
#27452,#27453),.UNSPECIFIED.,.F.,.F.,(4,2,2,2,2,2,2,2,2,2,2,2,2,2,2,2,2,
2,2,2,2,2,2,2,2,2,2,2,2,2,2,2,2,2,2,2,2,2,2,2,2,2,2,2,2,2,2,2,2,2,2,2,2,
2,2,2,2,2,2,2,2,2,2,2,2,2,2,2,2,2,2,2,2,2,2,2,2,2,2,2,2,2,2,2,2,2,2,2,2,
2,2,2,2,2,2,2,2,2,2,2,2,2,2,2,2,2,2,2,2,2,2,2,2,2,2,2,2,2,2,2,2,2,2,2,2,
2,2,2,2,2,2,2,2,2,2,2,2,2,2,2,2,2,2,2,2,2,2,2,2,2,2,2,2,2,2,2,2,2,2,2,2,
2,2,2,2,2,2,2,2,2,2,2,2,2,2,2,2,2,2,2,2,2,2,2,2,2,2,2,2,2,2,2,2,2,2,2,2,
2,2,2,2,2,2,2,2,2,2,2,2,2,2,2,2,2,2,2,2,2,2,2,2,2,2,2,2,2,2,2,2,2,2,2,2,
2,2,2,2,2,2,4),(-2.51332395769527,-2.46474828361658,-2.46116306924221,-2.4593699194601,
-2.45787086751029,-2.45696913561548,-2.45615318554831,-2.45509034196855,
-2.45330692094798,-2.44224479945897,-2.43865158241955,-2.4313375094352,
-2.40560667303955,-2.38788740616807,-2.36529844435069,-2.36045418606504,
-2.35885307230337,-2.35749504545638,-2.35604568463502,-2.3542249422401,
-2.35138597987877,-2.33750991168437,-2.33465826145439,-2.32645813380707,
-2.2982124093394,-2.27465882310025,-2.26519882645719,-2.25980042106438,
-2.25829969436402,-2.25739757544443,-2.2565817103599,-2.25551955520539,
-2.25373852679323,-2.24272604101519,-2.22116599881277,-2.18310722642188,
-2.16998954510344,-2.1645735891904,-2.16049435664933,-2.15858654898353,
-2.1571208244371,-2.15574202518615,-2.15345053968071,-2.14751565193713,
-2.14609830693586,-2.14456286037487,-2.08074844137598,-2.06725950949993,
-2.06032705747805,-2.05869891913456,-2.05776835130141,-2.0569580713294,
-2.05592626014152,-2.05428471346218,-2.0458251775807,-1.98651126146365,
-1.97131764782859,-1.96220996706017,-1.95960352996115,-1.95800235075195,
-1.95654667051234,-1.95467091421605,-1.95076722311105,-1.91243527507579,
-1.86576952138576,-1.86032089928283,-1.85882793412789,-1.85792744609472,
-1.85711091709718,-1.85604504925556,-1.85425166825216,-1.84298888763837,
-1.81745195756351,-1.78717848952787,-1.77176304952694,-1.76255863335647,
-1.75994228034119,-1.75833877224081,-1.75688344265723,-1.75501159750981,
-1.75112859210124,-1.71797872664734,-1.66627032069229,-1.66065903308598,
-1.65915056135955,-1.65824652474706,-1.65743083657232,-1.65637144127167,
-1.65406268949003,-1.61913161913508,-1.58837720144721,-1.57235461573101,
-1.56288888624091,-1.56024654480853,-1.55863710974485,-1.55718290052906,
-1.55532153204203,-1.55149261146515,-1.54768589551934,-1.50327062482036,
-1.47673460526656,-1.46664583848783,-1.46097090378476,-1.45945649361129,
-1.45855110408222,-1.45773572688925,-1.45667875699208,-1.45438310506596,
-1.4187008248078,-1.38819432029752,-1.37248862920222,-1.36315844401215,
-1.3605292937554,-1.3589227484772,-1.35746779937504,-1.3556008208601,-1.35174366963999,
-1.32047334928139,-1.27012925756055,-1.26161719079115,-1.25989298897333,
-1.25894118423916,-1.25813272089357,-1.25712890938093,-1.2551594889612,
-1.24084581064947,-1.21614110238151,-1.1692000228423,-1.16283663969254,
-1.16047812651329,-1.1590859192022,-1.15762562289127,-1.15571895623606,
-1.15165733095664,-1.11591837415816,-1.07808917102712,-1.06259512034142,
-1.06042915914553,-1.05938575513482,-1.05857412522969,-1.05765059287603,
-1.05605500406282,-1.04942639686582,-1.03683633828169,-0.997506801881617,
-0.965778788437095,-0.961914603358767,-0.960046153125368,-0.958590922179214,
-0.956984944443865,-0.95435871902511,-0.945059624745885,-0.929424297942888,
-0.898944744922087,-0.863071237870986,-0.861005321815355,-0.859964268948691,
-0.859203074905411,-0.858369811136605,-0.857188625769793,-0.854251187562669,
-0.81563597083389,-0.769750962378527,-0.763583330847972,-0.76111395999698,
-0.759699901105109,-0.758392347772969,-0.756615561898078,-0.753203749833357,
-0.730122509032019,-0.699881529130821,-0.689482833722177,-0.663424074653541,
-0.66106941433786,-0.660001407686329,-0.659184392516423,-0.658284604894092,
-0.656795432413241,-0.651388791851969,-0.641961932862458,-0.618180764598795,
-0.569929693877353,-0.565703153692123,-0.562564867068603,-0.560673507729573,
-0.559210807901309,-0.557631538481867,-0.555125156250188,-0.546963296060805,
-0.533874216787375,-0.481472992293541,-0.46348392730341,-0.461467305363734,
-0.460438762915992,-0.459680755320231,-0.458844406858479,-0.457647398334057,
-0.454611028127832,-0.437439505877787,-0.391869766866492,-0.380384043658242,
-0.365509490772975,-0.362605889808877,-0.360764855569276,-0.359312819313376,
-0.357724058518867,-0.355151434155842,-0.352071998322744,-0.346058870197086,
-0.33086419188426,-0.295248831152963,-0.279751570060649,-0.263686141486495,
-0.261501451205079,-0.26045438554456,-0.259642374119812,-0.258721119785569,
-0.257135779989148,-0.250636286419062,-0.238399815691751,-0.192238898274493,
-0.180764963804175,-0.1658089436138,-0.162900356336665,-0.161057822386082,
-0.15960565640638,-0.158248572266005,-0.156659019389015,-0.151938423830255,
-0.130901259995497,-0.113205627287674,-0.0669098856791247,-0.062628526562833,
-0.0612084632076815,-0.0604122082424815,-0.0596798606573647,-0.0586609252498538,
-0.0566175252987397,-0.0539782882255648,-0.000592841608242558),
 .UNSPECIFIED.);
#829=B_SPLINE_CURVE_WITH_KNOTS('',3,(#28433,#28434,#28435,#28436,#28437,
#28438,#28439,#28440,#28441,#28442,#28443,#28444,#28445,#28446,#28447,#28448,
#28449,#28450,#28451,#28452,#28453,#28454,#28455,#28456,#28457,#28458,#28459,
#28460,#28461,#28462,#28463,#28464,#28465,#28466,#28467,#28468,#28469,#28470,
#28471,#28472,#28473,#28474,#28475,#28476,#28477,#28478,#28479,#28480,#28481,
#28482,#28483,#28484,#28485,#28486,#28487,#28488,#28489,#28490,#28491,#28492,
#28493,#28494,#28495,#28496,#28497,#28498,#28499,#28500,#28501,#28502,#28503,
#28504,#28505,#28506,#28507,#28508,#28509,#28510,#28511,#28512,#28513,#28514,
#28515,#28516,#28517),.UNSPECIFIED.,.F.,.F.,(4,3,3,3,3,3,3,3,3,3,3,3,3,
3,3,3,3,3,3,3,3,3,3,3,3,3,3,3,4),(0.,0.0170098241792627,0.0424826395433647,
0.0682962769238695,0.0913512330686695,0.0964562008288006,0.121594894041372,
0.146637962453068,0.171052849770118,0.182468804955695,0.186977115896109,
0.211109611306723,0.234543633473231,0.251322674972674,0.264602698464612,
0.269910529014969,0.273918093975593,0.297399013310025,0.321140231227419,
0.342399840472737,0.351520822404548,0.355793196577609,0.378788067002577,
0.400130399022457,0.407097962113538,0.413428647993403,0.435399867888606,
0.457192780488514,0.463803050843695),.UNSPECIFIED.);
#830=B_SPLINE_CURVE_WITH_KNOTS('',3,(#28519,#28520,#28521,#28522,#28523,
#28524,#28525,#28526,#28527,#28528,#28529,#28530,#28531,#28532,#28533,#28534,
#28535,#28536,#28537,#28538,#28539,#28540,#28541,#28542,#28543,#28544,#28545,
#28546,#28547,#28548,#28549,#28550,#28551,#28552,#28553,#28554,#28555,#28556,
#28557,#28558,#28559,#28560,#28561,#28562,#28563,#28564,#28565,#28566,#28567,
#28568,#28569,#28570,#28571,#28572,#28573,#28574,#28575,#28576,#28577,#28578,
#28579,#28580,#28581,#28582,#28583,#28584,#28585,#28586,#28587,#28588,#28589,
#28590,#28591,#28592,#28593,#28594,#28595,#28596,#28597,#28598,#28599,#28600,
#28601,#28602,#28603,#28604,#28605,#28606),.UNSPECIFIED.,.F.,.F.,(4,3,3,
3,3,3,3,3,3,3,3,3,3,3,3,3,3,3,3,3,3,3,3,3,3,3,3,3,3,4),(-0.463803050843694,
-0.449790106353243,-0.427990665865324,-0.416071534428731,-0.41053262250662,
-0.406065555453362,-0.383649085978725,-0.360658636559499,-0.357654820809351,
-0.351701489295335,-0.328241177350174,-0.304498488949914,-0.280901268184384,
-0.274909285295064,-0.270960497067351,-0.246531766448708,-0.235762608198985,
-0.211934962645635,-0.188107317092285,-0.183891756486896,-0.180496953448606,
-0.156079531689618,-0.131226048105235,-0.106117747812671,-0.0959943972028356,
-0.0910045065255718,-0.0652633795699505,-0.0394823888695457,-0.0142475767317681,
0.),.UNSPECIFIED.);
#831=B_SPLINE_CURVE_WITH_KNOTS('',3,(#28607,#28608,#28609,#28610),
 .UNSPECIFIED.,.F.,.F.,(4,4),(-0.0140491024708372,0.),.UNSPECIFIED.);
#832=B_SPLINE_CURVE_WITH_KNOTS('',3,(#29575,#29576,#29577,#29578,#29579,
#29580,#29581,#29582,#29583,#29584,#29585,#29586,#29587,#29588,#29589,#29590,
#29591,#29592,#29593,#29594,#29595,#29596,#29597,#29598,#29599,#29600,#29601,
#29602,#29603,#29604,#29605,#29606,#29607,#29608,#29609,#29610,#29611,#29612,
#29613,#29614,#29615,#29616,#29617,#29618,#29619,#29620,#29621,#29622,#29623,
#29624,#29625,#29626,#29627,#29628,#29629,#29630,#29631,#29632,#29633,#29634,
#29635,#29636,#29637,#29638,#29639,#29640,#29641,#29642,#29643,#29644,#29645,
#29646,#29647,#29648,#29649,#29650,#29651,#29652,#29653,#29654,#29655,#29656,
#29657,#29658,#29659,#29660,#29661,#29662,#29663,#29664,#29665,#29666,#29667,
#29668),.UNSPECIFIED.,.F.,.F.,(4,3,3,3,3,3,3,3,3,3,3,3,3,3,3,3,3,3,3,3,
3,3,3,3,3,3,3,3,3,3,3,4),(0.,0.0139666598681629,0.0354492048263863,0.0576250686896674,
0.0685265859231677,0.0770896876198345,0.0816411102851959,0.104504088810244,
0.127761520890668,0.145893898052724,0.154960086633753,0.160934662671419,
0.164026275214781,0.18805909179815,0.211994708341173,0.227291834558635,
0.241947905204957,0.246523482387956,0.250638107839803,0.274355640976877,
0.298561537524763,0.323231579885226,0.329929774781174,0.335709929194683,
0.339916350947803,0.365091941017713,0.390436885206924,0.397901145376386,
0.402692087010053,0.428435843892961,0.45394520469992,0.461788964899784),
 .UNSPECIFIED.);
#833=B_SPLINE_CURVE_WITH_KNOTS('',3,(#29669,#29670,#29671,#29672,#29673,
#29674,#29675,#29676,#29677,#29678,#29679,#29680,#29681,#29682,#29683,#29684,
#29685,#29686,#29687,#29688,#29689,#29690,#29691,#29692,#29693,#29694,#29695,
#29696,#29697,#29698,#29699,#29700,#29701,#29702,#29703,#29704,#29705,#29706,
#29707,#29708,#29709,#29710,#29711,#29712,#29713,#29714,#29715,#29716,#29717,
#29718,#29719,#29720,#29721,#29722,#29723,#29724,#29725,#29726,#29727,#29728,
#29729,#29730,#29731,#29732,#29733,#29734,#29735,#29736,#29737,#29738,#29739,
#29740,#29741,#29742,#29743,#29744,#29745,#29746,#29747,#29748,#29749,#29750,
#29751,#29752,#29753,#29754,#29755,#29756),.UNSPECIFIED.,.F.,.F.,(4,3,3,
3,3,3,3,3,3,3,3,3,3,3,3,3,3,3,3,3,3,3,3,3,3,3,3,3,3,4),(-0.461788964899782,
-0.444855550134428,-0.419152893345616,-0.406271531682089,-0.400199974555711,
-0.395168529208714,-0.369855739683799,-0.344556768713737,-0.341034351191149,
-0.33606198793914,-0.331746083665484,-0.307015393549491,-0.282570742889413,
-0.258867857593402,-0.248690711882788,-0.244217611698179,-0.220731256812843,
-0.211799399012893,-0.187739266633416,-0.164360764291082,-0.158727229016938,
-0.135371887906763,-0.112003733335168,-0.0891062190630772,-0.0803325096073959,
-0.0766178882203682,-0.0541551504458856,-0.0320568974934828,-0.0106664530521837,
-1.30075470011633E-14),.UNSPECIFIED.);
#834=B_SPLINE_CURVE_WITH_KNOTS('',3,(#29760,#29761,#29762,#29763,#29764,
#29765,#29766,#29767,#29768,#29769,#29770,#29771,#29772,#29773,#29774,#29775,
#29776,#29777,#29778,#29779,#29780,#29781,#29782,#29783,#29784,#29785,#29786,
#29787,#29788,#29789,#29790,#29791,#29792,#29793),.UNSPECIFIED.,.F.,.F.,
(4,2,2,2,2,2,2,2,2,2,2,2,2,2,2,2,4),(-0.22533843255893,-0.216182593404494,
-0.18091865643817,-0.156950339943155,-0.140921103226519,-0.129823782034954,
-0.118153571207391,-0.114481377626862,-0.112295015626103,-0.110369884265133,
-0.107992250297265,-0.103463255811762,-0.0921160616035588,-0.0805188447194219,
-0.0652099958826858,-0.043221973238958,0.),.UNSPECIFIED.);
#835=B_SPLINE_CURVE_WITH_KNOTS('',3,(#29802,#29803,#29804,#29805,#29806,
#29807,#29808,#29809,#29810,#29811,#29812,#29813,#29814,#29815,#29816,#29817,
#29818,#29819,#29820,#29821,#29822,#29823,#29824,#29825,#29826,#29827,#29828,
#29829,#29830,#29831,#29832,#29833,#29834,#29835),.UNSPECIFIED.,.F.,.F.,
(4,2,2,2,2,2,2,2,2,2,2,2,2,2,2,2,4),(-0.225338432559487,-0.216182593405045,
-0.180918656438646,-0.156950339943541,-0.140921103226827,-0.129823782035196,
-0.118153571207555,-0.114481377627008,-0.112295015626236,-0.110369884265256,
-0.107992250297385,-0.103463255811877,-0.0921160616036507,-0.0805188447194852,
-0.0652099958827053,-0.0432219732389482,0.),.UNSPECIFIED.);
#836=B_SPLINE_CURVE_WITH_KNOTS('',3,(#29844,#29845,#29846,#29847,#29848,
#29849,#29850,#29851,#29852,#29853,#29854,#29855,#29856,#29857,#29858,#29859,
#29860,#29861,#29862,#29863,#29864,#29865,#29866,#29867,#29868,#29869,#29870,
#29871,#29872,#29873,#29874,#29875,#29876,#29877),.UNSPECIFIED.,.F.,.F.,
(4,2,2,2,2,2,2,2,2,2,2,2,2,2,2,2,4),(-0.225338432559843,-0.216182593405344,
-0.180918656438743,-0.156950339943502,-0.140921103226703,-0.129823782035015,
-0.118153571207324,-0.114481377626746,-0.112295015625973,-0.110369884265002,
-0.107992250297144,-0.103463255811654,-0.0921160616034753,-0.0805188447193631,
-0.0652099958826622,-0.0432219732389638,0.),.UNSPECIFIED.);
#837=B_SPLINE_CURVE_WITH_KNOTS('',3,(#29886,#29887,#29888,#29889,#29890,
#29891,#29892,#29893,#29894,#29895,#29896,#29897,#29898,#29899,#29900,#29901,
#29902,#29903,#29904,#29905,#29906,#29907,#29908,#29909,#29910,#29911,#29912,
#29913,#29914,#29915,#29916,#29917,#29918,#29919),.UNSPECIFIED.,.F.,.F.,
(4,2,2,2,2,2,2,2,2,2,2,2,2,2,2,2,4),(-0.225338432559394,-0.216182593404911,
-0.180918656438384,-0.15695033994328,-0.140921103226616,-0.12982378203502,
-0.118153571207424,-0.114481377626883,-0.112295015626127,-0.110369884265165,
-0.107992250297307,-0.103463255811807,-0.0921160616035986,-0.0805188447194506,
-0.0652099958826983,-0.0432219732389566,0.),.UNSPECIFIED.);
#838=B_SPLINE_CURVE_WITH_KNOTS('',3,(#29928,#29929,#29930,#29931,#29932,
#29933,#29934,#29935,#29936,#29937,#29938,#29939,#29940,#29941,#29942,#29943,
#29944,#29945,#29946,#29947,#29948,#29949,#29950,#29951,#29952,#29953,#29954,
#29955,#29956,#29957,#29958,#29959,#29960,#29961),.UNSPECIFIED.,.F.,.F.,
(4,2,2,2,2,2,2,2,2,2,2,2,2,2,2,2,4),(-0.225338432559585,-0.216182593405109,
-0.180918656438604,-0.156950339943452,-0.140921103226724,-0.129823782035084,
-0.118153571207435,-0.114481377626872,-0.112295015626095,-0.110369884265119,
-0.107992250297262,-0.103463255811765,-0.0921160616035663,-0.0805188447194236,
-0.065209995882676,-0.0432219732389438,0.),.UNSPECIFIED.);
#839=B_SPLINE_CURVE_WITH_KNOTS('',3,(#29970,#29971,#29972,#29973,#29974,
#29975,#29976,#29977,#29978,#29979,#29980,#29981,#29982,#29983,#29984,#29985,
#29986,#29987,#29988,#29989,#29990,#29991,#29992,#29993,#29994,#29995,#29996,
#29997,#29998,#29999,#30000,#30001,#30002,#30003),.UNSPECIFIED.,.F.,.F.,
(4,2,2,2,2,2,2,2,2,2,2,2,2,2,2,2,4),(-0.225338432560591,-0.216182593406049,
-0.180918656439286,-0.156950339943944,-0.140921103227085,-0.129823782035365,
-0.118153571207645,-0.11448137762707,-0.112295015626274,-0.110369884265278,
-0.107992250297404,-0.103463255811892,-0.0921160616036589,-0.0805188447194971,
-0.0652099958827318,-0.043221973238974,0.),.UNSPECIFIED.);
#840=B_SPLINE_CURVE_WITH_KNOTS('',3,(#30012,#30013,#30014,#30015,#30016,
#30017,#30018,#30019,#30020,#30021,#30022,#30023,#30024,#30025,#30026,#30027,
#30028,#30029,#30030,#30031,#30032,#30033,#30034,#30035,#30036,#30037,#30038,
#30039,#30040,#30041,#30042,#30043,#30044,#30045),.UNSPECIFIED.,.F.,.F.,
(4,2,2,2,2,2,2,2,2,2,2,2,2,2,2,2,4),(-0.225338432560395,-0.21618259340586,
-0.180918656439119,-0.156950339943809,-0.140921103226983,-0.129823782035285,
-0.118153571207591,-0.114481377627025,-0.112295015626251,-0.110369884265274,
-0.107992250297403,-0.103463255811889,-0.0921160616036515,-0.0805188447194844,
-0.0652099958827251,-0.0432219732389749,0.),.UNSPECIFIED.);
#841=B_SPLINE_CURVE_WITH_KNOTS('',3,(#30054,#30055,#30056,#30057,#30058,
#30059,#30060,#30061,#30062,#30063,#30064,#30065,#30066,#30067,#30068,#30069,
#30070,#30071,#30072,#30073,#30074,#30075,#30076,#30077,#30078,#30079,#30080,
#30081,#30082,#30083,#30084,#30085,#30086,#30087),.UNSPECIFIED.,.F.,.F.,
(4,2,2,2,2,2,2,2,2,2,2,2,2,2,2,2,4),(-0.225338432558288,-0.216182593403889,
-0.180918656437663,-0.156950339942723,-0.140921103226146,-0.129823782034617,
-0.118153571207095,-0.114481377626574,-0.112295015625834,-0.110369884264885,
-0.107992250297034,-0.103463255811553,-0.0921160616033991,-0.0805188447193084,
-0.0652099958826347,-0.0432219732389551,0.),.UNSPECIFIED.);
#842=B_SPLINE_CURVE_WITH_KNOTS('',3,(#30096,#30097,#30098,#30099,#30100,
#30101,#30102,#30103,#30104,#30105,#30106,#30107,#30108,#30109,#30110,#30111,
#30112,#30113,#30114,#30115,#30116,#30117,#30118,#30119,#30120,#30121,#30122,
#30123,#30124,#30125,#30126,#30127,#30128,#30129),.UNSPECIFIED.,.F.,.F.,
(4,2,2,2,2,2,2,2,2,2,2,2,2,2,2,2,4),(-0.225338432559953,-0.216182593405462,
-0.180918656438873,-0.156950339943631,-0.14092110322683,-0.129823782035144,
-0.118153571207449,-0.114481377626881,-0.112295015626082,-0.110369884265086,
-0.107992250297227,-0.103463255811732,-0.0921160616035443,-0.0805188447194133,
-0.0652099958826861,-0.043221973238957,0.),.UNSPECIFIED.);
#843=B_SPLINE_CURVE_WITH_KNOTS('',3,(#30138,#30139,#30140,#30141,#30142,
#30143,#30144,#30145,#30146,#30147,#30148,#30149,#30150,#30151,#30152,#30153,
#30154,#30155,#30156,#30157),.UNSPECIFIED.,.F.,.F.,(4,2,2,2,2,2,2,2,2,4),
(-0.475220070020625,-0.441790011987763,-0.414059721280184,-0.394580184974582,
-0.380386463975323,-0.36989470508298,-0.361499869486035,-0.358160690967077,
-0.355853630537146,-0.355774891916115),.UNSPECIFIED.);
#844=B_SPLINE_CURVE_WITH_KNOTS('',3,(#30164,#30165,#30166,#30167,#30168,
#30169,#30170,#30171,#30172,#30173,#30174,#30175,#30176,#30177,#30178,#30179,
#30180,#30181),.UNSPECIFIED.,.F.,.F.,(4,2,2,2,2,2,2,2,4),(-0.355774891916115,
-0.353603695467602,-0.350430609151558,-0.343375404346486,-0.330600159177977,
-0.316000108246756,-0.296556237452606,-0.264901408087306,-0.225338432559845),
 .UNSPECIFIED.);
#845=B_SPLINE_CURVE_WITH_KNOTS('',3,(#30185,#30186,#30187,#30188,#30189,
#30190,#30191,#30192,#30193,#30194,#30195,#30196,#30197,#30198,#30199,#30200,
#30201,#30202,#30203,#30204,#30205,#30206,#30207,#30208,#30209,#30210,#30211,
#30212,#30213,#30214,#30215,#30216,#30217,#30218),.UNSPECIFIED.,.F.,.F.,
(4,2,2,2,2,2,2,2,2,2,2,2,2,2,2,2,4),(-0.225338432559478,-0.216182593404956,
-0.180918656438277,-0.156950339943081,-0.140921103226373,-0.129823782034755,
-0.118153571207149,-0.114481377626612,-0.112295015625852,-0.110369884264885,
-0.107992250297023,-0.103463255811539,-0.0921160616033758,-0.0805188447192899,
-0.0652099958826333,-0.0432219732389767,0.),.UNSPECIFIED.);
#846=B_SPLINE_CURVE_WITH_KNOTS('',3,(#30227,#30228,#30229,#30230,#30231,
#30232,#30233,#30234,#30235,#30236,#30237,#30238,#30239,#30240,#30241,#30242,
#30243,#30244,#30245,#30246,#30247,#30248,#30249,#30250,#30251,#30252,#30253,
#30254,#30255,#30256,#30257,#30258,#30259,#30260),.UNSPECIFIED.,.F.,.F.,
(4,2,2,2,2,2,2,2,2,2,2,2,2,2,2,2,4),(-0.225338432560806,-0.216182593406188,
-0.180918656439175,-0.156950339943746,-0.140921103226884,-0.12982378203515,
-0.118153571207415,-0.114481377626832,-0.11229501562605,-0.110369884265066,
-0.107992250297192,-0.103463255811689,-0.0921160616035007,-0.0805188447193768,
-0.0652099958826869,-0.0432219732389717,0.),.UNSPECIFIED.);
#847=B_SPLINE_CURVE_WITH_KNOTS('',3,(#30269,#30270,#30271,#30272,#30273,
#30274,#30275,#30276,#30277,#30278,#30279,#30280,#30281,#30282,#30283,#30284,
#30285,#30286,#30287,#30288,#30289,#30290,#30291,#30292,#30293,#30294,#30295,
#30296,#30297,#30298,#30299,#30300,#30301,#30302),.UNSPECIFIED.,.F.,.F.,
(4,2,2,2,2,2,2,2,2,2,2,2,2,2,2,2,4),(-0.225338432559276,-0.21618259340483,
-0.180918656438373,-0.156950339943235,-0.140921103226506,-0.129823782034874,
-0.118153571207256,-0.114481377626715,-0.112295015625943,-0.11036988426497,
-0.107992250297116,-0.103463255811614,-0.0921160616034403,-0.0805188447193372,
-0.065209995882666,-0.0432219732389822,0.),.UNSPECIFIED.);
#848=B_SPLINE_CURVE_WITH_KNOTS('',3,(#30311,#30312,#30313,#30314,#30315,
#30316,#30317,#30318,#30319,#30320,#30321,#30322,#30323,#30324,#30325,#30326,
#30327,#30328,#30329,#30330,#30331,#30332,#30333,#30334,#30335,#30336,#30337,
#30338,#30339,#30340,#30341,#30342,#30343,#30344),.UNSPECIFIED.,.F.,.F.,
(4,2,2,2,2,2,2,2,2,2,2,2,2,2,2,2,4),(-0.225338432560726,-0.21618259340622,
-0.180918656439635,-0.156950339944368,-0.140921103227535,-0.129823782035824,
-0.118153571208108,-0.114481377627516,-0.112295015626722,-0.110369884265733,
-0.107992250297856,-0.103463255812308,-0.092116061603986,-0.0805188447197293,
-0.0652099958828215,-0.0432219732389566,0.),.UNSPECIFIED.);
#849=B_SPLINE_CURVE_WITH_KNOTS('',3,(#30353,#30354,#30355,#30356,#30357,
#30358,#30359,#30360,#30361,#30362,#30363,#30364,#30365,#30366,#30367,#30368,
#30369,#30370,#30371,#30372,#30373,#30374,#30375,#30376,#30377,#30378,#30379,
#30380,#30381,#30382,#30383,#30384,#30385,#30386),.UNSPECIFIED.,.F.,.F.,
(4,2,2,2,2,2,2,2,2,2,2,2,2,2,2,2,4),(-0.225338432561249,-0.216182593406692,
-0.180918656439827,-0.156950339944366,-0.140921103227389,-0.129823782035595,
-0.1181535712078,-0.114481377627208,-0.112295015626422,-0.110369884265441,
-0.107992250297571,-0.103463255812037,-0.0921160616037674,-0.0805188447195652,
-0.0652099958827499,-0.0432219732389706,0.),.UNSPECIFIED.);
#850=B_SPLINE_CURVE_WITH_KNOTS('',3,(#30395,#30396,#30397,#30398,#30399,
#30400,#30401,#30402,#30403,#30404,#30405,#30406,#30407,#30408,#30409,#30410,
#30411,#30412,#30413,#30414,#30415,#30416,#30417,#30418,#30419,#30420,#30421,
#30422,#30423,#30424,#30425,#30426,#30427,#30428),.UNSPECIFIED.,.F.,.F.,
(4,2,2,2,2,2,2,2,2,2,2,2,2,2,2,2,4),(-0.225338432560144,-0.216182593405564,
-0.180918656438685,-0.156950339943354,-0.140921103226555,-0.129823782034876,
-0.118153571207208,-0.114481377626656,-0.112295015625892,-0.110369884264924,
-0.107992250297063,-0.103463255811581,-0.0921160616034071,-0.0805188447193141,
-0.0652099958826549,-0.0432219732389826,0.),.UNSPECIFIED.);
#851=B_SPLINE_CURVE_WITH_KNOTS('',3,(#30437,#30438,#30439,#30440,#30441,
#30442,#30443,#30444,#30445,#30446,#30447,#30448,#30449,#30450,#30451,#30452,
#30453,#30454,#30455,#30456,#30457,#30458,#30459,#30460,#30461,#30462,#30463,
#30464,#30465,#30466,#30467,#30468,#30469,#30470),.UNSPECIFIED.,.F.,.F.,
(4,2,2,2,2,2,2,2,2,2,2,2,2,2,2,2,4),(-0.225338432560541,-0.216182593406004,
-0.180918656439237,-0.156950339943896,-0.140921103227052,-0.129823782035331,
-0.118153571207599,-0.114481377627011,-0.112295015626233,-0.11036988426526,
-0.107992250297404,-0.1034632558119,-0.092116061603665,-0.0805188447195002,
-0.0652099958827254,-0.0432219732389589,0.),.UNSPECIFIED.);
#852=B_SPLINE_CURVE_WITH_KNOTS('',3,(#30479,#30480,#30481,#30482,#30483,
#30484,#30485,#30486,#30487,#30488,#30489,#30490,#30491,#30492,#30493,#30494,
#30495,#30496,#30497,#30498,#30499,#30500,#30501,#30502,#30503,#30504,#30505,
#30506,#30507,#30508,#30509,#30510,#30511,#30512),.UNSPECIFIED.,.F.,.F.,
(4,2,2,2,2,2,2,2,2,2,2,2,2,2,2,2,4),(-0.225338432560968,-0.216182593406323,
-0.180918656439217,-0.15695033994371,-0.140921103226774,-0.129823782034991,
-0.118153571207195,-0.114481377626593,-0.112295015625806,-0.11036988426482,
-0.107992250296948,-0.103463255811474,-0.0921160616033362,-0.0805188447192614,
-0.0652099958826226,-0.0432219732389696,0.),.UNSPECIFIED.);
#853=B_SPLINE_CURVE_WITH_KNOTS('',3,(#30521,#30522,#30523,#30524,#30525,
#30526,#30527,#30528,#30529,#30530,#30531,#30532,#30533,#30534,#30535,#30536,
#30537,#30538,#30539,#30540,#30541,#30542,#30543,#30544,#30545,#30546,#30547,
#30548,#30549,#30550,#30551,#30552,#30553,#30554),.UNSPECIFIED.,.F.,.F.,
(4,2,2,2,2,2,2,2,2,2,2,2,2,2,2,2,4),(-0.225338432559187,-0.216182593404789,
-0.180918656438548,-0.156950339943463,-0.140921103226717,-0.129823782035056,
-0.118153571207385,-0.114481377626823,-0.112295015626038,-0.110369884265052,
-0.107992250297197,-0.103463255811722,-0.0921160616035283,-0.0805188447194076,
-0.0652099958826757,-0.0432219732389471,0.),.UNSPECIFIED.);
#854=B_SPLINE_CURVE_WITH_KNOTS('',3,(#30563,#30564,#30565,#30566,#30567,
#30568,#30569,#30570,#30571,#30572,#30573,#30574,#30575,#30576,#30577,#30578,
#30579,#30580,#30581,#30582,#30583,#30584,#30585,#30586,#30587,#30588,#30589,
#30590,#30591,#30592,#30593,#30594,#30595,#30596),.UNSPECIFIED.,.F.,.F.,
(4,2,2,2,2,2,2,2,2,2,2,2,2,2,2,2,4),(-0.225338432560443,-0.216182593405909,
-0.180918656439139,-0.156950339943792,-0.140921103226935,-0.1298237820352,
-0.118153571207452,-0.114481377626862,-0.112295015626078,-0.110369884265102,
-0.10799225029725,-0.103463255811758,-0.092116061603562,-0.0805188447194234,
-0.0652099958826702,-0.0432219732389456,0.),.UNSPECIFIED.);
#855=B_SPLINE_CURVE_WITH_KNOTS('',3,(#30605,#30606,#30607,#30608,#30609,
#30610,#30611,#30612,#30613,#30614,#30615,#30616,#30617,#30618,#30619,#30620,
#30621,#30622,#30623,#30624,#30625,#30626,#30627,#30628,#30629,#30630,#30631,
#30632,#30633,#30634,#30635,#30636,#30637,#30638),.UNSPECIFIED.,.F.,.F.,
(4,2,2,2,2,2,2,2,2,2,2,2,2,2,2,2,4),(-0.225338432559121,-0.216182593404619,
-0.18091865643809,-0.156950339942956,-0.14092110322627,-0.129823782034653,
-0.118153571207027,-0.114481377626479,-0.112295015625724,-0.110369884264759,
-0.107992250296894,-0.103463255811428,-0.0921160616033008,-0.0805188447192374,
-0.0652099958825975,-0.0432219732389517,0.),.UNSPECIFIED.);
#856=B_SPLINE_CURVE_WITH_KNOTS('',3,(#30647,#30648,#30649,#30650,#30651,
#30652,#30653,#30654,#30655,#30656,#30657,#30658,#30659,#30660,#30661,#30662,
#30663,#30664,#30665,#30666,#30667,#30668,#30669,#30670,#30671,#30672,#30673,
#30674,#30675,#30676,#30677,#30678,#30679,#30680),.UNSPECIFIED.,.F.,.F.,
(4,2,2,2,2,2,2,2,2,2,2,2,2,2,2,2,4),(-0.225338432559561,-0.216182593405078,
-0.180918656438519,-0.156950339943348,-0.140921103226635,-0.12982378203501,
-0.118153571207387,-0.114481377626829,-0.112295015626078,-0.110369884265122,
-0.10799225029726,-0.103463255811752,-0.0921160616035431,-0.0805188447194093,
-0.0652099958827019,-0.0432219732389723,0.),.UNSPECIFIED.);
#857=B_SPLINE_CURVE_WITH_KNOTS('',3,(#30689,#30690,#30691,#30692,#30693,
#30694,#30695,#30696,#30697,#30698,#30699,#30700,#30701,#30702,#30703,#30704,
#30705,#30706,#30707,#30708,#30709,#30710,#30711,#30712,#30713,#30714,#30715,
#30716,#30717,#30718,#30719,#30720,#30721,#30722),.UNSPECIFIED.,.F.,.F.,
(4,2,2,2,2,2,2,2,2,2,2,2,2,2,2,2,4),(-0.225338432559738,-0.216182593405211,
-0.180918656438537,-0.156950339943277,-0.140921103226497,-0.129823782034835,
-0.11815357120718,-0.114481377626615,-0.112295015625857,-0.110369884264898,
-0.107992250297039,-0.103463255811543,-0.0921160616033831,-0.0805188447192948,
-0.0652099958826484,-0.0432219732389855,0.),.UNSPECIFIED.);
#858=B_SPLINE_CURVE_WITH_KNOTS('',3,(#30731,#30732,#30733,#30734,#30735,
#30736,#30737,#30738,#30739,#30740,#30741,#30742,#30743,#30744,#30745,#30746,
#30747,#30748,#30749,#30750,#30751,#30752,#30753,#30754,#30755,#30756,#30757,
#30758,#30759,#30760,#30761,#30762,#30763,#30764),.UNSPECIFIED.,.F.,.F.,
(4,2,2,2,2,2,2,2,2,2,2,2,2,2,2,2,4),(-0.225338432559396,-0.216182593405001,
-0.180918656438744,-0.15695033994371,-0.140921103227021,-0.129823782035391,
-0.118153571207753,-0.114481377627195,-0.112295015626432,-0.110369884265467,
-0.107992250297605,-0.103463255812088,-0.0921160616038249,-0.080518844719617,
-0.0652099958827568,-0.0432219732389323,0.),.UNSPECIFIED.);
#859=B_SPLINE_CURVE_WITH_KNOTS('',3,(#30773,#30774,#30775,#30776,#30777,
#30778,#30779,#30780,#30781,#30782,#30783,#30784,#30785,#30786,#30787,#30788,
#30789,#30790,#30791,#30792,#30793,#30794,#30795,#30796,#30797,#30798,#30799,
#30800,#30801,#30802,#30803,#30804,#30805,#30806),.UNSPECIFIED.,.F.,.F.,
(4,2,2,2,2,2,2,2,2,2,2,2,2,2,2,2,4),(-0.225338432560286,-0.216182593405743,
-0.180918656439008,-0.156950339943687,-0.140921103226838,-0.129823782035135,
-0.11815357120744,-0.114481377626867,-0.112295015626096,-0.110369884265129,
-0.107992250297272,-0.103463255811758,-0.0921160616035475,-0.0805188447194081,
-0.0652099958826912,-0.0432219732389774,0.),.UNSPECIFIED.);
#860=B_SPLINE_CURVE_WITH_KNOTS('',3,(#30815,#30816,#30817,#30818,#30819,
#30820,#30821,#30822,#30823,#30824,#30825,#30826,#30827,#30828,#30829,#30830,
#30831,#30832,#30833,#30834,#30835,#30836,#30837,#30838,#30839,#30840,#30841,
#30842,#30843,#30844,#30845,#30846,#30847,#30848),.UNSPECIFIED.,.F.,.F.,
(4,2,2,2,2,2,2,2,2,2,2,2,2,2,2,2,4),(-0.225338432557624,-0.216182593403256,
-0.180918656437128,-0.156950339942263,-0.14092110322575,-0.129823782034263,
-0.118153571206773,-0.114481377626263,-0.112295015625533,-0.110369884264596,
-0.107992250296765,-0.103463255811312,-0.0921160616032174,-0.0805188447191867,
-0.0652099958825827,-0.0432219732389505,0.),.UNSPECIFIED.);
#861=B_SPLINE_CURVE_WITH_KNOTS('',3,(#30857,#30858,#30859,#30860,#30861,
#30862,#30863,#30864,#30865,#30866,#30867,#30868,#30869,#30870,#30871,#30872,
#30873,#30874,#30875,#30876,#30877,#30878,#30879,#30880,#30881,#30882,#30883,
#30884,#30885,#30886,#30887,#30888,#30889,#30890),.UNSPECIFIED.,.F.,.F.,
(4,2,2,2,2,2,2,2,2,2,2,2,2,2,2,2,4),(-0.225338432559972,-0.216182593405463,
-0.180918656438837,-0.156950339943573,-0.140921103226747,-0.129823782035054,
-0.118153571207361,-0.114481377626792,-0.112295015626031,-0.110369884265071,
-0.107992250297217,-0.103463255811723,-0.0921160616035288,-0.0805188447194011,
-0.0652099958826789,-0.0432219732389621,0.),.UNSPECIFIED.);
#862=B_SPLINE_CURVE_WITH_KNOTS('',3,(#30899,#30900,#30901,#30902,#30903,
#30904,#30905,#30906,#30907,#30908,#30909,#30910,#30911,#30912,#30913,#30914,
#30915,#30916,#30917,#30918,#30919,#30920,#30921,#30922,#30923,#30924,#30925,
#30926,#30927,#30928,#30929,#30930,#30931,#30932),.UNSPECIFIED.,.F.,.F.,
(4,2,2,2,2,2,2,2,2,2,2,2,2,2,2,2,4),(-0.225338432559886,-0.216182593405346,
-0.180918656438623,-0.156950339943384,-0.140921103226634,-0.129823782034983,
-0.118153571207324,-0.11448137762676,-0.112295015626009,-0.110369884265057,
-0.1079922502972,-0.103463255811702,-0.0921160616035172,-0.080518844719388,
-0.0652099958826653,-0.0432219732389498,0.),.UNSPECIFIED.);
#863=B_SPLINE_CURVE_WITH_KNOTS('',3,(#30941,#30942,#30943,#30944,#30945,
#30946,#30947,#30948,#30949,#30950,#30951,#30952,#30953,#30954,#30955,#30956,
#30957,#30958,#30959,#30960,#30961,#30962,#30963,#30964,#30965,#30966,#30967,
#30968,#30969,#30970,#30971,#30972,#30973,#30974),.UNSPECIFIED.,.F.,.F.,
(4,2,2,2,2,2,2,2,2,2,2,2,2,2,2,2,4),(-0.225338432560165,-0.216182593405626,
-0.180918656438868,-0.156950339943628,-0.140921103226887,-0.12982378203525,
-0.118153571207617,-0.114481377627066,-0.112295015626281,-0.110369884265287,
-0.107992250297409,-0.103463255811908,-0.0921160616036701,-0.0805188447195032,
-0.0652099958827271,-0.0432219732389648,0.),.UNSPECIFIED.);
#864=B_SPLINE_CURVE_WITH_KNOTS('',3,(#30983,#30984,#30985,#30986,#30987,
#30988,#30989,#30990,#30991,#30992,#30993,#30994,#30995,#30996,#30997,#30998,
#30999,#31000,#31001,#31002,#31003,#31004,#31005,#31006,#31007,#31008,#31009,
#31010,#31011,#31012,#31013,#31014,#31015,#31016),.UNSPECIFIED.,.F.,.F.,
(4,2,2,2,2,2,2,2,2,2,2,2,2,2,2,2,4),(-0.225338432558513,-0.216182593404118,
-0.180918656437953,-0.156950339943,-0.14092110322638,-0.129823782034829,
-0.118153571207289,-0.114481377626764,-0.112295015626003,-0.110369884265039,
-0.10799225029719,-0.103463255811691,-0.0921160616035001,-0.0805188447193769,
-0.0652099958826662,-0.0432219732389656,0.),.UNSPECIFIED.);
#865=B_SPLINE_CURVE_WITH_KNOTS('',3,(#31025,#31026,#31027,#31028,#31029,
#31030,#31031,#31032,#31033,#31034,#31035,#31036,#31037,#31038,#31039,#31040,
#31041,#31042,#31043,#31044,#31045,#31046,#31047,#31048,#31049,#31050,#31051,
#31052,#31053,#31054,#31055,#31056,#31057,#31058),.UNSPECIFIED.,.F.,.F.,
(4,2,2,2,2,2,2,2,2,2,2,2,2,2,2,2,4),(-0.225338432558754,-0.21618259340434,
-0.18091865643812,-0.156950339943179,-0.140921103226598,-0.129823782035052,
-0.118153571207509,-0.114481377626976,-0.112295015626201,-0.110369884265216,
-0.107992250297339,-0.103463255811827,-0.0921160616036153,-0.0805188447194577,
-0.065209995882691,-0.0432219732389451,0.),.UNSPECIFIED.);
#866=B_SPLINE_CURVE_WITH_KNOTS('',3,(#31067,#31068,#31069,#31070,#31071,
#31072,#31073,#31074,#31075,#31076,#31077,#31078,#31079,#31080,#31081,#31082,
#31083,#31084,#31085,#31086,#31087,#31088,#31089,#31090,#31091,#31092,#31093,
#31094,#31095,#31096,#31097,#31098,#31099,#31100),.UNSPECIFIED.,.F.,.F.,
(4,2,2,2,2,2,2,2,2,2,2,2,2,2,2,2,4),(-0.225338432559566,-0.216182593405091,
-0.18091865643861,-0.156950339943494,-0.140921103226803,-0.129823782035189,
-0.118153571207577,-0.114481377627025,-0.11229501562625,-0.11036988426527,
-0.1079922502974,-0.103463255811888,-0.0921160616036564,-0.0805188447194867,
-0.0652099958827102,-0.0432219732389514,0.),.UNSPECIFIED.);
#867=B_SPLINE_CURVE_WITH_KNOTS('',3,(#31109,#31110,#31111,#31112,#31113,
#31114,#31115,#31116,#31117,#31118,#31119,#31120,#31121,#31122,#31123,#31124,
#31125,#31126,#31127,#31128,#31129,#31130,#31131,#31132,#31133,#31134,#31135,
#31136,#31137,#31138,#31139,#31140,#31141,#31142),.UNSPECIFIED.,.F.,.F.,
(4,2,2,2,2,2,2,2,2,2,2,2,2,2,2,2,4),(-0.225338432560737,-0.216182593406169,
-0.180918656439285,-0.156950339943892,-0.140921103227009,-0.129823782035269,
-0.118153571207521,-0.114481377626936,-0.112295015626147,-0.11036988426516,
-0.107992250297296,-0.103463255811794,-0.0921160616035909,-0.0805188447194464,
-0.0652099958826976,-0.0432219732389541,0.),.UNSPECIFIED.);
#868=B_SPLINE_CURVE_WITH_KNOTS('',3,(#31151,#31152,#31153,#31154,#31155,
#31156,#31157,#31158,#31159,#31160,#31161,#31162,#31163,#31164,#31165,#31166,
#31167,#31168,#31169,#31170,#31171,#31172,#31173,#31174,#31175,#31176,#31177,
#31178,#31179,#31180,#31181,#31182,#31183,#31184),.UNSPECIFIED.,.F.,.F.,
(4,2,2,2,2,2,2,2,2,2,2,2,2,2,2,2,4),(-0.225338432559896,-0.216182593405404,
-0.180918656438774,-0.156950339943504,-0.140921103226688,-0.129823782034989,
-0.118153571207288,-0.114481377626717,-0.112295015625947,-0.110369884264978,
-0.107992250297119,-0.103463255811626,-0.0921160616034505,-0.0805188447193407,
-0.0652099958826552,-0.0432219732389624,0.),.UNSPECIFIED.);
#869=B_SPLINE_CURVE_WITH_KNOTS('',3,(#31193,#31194,#31195,#31196,#31197,
#31198,#31199,#31200,#31201,#31202,#31203,#31204,#31205,#31206,#31207,#31208,
#31209,#31210,#31211,#31212,#31213,#31214,#31215,#31216,#31217,#31218,#31219,
#31220,#31221,#31222,#31223,#31224,#31225,#31226),.UNSPECIFIED.,.F.,.F.,
(4,2,2,2,2,2,2,2,2,2,2,2,2,2,2,2,4),(-0.225338432559856,-0.216182593405332,
-0.180918656438658,-0.156950339943401,-0.140921103226618,-0.129823782034946,
-0.118153571207272,-0.114481377626712,-0.11229501562595,-0.110369884264986,
-0.107992250297126,-0.103463255811634,-0.0921160616034556,-0.0805188447193506,
-0.0652099958826651,-0.0432219732389713,0.),.UNSPECIFIED.);
#870=B_SPLINE_CURVE_WITH_KNOTS('',3,(#31235,#31236,#31237,#31238,#31239,
#31240,#31241,#31242,#31243,#31244,#31245,#31246,#31247,#31248,#31249,#31250,
#31251,#31252,#31253,#31254,#31255,#31256,#31257,#31258,#31259,#31260,#31261,
#31262,#31263,#31264,#31265,#31266,#31267,#31268),.UNSPECIFIED.,.F.,.F.,
(4,2,2,2,2,2,2,2,2,2,2,2,2,2,2,2,4),(-0.225338432559793,-0.216182593405304,
-0.180918656438779,-0.156950339943631,-0.140921103226917,-0.129823782035281,
-0.118153571207644,-0.114481377627095,-0.112295015626322,-0.110369884265348,
-0.107992250297489,-0.10346325581197,-0.0921160616037223,-0.0805188447195313,
-0.0652099958827248,-0.0432219732389509,0.),.UNSPECIFIED.);
#871=B_SPLINE_CURVE_WITH_KNOTS('',3,(#31277,#31278,#31279,#31280,#31281,
#31282,#31283,#31284,#31285,#31286,#31287,#31288,#31289,#31290,#31291,#31292,
#31293,#31294,#31295,#31296,#31297,#31298,#31299,#31300,#31301,#31302,#31303,
#31304,#31305,#31306,#31307,#31308,#31309,#31310),.UNSPECIFIED.,.F.,.F.,
(4,2,2,2,2,2,2,2,2,2,2,2,2,2,2,2,4),(-0.225338432558185,-0.216182593403776,
-0.180918656437544,-0.156950339942601,-0.140921103226024,-0.129823782034494,
-0.118153571206967,-0.114481377626462,-0.112295015625713,-0.110369884264754,
-0.107992250296906,-0.103463255811428,-0.0921160616033045,-0.0805188447192422,
-0.0652099958826089,-0.0432219732389611,0.),.UNSPECIFIED.);
#872=B_SPLINE_CURVE_WITH_KNOTS('',3,(#31319,#31320,#31321,#31322,#31323,
#31324,#31325,#31326,#31327,#31328,#31329,#31330,#31331,#31332,#31333,#31334,
#31335,#31336,#31337,#31338,#31339,#31340,#31341,#31342,#31343,#31344,#31345,
#31346,#31347,#31348,#31349,#31350,#31351,#31352),.UNSPECIFIED.,.F.,.F.,
(4,2,2,2,2,2,2,2,2,2,2,2,2,2,2,2,4),(-0.22533843255964,-0.216182593405169,
-0.180918656438643,-0.156950339943465,-0.14092110322672,-0.12982378203507,
-0.118153571207417,-0.114481377626855,-0.112295015626077,-0.110369884265096,
-0.107992250297229,-0.10346325581173,-0.0921160616035346,-0.0805188447194051,
-0.0652099958826819,-0.0432219732389622,0.),.UNSPECIFIED.);
#873=B_SPLINE_CURVE_WITH_KNOTS('',3,(#31361,#31362,#31363,#31364,#31365,
#31366,#31367,#31368,#31369,#31370,#31371,#31372,#31373,#31374,#31375,#31376,
#31377,#31378,#31379,#31380,#31381,#31382,#31383,#31384,#31385,#31386,#31387,
#31388,#31389,#31390,#31391,#31392,#31393,#31394),.UNSPECIFIED.,.F.,.F.,
(4,2,2,2,2,2,2,2,2,2,2,2,2,2,2,2,4),(-0.225338432560957,-0.216182593406373,
-0.180918656439496,-0.156950339944078,-0.140921103227165,-0.129823782035403,
-0.118153571207639,-0.114481377627053,-0.11229501562626,-0.110369884265268,
-0.107992250297394,-0.103463255811882,-0.0921160616036502,-0.0805188447194852,
-0.0652099958827201,-0.0432219732389695,0.),.UNSPECIFIED.);
#874=B_SPLINE_CURVE_WITH_KNOTS('',3,(#31528,#31529,#31530,#31531,#31532,
#31533,#31534,#31535,#31536,#31537,#31538,#31539,#31540,#31541,#31542,#31543,
#31544,#31545,#31546,#31547,#31548,#31549,#31550,#31551,#31552,#31553,#31554,
#31555,#31556,#31557,#31558,#31559,#31560,#31561),.UNSPECIFIED.,.F.,.F.,
(4,2,2,2,2,2,2,2,2,2,2,2,2,2,2,2,4),(-0.225338432560343,-0.216182593405787,
-0.180918656438999,-0.156950339943695,-0.140921103226895,-0.129823782035217,
-0.118153571207545,-0.114481377627,-0.112295015626234,-0.110369884265269,
-0.10799225029742,-0.10346325581189,-0.0921160616036499,-0.0805188447194839,
-0.0652099958827262,-0.04322197323898,0.),.UNSPECIFIED.);
#875=B_SPLINE_CURVE_WITH_KNOTS('',3,(#31840,#31841,#31842,#31843,#31844,
#31845,#31846,#31847,#31848,#31849,#31850,#31851,#31852,#31853,#31854,#31855,
#31856,#31857,#31858,#31859),.UNSPECIFIED.,.F.,.F.,(4,2,2,2,2,2,2,2,2,4),
(-0.787824152103525,-0.776665386905323,-0.683544248464441,-0.586951582106689,
-0.487645947294414,-0.388535605921421,-0.295627476504987,-0.199263976847017,
-0.0990296104815163,0.),.UNSPECIFIED.);
#876=B_SPLINE_CURVE_WITH_KNOTS('',3,(#31860,#31861,#31862,#31863,#31864,
#31865,#31866,#31867,#31868,#31869,#31870,#31871,#31872,#31873,#31874,#31875,
#31876,#31877,#31878,#31879),.UNSPECIFIED.,.F.,.F.,(4,2,2,2,2,2,2,2,2,4),
(0.,0.0550500400736549,0.113849056000799,0.210816540693219,0.310109597556883,
0.410211670547243,0.50352797305395,0.600331621930534,0.699630608578638,
0.787671103816309),.UNSPECIFIED.);
#877=B_SPLINE_CURVE_WITH_KNOTS('',3,(#31883,#31884,#31885,#31886,#31887,
#31888,#31889,#31890,#31891,#31892,#31893,#31894,#31895,#31896,#31897,#31898,
#31899,#31900,#31901,#31902),.UNSPECIFIED.,.F.,.F.,(4,2,2,2,2,2,2,2,2,4),
(-0.787824152103524,-0.776665386905322,-0.68354424846444,-0.586951582106688,
-0.487645947294413,-0.388535605921421,-0.295627476504987,-0.199263976847016,
-0.099029610481516,0.),.UNSPECIFIED.);
#878=B_SPLINE_CURVE_WITH_KNOTS('',3,(#31903,#31904,#31905,#31906,#31907,
#31908,#31909,#31910,#31911,#31912,#31913,#31914,#31915,#31916,#31917,#31918,
#31919,#31920,#31921,#31922),.UNSPECIFIED.,.F.,.F.,(4,2,2,2,2,2,2,2,2,4),
(0.,0.0550500400736533,0.113849056000795,0.210816540693215,0.310109597556879,
0.410211670547239,0.503527973053946,0.600331621930529,0.699630608578633,
0.787671103816304),.UNSPECIFIED.);
#879=B_SPLINE_CURVE_WITH_KNOTS('',3,(#32042,#32043,#32044,#32045,#32046,
#32047,#32048,#32049,#32050,#32051,#32052,#32053,#32054),.UNSPECIFIED.,
 .F.,.F.,(4,3,3,3,4),(-0.114678109950221,0.00706539599431312,0.499330519660279,
0.973092065693301,0.984123122879426),.UNSPECIFIED.);
#880=B_SPLINE_CURVE_WITH_KNOTS('',3,(#32333,#32334,#32335,#32336,#32337,
#32338,#32339,#32340,#32341,#32342,#32343,#32344,#32345,#32346,#32347,#32348,
#32349,#32350,#32351,#32352),.UNSPECIFIED.,.F.,.F.,(4,2,2,2,2,2,2,2,2,4),
(-0.787824152103525,-0.776665386905323,-0.683544248464441,-0.586951582106689,
-0.487645947294414,-0.388535605921421,-0.295627476504987,-0.199263976847017,
-0.0990296104815162,0.),.UNSPECIFIED.);
#881=B_SPLINE_CURVE_WITH_KNOTS('',3,(#32353,#32354,#32355,#32356,#32357,
#32358,#32359,#32360,#32361,#32362,#32363,#32364,#32365,#32366,#32367,#32368,
#32369,#32370,#32371,#32372),.UNSPECIFIED.,.F.,.F.,(4,2,2,2,2,2,2,2,2,4),
(0.,0.055050040073654,0.113849056000797,0.210816540693217,0.310109597556882,
0.410211670547242,0.503527973053949,0.600331621930533,0.699630608578637,
0.787671103816308),.UNSPECIFIED.);
#882=B_SPLINE_CURVE_WITH_KNOTS('',3,(#32376,#32377,#32378,#32379,#32380,
#32381,#32382,#32383,#32384,#32385,#32386,#32387,#32388,#32389,#32390,#32391,
#32392,#32393,#32394,#32395),.UNSPECIFIED.,.F.,.F.,(4,2,2,2,2,2,2,2,2,4),
(-0.787824152103524,-0.776665386905322,-0.683544248464441,-0.586951582106688,
-0.487645947294414,-0.388535605921421,-0.295627476504987,-0.199263976847017,
-0.0990296104815161,0.),.UNSPECIFIED.);
#883=B_SPLINE_CURVE_WITH_KNOTS('',3,(#32396,#32397,#32398,#32399,#32400,
#32401,#32402,#32403,#32404,#32405,#32406,#32407,#32408,#32409,#32410,#32411,
#32412,#32413,#32414,#32415),.UNSPECIFIED.,.F.,.F.,(4,2,2,2,2,2,2,2,2,4),
(0.,0.0550500400736524,0.113849056000793,0.210816540693213,0.310109597556877,
0.410211670547238,0.503527973053945,0.600331621930529,0.699630608578633,
0.787671103816303),.UNSPECIFIED.);
#884=B_SPLINE_CURVE_WITH_KNOTS('',3,(#32535,#32536,#32537,#32538,#32539,
#32540,#32541,#32542,#32543,#32544,#32545,#32546,#32547),.UNSPECIFIED.,
 .F.,.F.,(4,3,3,3,4),(-0.114678109950223,0.00706539599431312,0.499330519660279,
0.973092065693301,0.984123122879426),.UNSPECIFIED.);
#885=B_SPLINE_CURVE_WITH_KNOTS('',3,(#33225,#33226,#33227,#33228,#33229,
#33230,#33231,#33232,#33233,#33234,#33235,#33236,#33237,#33238,#33239,#33240,
#33241,#33242,#33243,#33244,#33245,#33246,#33247,#33248,#33249,#33250,#33251,
#33252,#33253,#33254,#33255,#33256,#33257,#33258,#33259,#33260,#33261,#33262),
 .UNSPECIFIED.,.T.,.F.,(4,2,2,2,2,2,2,2,2,2,2,2,2,2,2,2,2,2,4),(0.,0.00206072859309695,
0.0220215556481098,0.0407099078585203,0.0625462239528445,0.0881430461322091,
0.1134648757547,0.139536921228863,0.159892801933617,0.179007909130638,0.198254802917601,
0.219009023030338,0.245767304565503,0.269399724022644,0.291540287076427,
0.310569846912954,0.326831397693072,0.344031389185084,0.345530869607548),
 .UNSPECIFIED.);
#886=B_SPLINE_CURVE_WITH_KNOTS('',3,(#33264,#33265,#33266,#33267,#33268,
#33269,#33270,#33271,#33272,#33273,#33274,#33275,#33276,#33277,#33278,#33279,
#33280,#33281,#33282,#33283,#33284,#33285,#33286,#33287,#33288,#33289,#33290,
#33291,#33292,#33293,#33294,#33295,#33296,#33297,#33298,#33299,#33300,#33301,
#33302,#33303,#33304,#33305,#33306,#33307,#33308,#33309,#33310,#33311,#33312,
#33313,#33314,#33315,#33316,#33317,#33318,#33319,#33320,#33321,#33322,#33323,
#33324,#33325,#33326,#33327,#33328,#33329,#33330),.UNSPECIFIED.,.F.,.F.,
(4,1,1,1,1,1,1,1,1,1,1,1,1,1,1,1,1,1,1,1,1,1,1,1,1,1,1,1,1,1,1,1,1,1,1,
1,1,1,1,1,1,1,1,1,1,1,1,1,1,1,1,1,1,1,1,1,1,1,1,1,1,1,1,1,4),(0.,0.490873852123405,
0.98174770424681,1.47262155637022,1.96349540849362,2.45436926061703,2.94524311274043,
3.43611696486384,3.92699081698724,4.41786466911065,4.90873852123405,5.39961237335746,
5.89048622548086,6.38136007760427,6.87223392972767,7.36310778185108,7.85398163397448,
8.34485548609789,8.83572933822129,9.3266031903447,9.8174770424681,10.3083508945915,
10.7992247467149,11.2900985988383,11.7809724509617,12.2718463030851,12.7627201552085,
13.2535940073319,13.7444678594553,14.2353417115787,14.7262155637022,15.2170894158256,
15.707963267949,16.1988371200724,16.6897109721958,17.1805848243192,17.6714586764426,
18.162332528566,18.6532063806894,19.1440802328128,19.6349540849362,20.1258279370596,
20.616701789183,21.1075756413064,21.5984494934298,22.0893233455532,22.5801971976766,
23.0710710498,23.5619449019234,24.0528187540469,24.5436926061703,25.0345664582937,
25.5254403104171,26.0163141625405,26.5071880146639,26.9980618667873,27.4889357189107,
27.9798095710341,28.4706834231575,28.9615572752809,29.4524311274043,29.9433049795277,
30.4341788316511,30.9250526837745,31.4159265358979),.UNSPECIFIED.);
#887=B_SPLINE_CURVE_WITH_KNOTS('',3,(#33331,#33332,#33333,#33334,#33335,
#33336,#33337,#33338,#33339,#33340,#33341,#33342,#33343,#33344,#33345,#33346,
#33347,#33348,#33349,#33350,#33351,#33352,#33353,#33354,#33355,#33356,#33357,
#33358,#33359,#33360,#33361,#33362,#33363,#33364,#33365,#33366,#33367,#33368),
 .UNSPECIFIED.,.T.,.F.,(4,2,2,2,2,2,2,2,2,2,2,2,2,2,2,2,2,2,4),(0.,0.00206072869877635,
0.0220215568887002,0.0407099101465702,0.0625462274814992,0.0881430511099225,
0.113464882180861,0.13953692914445,0.159892811025697,0.179007918914596,
0.19825481309114,0.219009033749323,0.245767316005896,0.269399736268268,
0.291540300209445,0.310569860803271,0.326831412241971,0.344031404416905,
0.345530884782505),.UNSPECIFIED.);
#888=VERTEX_POINT('',#3811);
#889=VERTEX_POINT('',#3812);
#890=VERTEX_POINT('',#3819);
#891=VERTEX_POINT('',#3821);
#892=VERTEX_POINT('',#3856);
#893=VERTEX_POINT('',#4047);
#894=VERTEX_POINT('',#4058);
#895=VERTEX_POINT('',#4249);
#896=VERTEX_POINT('',#4262);
#897=VERTEX_POINT('',#4456);
#898=VERTEX_POINT('',#4467);
#899=VERTEX_POINT('',#4479);
#900=VERTEX_POINT('',#4490);
#901=VERTEX_POINT('',#4501);
#902=VERTEX_POINT('',#4692);
#903=VERTEX_POINT('',#4703);
#904=VERTEX_POINT('',#4894);
#905=VERTEX_POINT('',#4905);
#906=VERTEX_POINT('',#5096);
#907=VERTEX_POINT('',#5290);
#908=VERTEX_POINT('',#5481);
#909=VERTEX_POINT('',#5493);
#910=VERTEX_POINT('',#5687);
#911=VERTEX_POINT('',#5881);
#912=VERTEX_POINT('',#6072);
#913=VERTEX_POINT('',#6085);
#914=VERTEX_POINT('',#6096);
#915=VERTEX_POINT('',#6290);
#916=VERTEX_POINT('',#6302);
#917=VERTEX_POINT('',#6493);
#918=VERTEX_POINT('',#6504);
#919=VERTEX_POINT('',#6695);
#920=VERTEX_POINT('',#6708);
#921=VERTEX_POINT('',#6902);
#922=VERTEX_POINT('',#6913);
#923=VERTEX_POINT('',#6925);
#924=VERTEX_POINT('',#6936);
#925=VERTEX_POINT('',#6947);
#926=VERTEX_POINT('',#7138);
#927=VERTEX_POINT('',#7329);
#928=VERTEX_POINT('',#7340);
#929=VERTEX_POINT('',#7351);
#930=VERTEX_POINT('',#7358);
#931=VERTEX_POINT('',#7360);
#932=VERTEX_POINT('',#7395);
#933=VERTEX_POINT('',#7586);
#934=VERTEX_POINT('',#7597);
#935=VERTEX_POINT('',#7788);
#936=VERTEX_POINT('',#7801);
#937=VERTEX_POINT('',#7995);
#938=VERTEX_POINT('',#8006);
#939=VERTEX_POINT('',#8018);
#940=VERTEX_POINT('',#8029);
#941=VERTEX_POINT('',#8040);
#942=VERTEX_POINT('',#8231);
#943=VERTEX_POINT('',#8242);
#944=VERTEX_POINT('',#8433);
#945=VERTEX_POINT('',#8444);
#946=VERTEX_POINT('',#8635);
#947=VERTEX_POINT('',#8829);
#948=VERTEX_POINT('',#9020);
#949=VERTEX_POINT('',#9032);
#950=VERTEX_POINT('',#9226);
#951=VERTEX_POINT('',#9420);
#952=VERTEX_POINT('',#9611);
#953=VERTEX_POINT('',#9624);
#954=VERTEX_POINT('',#9635);
#955=VERTEX_POINT('',#9829);
#956=VERTEX_POINT('',#9841);
#957=VERTEX_POINT('',#10032);
#958=VERTEX_POINT('',#10043);
#959=VERTEX_POINT('',#10234);
#960=VERTEX_POINT('',#10247);
#961=VERTEX_POINT('',#10441);
#962=VERTEX_POINT('',#10452);
#963=VERTEX_POINT('',#10464);
#964=VERTEX_POINT('',#10475);
#965=VERTEX_POINT('',#10486);
#966=VERTEX_POINT('',#10677);
#967=VERTEX_POINT('',#10868);
#968=VERTEX_POINT('',#10890);
#969=VERTEX_POINT('',#10891);
#970=VERTEX_POINT('',#11490);
#971=VERTEX_POINT('',#11492);
#972=VERTEX_POINT('',#11617);
#973=VERTEX_POINT('',#11808);
#974=VERTEX_POINT('',#12417);
#975=VERTEX_POINT('',#12910);
#976=VERTEX_POINT('',#13471);
#977=VERTEX_POINT('',#13662);
#978=VERTEX_POINT('',#13673);
#979=VERTEX_POINT('',#14174);
#980=VERTEX_POINT('',#14365);
#981=VERTEX_POINT('',#14376);
#982=VERTEX_POINT('',#14567);
#983=VERTEX_POINT('',#15040);
#984=VERTEX_POINT('',#15525);
#985=VERTEX_POINT('',#16018);
#986=VERTEX_POINT('',#16209);
#987=VERTEX_POINT('',#16670);
#988=VERTEX_POINT('',#17181);
#989=VERTEX_POINT('',#17772);
#990=VERTEX_POINT('',#17784);
#991=VERTEX_POINT('',#18303);
#992=VERTEX_POINT('',#18491);
#993=VERTEX_POINT('',#18962);
#994=VERTEX_POINT('',#19445);
#995=VERTEX_POINT('',#19636);
#996=VERTEX_POINT('',#19797);
#997=VERTEX_POINT('',#19799);
#998=VERTEX_POINT('',#19924);
#999=VERTEX_POINT('',#20115);
#1000=VERTEX_POINT('',#20708);
#1001=VERTEX_POINT('',#21193);
#1002=VERTEX_POINT('',#21732);
#1003=VERTEX_POINT('',#21923);
#1004=VERTEX_POINT('',#21934);
#1005=VERTEX_POINT('',#22409);
#1006=VERTEX_POINT('',#22600);
#1007=VERTEX_POINT('',#22611);
#1008=VERTEX_POINT('',#22802);
#1009=VERTEX_POINT('',#23275);
#1010=VERTEX_POINT('',#23750);
#1011=VERTEX_POINT('',#24293);
#1012=VERTEX_POINT('',#24484);
#1013=VERTEX_POINT('',#24945);
#1014=VERTEX_POINT('',#25450);
#1015=VERTEX_POINT('',#25641);
#1016=VERTEX_POINT('',#25832);
#1017=VERTEX_POINT('',#25844);
#1018=VERTEX_POINT('',#26315);
#1019=VERTEX_POINT('',#26503);
#1020=VERTEX_POINT('',#27455);
#1021=VERTEX_POINT('',#27457);
#1022=VERTEX_POINT('',#27461);
#1023=VERTEX_POINT('',#27463);
#1024=VERTEX_POINT('',#27465);
#1025=VERTEX_POINT('',#28518);
#1026=VERTEX_POINT('',#29758);
#1027=VERTEX_POINT('',#29759);
#1028=VERTEX_POINT('',#29794);
#1029=VERTEX_POINT('',#29796);
#1030=VERTEX_POINT('',#29800);
#1031=VERTEX_POINT('',#29801);
#1032=VERTEX_POINT('',#29836);
#1033=VERTEX_POINT('',#29838);
#1034=VERTEX_POINT('',#29842);
#1035=VERTEX_POINT('',#29843);
#1036=VERTEX_POINT('',#29878);
#1037=VERTEX_POINT('',#29880);
#1038=VERTEX_POINT('',#29884);
#1039=VERTEX_POINT('',#29885);
#1040=VERTEX_POINT('',#29920);
#1041=VERTEX_POINT('',#29922);
#1042=VERTEX_POINT('',#29926);
#1043=VERTEX_POINT('',#29927);
#1044=VERTEX_POINT('',#29962);
#1045=VERTEX_POINT('',#29964);
#1046=VERTEX_POINT('',#29968);
#1047=VERTEX_POINT('',#29969);
#1048=VERTEX_POINT('',#30004);
#1049=VERTEX_POINT('',#30006);
#1050=VERTEX_POINT('',#30010);
#1051=VERTEX_POINT('',#30011);
#1052=VERTEX_POINT('',#30046);
#1053=VERTEX_POINT('',#30048);
#1054=VERTEX_POINT('',#30052);
#1055=VERTEX_POINT('',#30053);
#1056=VERTEX_POINT('',#30088);
#1057=VERTEX_POINT('',#30090);
#1058=VERTEX_POINT('',#30094);
#1059=VERTEX_POINT('',#30095);
#1060=VERTEX_POINT('',#30130);
#1061=VERTEX_POINT('',#30132);
#1062=VERTEX_POINT('',#30136);
#1063=VERTEX_POINT('',#30137);
#1064=VERTEX_POINT('',#30158);
#1065=VERTEX_POINT('',#30160);
#1066=VERTEX_POINT('',#30162);
#1067=VERTEX_POINT('',#30183);
#1068=VERTEX_POINT('',#30184);
#1069=VERTEX_POINT('',#30219);
#1070=VERTEX_POINT('',#30221);
#1071=VERTEX_POINT('',#30225);
#1072=VERTEX_POINT('',#30226);
#1073=VERTEX_POINT('',#30261);
#1074=VERTEX_POINT('',#30263);
#1075=VERTEX_POINT('',#30267);
#1076=VERTEX_POINT('',#30268);
#1077=VERTEX_POINT('',#30303);
#1078=VERTEX_POINT('',#30305);
#1079=VERTEX_POINT('',#30309);
#1080=VERTEX_POINT('',#30310);
#1081=VERTEX_POINT('',#30345);
#1082=VERTEX_POINT('',#30347);
#1083=VERTEX_POINT('',#30351);
#1084=VERTEX_POINT('',#30352);
#1085=VERTEX_POINT('',#30387);
#1086=VERTEX_POINT('',#30389);
#1087=VERTEX_POINT('',#30393);
#1088=VERTEX_POINT('',#30394);
#1089=VERTEX_POINT('',#30429);
#1090=VERTEX_POINT('',#30431);
#1091=VERTEX_POINT('',#30435);
#1092=VERTEX_POINT('',#30436);
#1093=VERTEX_POINT('',#30471);
#1094=VERTEX_POINT('',#30473);
#1095=VERTEX_POINT('',#30477);
#1096=VERTEX_POINT('',#30478);
#1097=VERTEX_POINT('',#30513);
#1098=VERTEX_POINT('',#30515);
#1099=VERTEX_POINT('',#30519);
#1100=VERTEX_POINT('',#30520);
#1101=VERTEX_POINT('',#30555);
#1102=VERTEX_POINT('',#30557);
#1103=VERTEX_POINT('',#30561);
#1104=VERTEX_POINT('',#30562);
#1105=VERTEX_POINT('',#30597);
#1106=VERTEX_POINT('',#30599);
#1107=VERTEX_POINT('',#30603);
#1108=VERTEX_POINT('',#30604);
#1109=VERTEX_POINT('',#30639);
#1110=VERTEX_POINT('',#30641);
#1111=VERTEX_POINT('',#30645);
#1112=VERTEX_POINT('',#30646);
#1113=VERTEX_POINT('',#30681);
#1114=VERTEX_POINT('',#30683);
#1115=VERTEX_POINT('',#30687);
#1116=VERTEX_POINT('',#30688);
#1117=VERTEX_POINT('',#30723);
#1118=VERTEX_POINT('',#30725);
#1119=VERTEX_POINT('',#30729);
#1120=VERTEX_POINT('',#30730);
#1121=VERTEX_POINT('',#30765);
#1122=VERTEX_POINT('',#30767);
#1123=VERTEX_POINT('',#30771);
#1124=VERTEX_POINT('',#30772);
#1125=VERTEX_POINT('',#30807);
#1126=VERTEX_POINT('',#30809);
#1127=VERTEX_POINT('',#30813);
#1128=VERTEX_POINT('',#30814);
#1129=VERTEX_POINT('',#30849);
#1130=VERTEX_POINT('',#30851);
#1131=VERTEX_POINT('',#30855);
#1132=VERTEX_POINT('',#30856);
#1133=VERTEX_POINT('',#30891);
#1134=VERTEX_POINT('',#30893);
#1135=VERTEX_POINT('',#30897);
#1136=VERTEX_POINT('',#30898);
#1137=VERTEX_POINT('',#30933);
#1138=VERTEX_POINT('',#30935);
#1139=VERTEX_POINT('',#30939);
#1140=VERTEX_POINT('',#30940);
#1141=VERTEX_POINT('',#30975);
#1142=VERTEX_POINT('',#30977);
#1143=VERTEX_POINT('',#30981);
#1144=VERTEX_POINT('',#30982);
#1145=VERTEX_POINT('',#31017);
#1146=VERTEX_POINT('',#31019);
#1147=VERTEX_POINT('',#31023);
#1148=VERTEX_POINT('',#31024);
#1149=VERTEX_POINT('',#31059);
#1150=VERTEX_POINT('',#31061);
#1151=VERTEX_POINT('',#31065);
#1152=VERTEX_POINT('',#31066);
#1153=VERTEX_POINT('',#31101);
#1154=VERTEX_POINT('',#31103);
#1155=VERTEX_POINT('',#31107);
#1156=VERTEX_POINT('',#31108);
#1157=VERTEX_POINT('',#31143);
#1158=VERTEX_POINT('',#31145);
#1159=VERTEX_POINT('',#31149);
#1160=VERTEX_POINT('',#31150);
#1161=VERTEX_POINT('',#31185);
#1162=VERTEX_POINT('',#31187);
#1163=VERTEX_POINT('',#31191);
#1164=VERTEX_POINT('',#31192);
#1165=VERTEX_POINT('',#31227);
#1166=VERTEX_POINT('',#31229);
#1167=VERTEX_POINT('',#31233);
#1168=VERTEX_POINT('',#31234);
#1169=VERTEX_POINT('',#31269);
#1170=VERTEX_POINT('',#31271);
#1171=VERTEX_POINT('',#31275);
#1172=VERTEX_POINT('',#31276);
#1173=VERTEX_POINT('',#31311);
#1174=VERTEX_POINT('',#31313);
#1175=VERTEX_POINT('',#31317);
#1176=VERTEX_POINT('',#31318);
#1177=VERTEX_POINT('',#31353);
#1178=VERTEX_POINT('',#31355);
#1179=VERTEX_POINT('',#31359);
#1180=VERTEX_POINT('',#31360);
#1181=VERTEX_POINT('',#31395);
#1182=VERTEX_POINT('',#31397);
#1183=VERTEX_POINT('',#31439);
#1184=VERTEX_POINT('',#31441);
#1185=VERTEX_POINT('',#31445);
#1186=VERTEX_POINT('',#31526);
#1187=VERTEX_POINT('',#31569);
#1188=VERTEX_POINT('',#31571);
#1189=VERTEX_POINT('',#31575);
#1190=VERTEX_POINT('',#31579);
#1191=VERTEX_POINT('',#31583);
#1192=VERTEX_POINT('',#31584);
#1193=VERTEX_POINT('',#31813);
#1194=VERTEX_POINT('',#31839);
#1195=VERTEX_POINT('',#31881);
#1196=VERTEX_POINT('',#31882);
#1197=VERTEX_POINT('',#32041);
#1198=VERTEX_POINT('',#32055);
#1199=VERTEX_POINT('',#32062);
#1200=VERTEX_POINT('',#32064);
#1201=VERTEX_POINT('',#32068);
#1202=VERTEX_POINT('',#32072);
#1203=VERTEX_POINT('',#32076);
#1204=VERTEX_POINT('',#32077);
#1205=VERTEX_POINT('',#32306);
#1206=VERTEX_POINT('',#32332);
#1207=VERTEX_POINT('',#32374);
#1208=VERTEX_POINT('',#32375);
#1209=VERTEX_POINT('',#32534);
#1210=VERTEX_POINT('',#32548);
#1211=VERTEX_POINT('',#33224);
#1212=VERTEX_POINT('',#33263);
#1213=VERTEX_POINT('',#33373);
#1214=VERTEX_POINT('',#33374);
#1215=VERTEX_POINT('',#33376);
#1216=VERTEX_POINT('',#33380);
#1217=VERTEX_POINT('',#33386);
#1218=VERTEX_POINT('',#33390);
#1219=VERTEX_POINT('',#33396);
#1220=VERTEX_POINT('',#33398);
#1221=VERTEX_POINT('',#33400);
#1222=VERTEX_POINT('',#33404);
#1223=VERTEX_POINT('',#33411);
#1224=VERTEX_POINT('',#33419);
#1225=VERTEX_POINT('',#33425);
#1226=VERTEX_POINT('',#33429);
#1227=VERTEX_POINT('',#33435);
#1228=VERTEX_POINT('',#33445);
#1229=VERTEX_POINT('',#33447);
#1230=VERTEX_POINT('',#33452);
#1231=EDGE_CURVE('',#888,#889,#701,.T.);
#1232=EDGE_CURVE('',#889,#890,#545,.F.);
#1233=EDGE_CURVE('',#890,#891,#702,.T.);
#1234=EDGE_CURVE('',#891,#892,#703,.T.);
#1235=EDGE_CURVE('',#892,#893,#704,.T.);
#1236=EDGE_CURVE('',#893,#894,#705,.T.);
#1237=EDGE_CURVE('',#894,#895,#706,.T.);
#1238=EDGE_CURVE('',#895,#896,#707,.T.);
#1239=EDGE_CURVE('',#896,#897,#708,.T.);
#1240=EDGE_CURVE('',#897,#898,#709,.T.);
#1241=EDGE_CURVE('',#898,#899,#710,.T.);
#1242=EDGE_CURVE('',#899,#900,#711,.T.);
#1243=EDGE_CURVE('',#900,#901,#712,.T.);
#1244=EDGE_CURVE('',#901,#902,#713,.T.);
#1245=EDGE_CURVE('',#902,#903,#714,.T.);
#1246=EDGE_CURVE('',#903,#904,#715,.T.);
#1247=EDGE_CURVE('',#904,#905,#716,.T.);
#1248=EDGE_CURVE('',#905,#906,#717,.T.);
#1249=EDGE_CURVE('',#906,#907,#718,.T.);
#1250=EDGE_CURVE('',#907,#908,#719,.T.);
#1251=EDGE_CURVE('',#908,#909,#720,.T.);
#1252=EDGE_CURVE('',#909,#910,#721,.T.);
#1253=EDGE_CURVE('',#910,#911,#722,.T.);
#1254=EDGE_CURVE('',#911,#912,#723,.T.);
#1255=EDGE_CURVE('',#912,#913,#724,.T.);
#1256=EDGE_CURVE('',#913,#914,#725,.T.);
#1257=EDGE_CURVE('',#914,#915,#726,.T.);
#1258=EDGE_CURVE('',#915,#916,#727,.T.);
#1259=EDGE_CURVE('',#916,#917,#728,.T.);
#1260=EDGE_CURVE('',#917,#918,#729,.T.);
#1261=EDGE_CURVE('',#918,#919,#730,.T.);
#1262=EDGE_CURVE('',#919,#920,#731,.T.);
#1263=EDGE_CURVE('',#920,#921,#732,.T.);
#1264=EDGE_CURVE('',#921,#922,#733,.T.);
#1265=EDGE_CURVE('',#922,#923,#734,.T.);
#1266=EDGE_CURVE('',#923,#924,#735,.T.);
#1267=EDGE_CURVE('',#924,#925,#736,.T.);
#1268=EDGE_CURVE('',#925,#926,#737,.T.);
#1269=EDGE_CURVE('',#926,#927,#738,.T.);
#1270=EDGE_CURVE('',#927,#928,#739,.T.);
#1271=EDGE_CURVE('',#928,#929,#740,.T.);
#1272=EDGE_CURVE('',#930,#929,#546,.F.);
#1273=EDGE_CURVE('',#930,#931,#741,.T.);
#1274=EDGE_CURVE('',#931,#932,#742,.T.);
#1275=EDGE_CURVE('',#932,#933,#743,.T.);
#1276=EDGE_CURVE('',#933,#934,#744,.T.);
#1277=EDGE_CURVE('',#934,#935,#745,.T.);
#1278=EDGE_CURVE('',#935,#936,#746,.T.);
#1279=EDGE_CURVE('',#936,#937,#747,.T.);
#1280=EDGE_CURVE('',#937,#938,#748,.T.);
#1281=EDGE_CURVE('',#938,#939,#749,.T.);
#1282=EDGE_CURVE('',#939,#940,#750,.T.);
#1283=EDGE_CURVE('',#940,#941,#751,.T.);
#1284=EDGE_CURVE('',#941,#942,#752,.T.);
#1285=EDGE_CURVE('',#942,#943,#753,.T.);
#1286=EDGE_CURVE('',#943,#944,#754,.T.);
#1287=EDGE_CURVE('',#944,#945,#755,.T.);
#1288=EDGE_CURVE('',#945,#946,#756,.T.);
#1289=EDGE_CURVE('',#946,#947,#757,.T.);
#1290=EDGE_CURVE('',#947,#948,#758,.T.);
#1291=EDGE_CURVE('',#948,#949,#759,.T.);
#1292=EDGE_CURVE('',#949,#950,#760,.T.);
#1293=EDGE_CURVE('',#950,#951,#761,.T.);
#1294=EDGE_CURVE('',#951,#952,#762,.T.);
#1295=EDGE_CURVE('',#952,#953,#763,.T.);
#1296=EDGE_CURVE('',#953,#954,#764,.T.);
#1297=EDGE_CURVE('',#954,#955,#765,.T.);
#1298=EDGE_CURVE('',#955,#956,#766,.T.);
#1299=EDGE_CURVE('',#956,#957,#767,.T.);
#1300=EDGE_CURVE('',#957,#958,#768,.T.);
#1301=EDGE_CURVE('',#958,#959,#769,.T.);
#1302=EDGE_CURVE('',#959,#960,#770,.T.);
#1303=EDGE_CURVE('',#960,#961,#771,.T.);
#1304=EDGE_CURVE('',#961,#962,#772,.T.);
#1305=EDGE_CURVE('',#962,#963,#773,.T.);
#1306=EDGE_CURVE('',#963,#964,#774,.T.);
#1307=EDGE_CURVE('',#964,#965,#775,.T.);
#1308=EDGE_CURVE('',#965,#966,#776,.T.);
#1309=EDGE_CURVE('',#966,#967,#777,.T.);
#1310=EDGE_CURVE('',#967,#888,#778,.T.);
#1311=EDGE_CURVE('',#968,#969,#779,.F.);
#1312=EDGE_CURVE('',#970,#968,#547,.T.);
#1313=EDGE_CURVE('',#970,#971,#780,.T.);
#1314=EDGE_CURVE('',#971,#972,#781,.T.);
#1315=EDGE_CURVE('',#972,#973,#782,.T.);
#1316=EDGE_CURVE('',#973,#974,#783,.T.);
#1317=EDGE_CURVE('',#974,#975,#784,.T.);
#1318=EDGE_CURVE('',#975,#976,#785,.T.);
#1319=EDGE_CURVE('',#976,#977,#786,.T.);
#1320=EDGE_CURVE('',#977,#978,#787,.T.);
#1321=EDGE_CURVE('',#978,#979,#788,.T.);
#1322=EDGE_CURVE('',#979,#980,#789,.T.);
#1323=EDGE_CURVE('',#980,#981,#790,.T.);
#1324=EDGE_CURVE('',#981,#982,#791,.T.);
#1325=EDGE_CURVE('',#982,#983,#792,.T.);
#1326=EDGE_CURVE('',#983,#984,#793,.T.);
#1327=EDGE_CURVE('',#984,#985,#794,.T.);
#1328=EDGE_CURVE('',#985,#986,#795,.T.);
#1329=EDGE_CURVE('',#986,#987,#796,.T.);
#1330=EDGE_CURVE('',#987,#988,#797,.T.);
#1331=EDGE_CURVE('',#988,#989,#798,.T.);
#1332=EDGE_CURVE('',#989,#990,#799,.T.);
#1333=EDGE_CURVE('',#990,#991,#800,.T.);
#1334=EDGE_CURVE('',#991,#992,#801,.T.);
#1335=EDGE_CURVE('',#992,#993,#802,.T.);
#1336=EDGE_CURVE('',#993,#994,#803,.T.);
#1337=EDGE_CURVE('',#994,#995,#804,.T.);
#1338=EDGE_CURVE('',#996,#995,#548,.T.);
#1339=EDGE_CURVE('',#997,#996,#805,.T.);
#1340=EDGE_CURVE('',#998,#997,#806,.T.);
#1341=EDGE_CURVE('',#999,#998,#807,.F.);
#1342=EDGE_CURVE('',#1000,#999,#808,.F.);
#1343=EDGE_CURVE('',#1001,#1000,#809,.F.);
#1344=EDGE_CURVE('',#1002,#1001,#810,.T.);
#1345=EDGE_CURVE('',#1003,#1002,#811,.T.);
#1346=EDGE_CURVE('',#1004,#1003,#812,.F.);
#1347=EDGE_CURVE('',#1005,#1004,#813,.T.);
#1348=EDGE_CURVE('',#1006,#1005,#814,.T.);
#1349=EDGE_CURVE('',#1007,#1006,#815,.T.);
#1350=EDGE_CURVE('',#1008,#1007,#816,.F.);
#1351=EDGE_CURVE('',#1009,#1008,#817,.F.);
#1352=EDGE_CURVE('',#1010,#1009,#818,.F.);
#1353=EDGE_CURVE('',#1011,#1010,#819,.T.);
#1354=EDGE_CURVE('',#1012,#1011,#820,.F.);
#1355=EDGE_CURVE('',#1013,#1012,#821,.F.);
#1356=EDGE_CURVE('',#1014,#1013,#822,.T.);
#1357=EDGE_CURVE('',#1015,#1014,#823,.T.);
#1358=EDGE_CURVE('',#1016,#1015,#824,.T.);
#1359=EDGE_CURVE('',#1017,#1016,#825,.F.);
#1360=EDGE_CURVE('',#1018,#1017,#826,.T.);
#1361=EDGE_CURVE('',#1019,#1018,#827,.F.);
#1362=EDGE_CURVE('',#969,#1019,#828,.F.);
#1363=EDGE_CURVE('',#1020,#1020,#549,.T.);
#1364=EDGE_CURVE('',#1020,#1021,#105,.T.);
#1365=EDGE_CURVE('',#1021,#1021,#550,.T.);
#1366=EDGE_CURVE('',#1022,#1022,#551,.T.);
#1367=EDGE_CURVE('',#1022,#1023,#106,.T.);
#1368=EDGE_CURVE('',#1024,#1023,#552,.T.);
#1369=EDGE_CURVE('',#1023,#1024,#553,.T.);
#1370=EDGE_CURVE('',#929,#996,#829,.T.);
#1371=EDGE_CURVE('',#1025,#890,#830,.T.);
#1372=EDGE_CURVE('',#1025,#968,#831,.T.);
#1373=EDGE_CURVE('',#995,#930,#832,.T.);
#1374=EDGE_CURVE('',#889,#970,#833,.T.);
#1375=EDGE_CURVE('',#1026,#1027,#834,.T.);
#1376=EDGE_CURVE('',#1028,#1026,#107,.T.);
#1377=EDGE_CURVE('',#1029,#1028,#554,.T.);
#1378=EDGE_CURVE('',#1027,#1029,#108,.T.);
#1379=EDGE_CURVE('',#1030,#1031,#835,.T.);
#1380=EDGE_CURVE('',#1032,#1030,#109,.T.);
#1381=EDGE_CURVE('',#1033,#1032,#555,.T.);
#1382=EDGE_CURVE('',#1031,#1033,#110,.T.);
#1383=EDGE_CURVE('',#1034,#1035,#836,.T.);
#1384=EDGE_CURVE('',#1036,#1034,#111,.T.);
#1385=EDGE_CURVE('',#1037,#1036,#556,.T.);
#1386=EDGE_CURVE('',#1035,#1037,#112,.T.);
#1387=EDGE_CURVE('',#1038,#1039,#837,.T.);
#1388=EDGE_CURVE('',#1040,#1038,#113,.T.);
#1389=EDGE_CURVE('',#1041,#1040,#557,.T.);
#1390=EDGE_CURVE('',#1039,#1041,#114,.T.);
#1391=EDGE_CURVE('',#1042,#1043,#838,.T.);
#1392=EDGE_CURVE('',#1044,#1042,#115,.T.);
#1393=EDGE_CURVE('',#1045,#1044,#558,.T.);
#1394=EDGE_CURVE('',#1043,#1045,#116,.T.);
#1395=EDGE_CURVE('',#1046,#1047,#839,.T.);
#1396=EDGE_CURVE('',#1048,#1046,#117,.T.);
#1397=EDGE_CURVE('',#1049,#1048,#559,.T.);
#1398=EDGE_CURVE('',#1047,#1049,#118,.T.);
#1399=EDGE_CURVE('',#1050,#1051,#840,.T.);
#1400=EDGE_CURVE('',#1052,#1050,#119,.T.);
#1401=EDGE_CURVE('',#1053,#1052,#560,.T.);
#1402=EDGE_CURVE('',#1051,#1053,#120,.T.);
#1403=EDGE_CURVE('',#1054,#1055,#841,.T.);
#1404=EDGE_CURVE('',#1056,#1054,#121,.T.);
#1405=EDGE_CURVE('',#1057,#1056,#561,.T.);
#1406=EDGE_CURVE('',#1055,#1057,#122,.T.);
#1407=EDGE_CURVE('',#1058,#1059,#842,.T.);
#1408=EDGE_CURVE('',#1060,#1058,#123,.T.);
#1409=EDGE_CURVE('',#1061,#1060,#562,.T.);
#1410=EDGE_CURVE('',#1059,#1061,#124,.T.);
#1411=EDGE_CURVE('',#1062,#1063,#843,.T.);
#1412=EDGE_CURVE('',#1064,#1062,#125,.T.);
#1413=EDGE_CURVE('',#1065,#1064,#563,.T.);
#1414=EDGE_CURVE('',#1066,#1065,#126,.T.);
#1415=EDGE_CURVE('',#1063,#1066,#844,.T.);
#1416=EDGE_CURVE('',#1067,#1068,#845,.T.);
#1417=EDGE_CURVE('',#1069,#1067,#127,.T.);
#1418=EDGE_CURVE('',#1070,#1069,#564,.T.);
#1419=EDGE_CURVE('',#1068,#1070,#128,.T.);
#1420=EDGE_CURVE('',#1071,#1072,#846,.T.);
#1421=EDGE_CURVE('',#1073,#1071,#129,.T.);
#1422=EDGE_CURVE('',#1074,#1073,#565,.T.);
#1423=EDGE_CURVE('',#1072,#1074,#130,.T.);
#1424=EDGE_CURVE('',#1075,#1076,#847,.T.);
#1425=EDGE_CURVE('',#1077,#1075,#131,.T.);
#1426=EDGE_CURVE('',#1078,#1077,#566,.T.);
#1427=EDGE_CURVE('',#1076,#1078,#132,.T.);
#1428=EDGE_CURVE('',#1079,#1080,#848,.T.);
#1429=EDGE_CURVE('',#1081,#1079,#133,.T.);
#1430=EDGE_CURVE('',#1082,#1081,#567,.T.);
#1431=EDGE_CURVE('',#1080,#1082,#134,.T.);
#1432=EDGE_CURVE('',#1083,#1084,#849,.T.);
#1433=EDGE_CURVE('',#1085,#1083,#135,.T.);
#1434=EDGE_CURVE('',#1086,#1085,#568,.T.);
#1435=EDGE_CURVE('',#1084,#1086,#136,.T.);
#1436=EDGE_CURVE('',#1087,#1088,#850,.T.);
#1437=EDGE_CURVE('',#1089,#1087,#137,.T.);
#1438=EDGE_CURVE('',#1090,#1089,#569,.T.);
#1439=EDGE_CURVE('',#1088,#1090,#138,.T.);
#1440=EDGE_CURVE('',#1091,#1092,#851,.T.);
#1441=EDGE_CURVE('',#1093,#1091,#139,.T.);
#1442=EDGE_CURVE('',#1094,#1093,#570,.T.);
#1443=EDGE_CURVE('',#1092,#1094,#140,.T.);
#1444=EDGE_CURVE('',#1095,#1096,#852,.T.);
#1445=EDGE_CURVE('',#1097,#1095,#141,.T.);
#1446=EDGE_CURVE('',#1098,#1097,#571,.T.);
#1447=EDGE_CURVE('',#1096,#1098,#142,.T.);
#1448=EDGE_CURVE('',#1099,#1100,#853,.T.);
#1449=EDGE_CURVE('',#1101,#1099,#143,.T.);
#1450=EDGE_CURVE('',#1102,#1101,#572,.T.);
#1451=EDGE_CURVE('',#1100,#1102,#144,.T.);
#1452=EDGE_CURVE('',#1103,#1104,#854,.T.);
#1453=EDGE_CURVE('',#1105,#1103,#145,.T.);
#1454=EDGE_CURVE('',#1106,#1105,#573,.T.);
#1455=EDGE_CURVE('',#1104,#1106,#146,.T.);
#1456=EDGE_CURVE('',#1107,#1108,#855,.T.);
#1457=EDGE_CURVE('',#1109,#1107,#147,.T.);
#1458=EDGE_CURVE('',#1110,#1109,#574,.T.);
#1459=EDGE_CURVE('',#1108,#1110,#148,.T.);
#1460=EDGE_CURVE('',#1111,#1112,#856,.T.);
#1461=EDGE_CURVE('',#1113,#1111,#149,.T.);
#1462=EDGE_CURVE('',#1114,#1113,#575,.T.);
#1463=EDGE_CURVE('',#1112,#1114,#150,.T.);
#1464=EDGE_CURVE('',#1115,#1116,#857,.T.);
#1465=EDGE_CURVE('',#1117,#1115,#151,.T.);
#1466=EDGE_CURVE('',#1118,#1117,#576,.T.);
#1467=EDGE_CURVE('',#1116,#1118,#152,.T.);
#1468=EDGE_CURVE('',#1119,#1120,#858,.T.);
#1469=EDGE_CURVE('',#1121,#1119,#153,.T.);
#1470=EDGE_CURVE('',#1122,#1121,#577,.T.);
#1471=EDGE_CURVE('',#1120,#1122,#154,.T.);
#1472=EDGE_CURVE('',#1123,#1124,#859,.T.);
#1473=EDGE_CURVE('',#1125,#1123,#155,.T.);
#1474=EDGE_CURVE('',#1126,#1125,#578,.T.);
#1475=EDGE_CURVE('',#1124,#1126,#156,.T.);
#1476=EDGE_CURVE('',#1127,#1128,#860,.T.);
#1477=EDGE_CURVE('',#1129,#1127,#157,.T.);
#1478=EDGE_CURVE('',#1130,#1129,#579,.T.);
#1479=EDGE_CURVE('',#1128,#1130,#158,.T.);
#1480=EDGE_CURVE('',#1131,#1132,#861,.T.);
#1481=EDGE_CURVE('',#1133,#1131,#159,.T.);
#1482=EDGE_CURVE('',#1134,#1133,#580,.T.);
#1483=EDGE_CURVE('',#1132,#1134,#160,.T.);
#1484=EDGE_CURVE('',#1135,#1136,#862,.T.);
#1485=EDGE_CURVE('',#1137,#1135,#161,.T.);
#1486=EDGE_CURVE('',#1138,#1137,#581,.T.);
#1487=EDGE_CURVE('',#1136,#1138,#162,.T.);
#1488=EDGE_CURVE('',#1139,#1140,#863,.T.);
#1489=EDGE_CURVE('',#1141,#1139,#163,.T.);
#1490=EDGE_CURVE('',#1142,#1141,#582,.T.);
#1491=EDGE_CURVE('',#1140,#1142,#164,.T.);
#1492=EDGE_CURVE('',#1143,#1144,#864,.T.);
#1493=EDGE_CURVE('',#1145,#1143,#165,.T.);
#1494=EDGE_CURVE('',#1146,#1145,#583,.T.);
#1495=EDGE_CURVE('',#1144,#1146,#166,.T.);
#1496=EDGE_CURVE('',#1147,#1148,#865,.T.);
#1497=EDGE_CURVE('',#1149,#1147,#167,.T.);
#1498=EDGE_CURVE('',#1150,#1149,#584,.T.);
#1499=EDGE_CURVE('',#1148,#1150,#168,.T.);
#1500=EDGE_CURVE('',#1151,#1152,#866,.T.);
#1501=EDGE_CURVE('',#1153,#1151,#169,.T.);
#1502=EDGE_CURVE('',#1154,#1153,#585,.T.);
#1503=EDGE_CURVE('',#1152,#1154,#170,.T.);
#1504=EDGE_CURVE('',#1155,#1156,#867,.T.);
#1505=EDGE_CURVE('',#1157,#1155,#171,.T.);
#1506=EDGE_CURVE('',#1158,#1157,#586,.T.);
#1507=EDGE_CURVE('',#1156,#1158,#172,.T.);
#1508=EDGE_CURVE('',#1159,#1160,#868,.T.);
#1509=EDGE_CURVE('',#1161,#1159,#173,.T.);
#1510=EDGE_CURVE('',#1162,#1161,#587,.T.);
#1511=EDGE_CURVE('',#1160,#1162,#174,.T.);
#1512=EDGE_CURVE('',#1163,#1164,#869,.T.);
#1513=EDGE_CURVE('',#1165,#1163,#175,.T.);
#1514=EDGE_CURVE('',#1166,#1165,#588,.T.);
#1515=EDGE_CURVE('',#1164,#1166,#176,.T.);
#1516=EDGE_CURVE('',#1167,#1168,#870,.T.);
#1517=EDGE_CURVE('',#1169,#1167,#177,.T.);
#1518=EDGE_CURVE('',#1170,#1169,#589,.T.);
#1519=EDGE_CURVE('',#1168,#1170,#178,.T.);
#1520=EDGE_CURVE('',#1171,#1172,#871,.T.);
#1521=EDGE_CURVE('',#1173,#1171,#179,.T.);
#1522=EDGE_CURVE('',#1174,#1173,#590,.T.);
#1523=EDGE_CURVE('',#1172,#1174,#180,.T.);
#1524=EDGE_CURVE('',#1175,#1176,#872,.T.);
#1525=EDGE_CURVE('',#1177,#1175,#181,.T.);
#1526=EDGE_CURVE('',#1178,#1177,#591,.T.);
#1527=EDGE_CURVE('',#1176,#1178,#182,.T.);
#1528=EDGE_CURVE('',#1179,#1180,#873,.T.);
#1529=EDGE_CURVE('',#1181,#1179,#183,.T.);
#1530=EDGE_CURVE('',#1182,#1181,#592,.T.);
#1531=EDGE_CURVE('',#1180,#1182,#184,.T.);
#1532=EDGE_CURVE('',#1033,#1028,#593,.T.);
#1533=EDGE_CURVE('',#1037,#1032,#594,.T.);
#1534=EDGE_CURVE('',#1041,#1036,#595,.T.);
#1535=EDGE_CURVE('',#1045,#1040,#596,.T.);
#1536=EDGE_CURVE('',#1049,#1044,#597,.T.);
#1537=EDGE_CURVE('',#1053,#1048,#598,.T.);
#1538=EDGE_CURVE('',#1057,#1052,#599,.T.);
#1539=EDGE_CURVE('',#1061,#1056,#600,.T.);
#1540=EDGE_CURVE('',#1065,#1060,#601,.T.);
#1541=EDGE_CURVE('',#1070,#1064,#602,.T.);
#1542=EDGE_CURVE('',#1074,#1069,#603,.T.);
#1543=EDGE_CURVE('',#1078,#1073,#604,.T.);
#1544=EDGE_CURVE('',#1082,#1077,#605,.T.);
#1545=EDGE_CURVE('',#1086,#1081,#606,.T.);
#1546=EDGE_CURVE('',#1090,#1085,#607,.T.);
#1547=EDGE_CURVE('',#1094,#1089,#608,.T.);
#1548=EDGE_CURVE('',#1098,#1093,#609,.T.);
#1549=EDGE_CURVE('',#1102,#1097,#610,.T.);
#1550=EDGE_CURVE('',#1106,#1101,#611,.T.);
#1551=EDGE_CURVE('',#1110,#1105,#612,.T.);
#1552=EDGE_CURVE('',#1114,#1109,#613,.T.);
#1553=EDGE_CURVE('',#1118,#1113,#614,.T.);
#1554=EDGE_CURVE('',#1122,#1117,#615,.T.);
#1555=EDGE_CURVE('',#1126,#1121,#616,.T.);
#1556=EDGE_CURVE('',#1130,#1125,#617,.T.);
#1557=EDGE_CURVE('',#1134,#1129,#618,.T.);
#1558=EDGE_CURVE('',#1138,#1133,#619,.T.);
#1559=EDGE_CURVE('',#1142,#1137,#620,.T.);
#1560=EDGE_CURVE('',#1146,#1141,#621,.T.);
#1561=EDGE_CURVE('',#1150,#1145,#622,.T.);
#1562=EDGE_CURVE('',#1154,#1149,#623,.T.);
#1563=EDGE_CURVE('',#1158,#1153,#624,.T.);
#1564=EDGE_CURVE('',#1162,#1157,#625,.T.);
#1565=EDGE_CURVE('',#1166,#1161,#626,.T.);
#1566=EDGE_CURVE('',#1170,#1165,#627,.T.);
#1567=EDGE_CURVE('',#1174,#1169,#628,.T.);
#1568=EDGE_CURVE('',#1178,#1173,#629,.T.);
#1569=EDGE_CURVE('',#1182,#1177,#630,.T.);
#1570=EDGE_CURVE('',#1183,#1181,#631,.T.);
#1571=EDGE_CURVE('',#1183,#1184,#632,.T.);
#1572=EDGE_CURVE('',#1029,#1184,#633,.T.);
#1573=EDGE_CURVE('',#1185,#1179,#634,.T.);
#1574=EDGE_CURVE('',#1185,#1183,#185,.T.);
#1575=EDGE_CURVE('',#1180,#1175,#635,.T.);
#1576=EDGE_CURVE('',#1176,#1171,#636,.T.);
#1577=EDGE_CURVE('',#1172,#1167,#637,.T.);
#1578=EDGE_CURVE('',#1168,#1163,#638,.T.);
#1579=EDGE_CURVE('',#1164,#1159,#639,.T.);
#1580=EDGE_CURVE('',#1160,#1155,#640,.T.);
#1581=EDGE_CURVE('',#1156,#1151,#641,.T.);
#1582=EDGE_CURVE('',#1152,#1147,#642,.T.);
#1583=EDGE_CURVE('',#1148,#1143,#643,.T.);
#1584=EDGE_CURVE('',#1144,#1139,#644,.T.);
#1585=EDGE_CURVE('',#1140,#1135,#645,.T.);
#1586=EDGE_CURVE('',#1136,#1131,#646,.T.);
#1587=EDGE_CURVE('',#1132,#1127,#647,.T.);
#1588=EDGE_CURVE('',#1128,#1123,#648,.T.);
#1589=EDGE_CURVE('',#1124,#1119,#649,.T.);
#1590=EDGE_CURVE('',#1120,#1115,#650,.T.);
#1591=EDGE_CURVE('',#1116,#1111,#651,.T.);
#1592=EDGE_CURVE('',#1112,#1107,#652,.T.);
#1593=EDGE_CURVE('',#1108,#1103,#653,.T.);
#1594=EDGE_CURVE('',#1104,#1099,#654,.T.);
#1595=EDGE_CURVE('',#1100,#1095,#655,.T.);
#1596=EDGE_CURVE('',#1096,#1091,#656,.T.);
#1597=EDGE_CURVE('',#1092,#1087,#657,.T.);
#1598=EDGE_CURVE('',#1088,#1083,#658,.T.);
#1599=EDGE_CURVE('',#1084,#1079,#659,.T.);
#1600=EDGE_CURVE('',#1080,#1075,#660,.T.);
#1601=EDGE_CURVE('',#1076,#1071,#661,.T.);
#1602=EDGE_CURVE('',#1072,#1067,#662,.T.);
#1603=EDGE_CURVE('',#1068,#1062,#663,.T.);
#1604=EDGE_CURVE('',#1066,#1058,#664,.T.);
#1605=EDGE_CURVE('',#1059,#1054,#665,.T.);
#1606=EDGE_CURVE('',#1055,#1050,#666,.T.);
#1607=EDGE_CURVE('',#1051,#1046,#667,.T.);
#1608=EDGE_CURVE('',#1047,#1042,#668,.T.);
#1609=EDGE_CURVE('',#1043,#1038,#669,.T.);
#1610=EDGE_CURVE('',#1039,#1034,#670,.T.);
#1611=EDGE_CURVE('',#1035,#1030,#671,.T.);
#1612=EDGE_CURVE('',#1031,#1026,#672,.T.);
#1613=EDGE_CURVE('',#1024,#1063,#673,.T.);
#1614=EDGE_CURVE('',#1027,#1186,#674,.T.);
#1615=EDGE_CURVE('',#1186,#1185,#874,.T.);
#1616=EDGE_CURVE('',#1184,#1186,#186,.T.);
#1617=EDGE_CURVE('',#1187,#1187,#675,.T.);
#1618=EDGE_CURVE('',#1187,#1188,#187,.T.);
#1619=EDGE_CURVE('',#1188,#1188,#676,.T.);
#1620=EDGE_CURVE('',#1189,#1189,#677,.T.);
#1621=EDGE_CURVE('',#1189,#1187,#678,.T.);
#1622=EDGE_CURVE('',#1190,#1190,#679,.T.);
#1623=EDGE_CURVE('',#1190,#1189,#188,.T.);
#1624=EDGE_CURVE('',#1191,#1192,#680,.T.);
#1625=EDGE_CURVE('',#1192,#1191,#681,.T.);
#1626=EDGE_CURVE('',#1192,#1190,#682,.T.);
#1627=EDGE_CURVE('',#1193,#1191,#31,.T.);
#1628=EDGE_CURVE('',#1194,#1193,#875,.F.);
#1629=EDGE_CURVE('',#1193,#1194,#876,.F.);
#1630=EDGE_CURVE('',#1195,#1196,#877,.T.);
#1631=EDGE_CURVE('',#1196,#1195,#878,.T.);
#1632=EDGE_CURVE('',#1196,#1194,#189,.T.);
#1633=EDGE_CURVE('',#1195,#1197,#879,.T.);
#1634=EDGE_CURVE('',#1198,#1197,#683,.T.);
#1635=EDGE_CURVE('',#1197,#1198,#684,.T.);
#1636=EDGE_CURVE('',#1188,#1198,#685,.T.);
#1637=EDGE_CURVE('',#1199,#1199,#686,.T.);
#1638=EDGE_CURVE('',#1199,#1200,#190,.T.);
#1639=EDGE_CURVE('',#1200,#1200,#687,.T.);
#1640=EDGE_CURVE('',#1201,#1201,#688,.T.);
#1641=EDGE_CURVE('',#1201,#1199,#689,.T.);
#1642=EDGE_CURVE('',#1202,#1202,#690,.T.);
#1643=EDGE_CURVE('',#1202,#1201,#191,.T.);
#1644=EDGE_CURVE('',#1203,#1204,#691,.T.);
#1645=EDGE_CURVE('',#1204,#1203,#692,.T.);
#1646=EDGE_CURVE('',#1204,#1202,#693,.T.);
#1647=EDGE_CURVE('',#1205,#1203,#32,.T.);
#1648=EDGE_CURVE('',#1206,#1205,#880,.F.);
#1649=EDGE_CURVE('',#1205,#1206,#881,.F.);
#1650=EDGE_CURVE('',#1207,#1208,#882,.T.);
#1651=EDGE_CURVE('',#1208,#1207,#883,.T.);
#1652=EDGE_CURVE('',#1208,#1206,#192,.T.);
#1653=EDGE_CURVE('',#1207,#1209,#884,.T.);
#1654=EDGE_CURVE('',#1210,#1209,#694,.T.);
#1655=EDGE_CURVE('',#1209,#1210,#695,.T.);
#1656=EDGE_CURVE('',#1200,#1210,#696,.T.);
#1657=EDGE_CURVE('',#1211,#1211,#885,.T.);
#1658=EDGE_CURVE('',#1211,#1212,#886,.T.);
#1659=EDGE_CURVE('',#1212,#1212,#887,.T.);
#1660=EDGE_CURVE('',#1213,#1214,#193,.T.);
#1661=EDGE_CURVE('',#1215,#1213,#33,.T.);
#1662=EDGE_CURVE('',#1216,#1215,#194,.T.);
#1663=EDGE_CURVE('',#1214,#1216,#34,.T.);
#1664=EDGE_CURVE('',#1217,#1215,#35,.T.);
#1665=EDGE_CURVE('',#1217,#1218,#195,.T.);
#1666=EDGE_CURVE('',#1216,#1218,#36,.T.);
#1667=EDGE_CURVE('',#1219,#1219,#697,.T.);
#1668=EDGE_CURVE('',#1219,#1220,#196,.T.);
#1669=EDGE_CURVE('',#1220,#1221,#37,.T.);
#1670=EDGE_CURVE('',#1221,#1222,#38,.T.);
#1671=EDGE_CURVE('',#1222,#1217,#39,.T.);
#1672=EDGE_CURVE('',#1213,#1223,#40,.T.);
#1673=EDGE_CURVE('',#1223,#1220,#41,.T.);
#1674=EDGE_CURVE('',#1224,#1214,#42,.T.);
#1675=EDGE_CURVE('',#1223,#1224,#197,.T.);
#1676=EDGE_CURVE('',#1225,#1224,#43,.T.);
#1677=EDGE_CURVE('',#1226,#1225,#44,.T.);
#1678=EDGE_CURVE('',#1221,#1226,#198,.T.);
#1679=EDGE_CURVE('',#1227,#1226,#45,.T.);
#1680=EDGE_CURVE('',#1222,#1227,#199,.T.);
#1681=EDGE_CURVE('',#1218,#1227,#46,.T.);
#1682=EDGE_CURVE('',#1228,#1228,#698,.T.);
#1683=EDGE_CURVE('',#1229,#1229,#699,.F.);
#1684=EDGE_CURVE('',#1225,#1228,#200,.T.);
#1685=EDGE_CURVE('',#1230,#1230,#700,.T.);
#1686=EDGE_CURVE('',#1230,#1229,#201,.T.);
#1687=ORIENTED_EDGE('',*,*,#1231,.T.);
#1688=ORIENTED_EDGE('',*,*,#1232,.T.);
#1689=ORIENTED_EDGE('',*,*,#1233,.T.);
#1690=ORIENTED_EDGE('',*,*,#1234,.T.);
#1691=ORIENTED_EDGE('',*,*,#1235,.T.);
#1692=ORIENTED_EDGE('',*,*,#1236,.T.);
#1693=ORIENTED_EDGE('',*,*,#1237,.T.);
#1694=ORIENTED_EDGE('',*,*,#1238,.T.);
#1695=ORIENTED_EDGE('',*,*,#1239,.T.);
#1696=ORIENTED_EDGE('',*,*,#1240,.T.);
#1697=ORIENTED_EDGE('',*,*,#1241,.T.);
#1698=ORIENTED_EDGE('',*,*,#1242,.T.);
#1699=ORIENTED_EDGE('',*,*,#1243,.T.);
#1700=ORIENTED_EDGE('',*,*,#1244,.T.);
#1701=ORIENTED_EDGE('',*,*,#1245,.T.);
#1702=ORIENTED_EDGE('',*,*,#1246,.T.);
#1703=ORIENTED_EDGE('',*,*,#1247,.T.);
#1704=ORIENTED_EDGE('',*,*,#1248,.T.);
#1705=ORIENTED_EDGE('',*,*,#1249,.T.);
#1706=ORIENTED_EDGE('',*,*,#1250,.T.);
#1707=ORIENTED_EDGE('',*,*,#1251,.T.);
#1708=ORIENTED_EDGE('',*,*,#1252,.T.);
#1709=ORIENTED_EDGE('',*,*,#1253,.T.);
#1710=ORIENTED_EDGE('',*,*,#1254,.T.);
#1711=ORIENTED_EDGE('',*,*,#1255,.T.);
#1712=ORIENTED_EDGE('',*,*,#1256,.T.);
#1713=ORIENTED_EDGE('',*,*,#1257,.T.);
#1714=ORIENTED_EDGE('',*,*,#1258,.T.);
#1715=ORIENTED_EDGE('',*,*,#1259,.T.);
#1716=ORIENTED_EDGE('',*,*,#1260,.T.);
#1717=ORIENTED_EDGE('',*,*,#1261,.T.);
#1718=ORIENTED_EDGE('',*,*,#1262,.T.);
#1719=ORIENTED_EDGE('',*,*,#1263,.T.);
#1720=ORIENTED_EDGE('',*,*,#1264,.T.);
#1721=ORIENTED_EDGE('',*,*,#1265,.T.);
#1722=ORIENTED_EDGE('',*,*,#1266,.T.);
#1723=ORIENTED_EDGE('',*,*,#1267,.T.);
#1724=ORIENTED_EDGE('',*,*,#1268,.T.);
#1725=ORIENTED_EDGE('',*,*,#1269,.T.);
#1726=ORIENTED_EDGE('',*,*,#1270,.T.);
#1727=ORIENTED_EDGE('',*,*,#1271,.T.);
#1728=ORIENTED_EDGE('',*,*,#1272,.F.);
#1729=ORIENTED_EDGE('',*,*,#1273,.T.);
#1730=ORIENTED_EDGE('',*,*,#1274,.T.);
#1731=ORIENTED_EDGE('',*,*,#1275,.T.);
#1732=ORIENTED_EDGE('',*,*,#1276,.T.);
#1733=ORIENTED_EDGE('',*,*,#1277,.T.);
#1734=ORIENTED_EDGE('',*,*,#1278,.T.);
#1735=ORIENTED_EDGE('',*,*,#1279,.T.);
#1736=ORIENTED_EDGE('',*,*,#1280,.T.);
#1737=ORIENTED_EDGE('',*,*,#1281,.T.);
#1738=ORIENTED_EDGE('',*,*,#1282,.T.);
#1739=ORIENTED_EDGE('',*,*,#1283,.T.);
#1740=ORIENTED_EDGE('',*,*,#1284,.T.);
#1741=ORIENTED_EDGE('',*,*,#1285,.T.);
#1742=ORIENTED_EDGE('',*,*,#1286,.T.);
#1743=ORIENTED_EDGE('',*,*,#1287,.T.);
#1744=ORIENTED_EDGE('',*,*,#1288,.T.);
#1745=ORIENTED_EDGE('',*,*,#1289,.T.);
#1746=ORIENTED_EDGE('',*,*,#1290,.T.);
#1747=ORIENTED_EDGE('',*,*,#1291,.T.);
#1748=ORIENTED_EDGE('',*,*,#1292,.T.);
#1749=ORIENTED_EDGE('',*,*,#1293,.T.);
#1750=ORIENTED_EDGE('',*,*,#1294,.T.);
#1751=ORIENTED_EDGE('',*,*,#1295,.T.);
#1752=ORIENTED_EDGE('',*,*,#1296,.T.);
#1753=ORIENTED_EDGE('',*,*,#1297,.T.);
#1754=ORIENTED_EDGE('',*,*,#1298,.T.);
#1755=ORIENTED_EDGE('',*,*,#1299,.T.);
#1756=ORIENTED_EDGE('',*,*,#1300,.T.);
#1757=ORIENTED_EDGE('',*,*,#1301,.T.);
#1758=ORIENTED_EDGE('',*,*,#1302,.T.);
#1759=ORIENTED_EDGE('',*,*,#1303,.T.);
#1760=ORIENTED_EDGE('',*,*,#1304,.T.);
#1761=ORIENTED_EDGE('',*,*,#1305,.T.);
#1762=ORIENTED_EDGE('',*,*,#1306,.T.);
#1763=ORIENTED_EDGE('',*,*,#1307,.T.);
#1764=ORIENTED_EDGE('',*,*,#1308,.T.);
#1765=ORIENTED_EDGE('',*,*,#1309,.T.);
#1766=ORIENTED_EDGE('',*,*,#1310,.T.);
#1767=ORIENTED_EDGE('',*,*,#1311,.F.);
#1768=ORIENTED_EDGE('',*,*,#1312,.F.);
#1769=ORIENTED_EDGE('',*,*,#1313,.T.);
#1770=ORIENTED_EDGE('',*,*,#1314,.T.);
#1771=ORIENTED_EDGE('',*,*,#1315,.T.);
#1772=ORIENTED_EDGE('',*,*,#1316,.T.);
#1773=ORIENTED_EDGE('',*,*,#1317,.T.);
#1774=ORIENTED_EDGE('',*,*,#1318,.T.);
#1775=ORIENTED_EDGE('',*,*,#1319,.T.);
#1776=ORIENTED_EDGE('',*,*,#1320,.T.);
#1777=ORIENTED_EDGE('',*,*,#1321,.T.);
#1778=ORIENTED_EDGE('',*,*,#1322,.T.);
#1779=ORIENTED_EDGE('',*,*,#1323,.T.);
#1780=ORIENTED_EDGE('',*,*,#1324,.T.);
#1781=ORIENTED_EDGE('',*,*,#1325,.T.);
#1782=ORIENTED_EDGE('',*,*,#1326,.T.);
#1783=ORIENTED_EDGE('',*,*,#1327,.T.);
#1784=ORIENTED_EDGE('',*,*,#1328,.T.);
#1785=ORIENTED_EDGE('',*,*,#1329,.T.);
#1786=ORIENTED_EDGE('',*,*,#1330,.T.);
#1787=ORIENTED_EDGE('',*,*,#1331,.T.);
#1788=ORIENTED_EDGE('',*,*,#1332,.T.);
#1789=ORIENTED_EDGE('',*,*,#1333,.T.);
#1790=ORIENTED_EDGE('',*,*,#1334,.T.);
#1791=ORIENTED_EDGE('',*,*,#1335,.T.);
#1792=ORIENTED_EDGE('',*,*,#1336,.T.);
#1793=ORIENTED_EDGE('',*,*,#1337,.T.);
#1794=ORIENTED_EDGE('',*,*,#1338,.F.);
#1795=ORIENTED_EDGE('',*,*,#1339,.F.);
#1796=ORIENTED_EDGE('',*,*,#1340,.F.);
#1797=ORIENTED_EDGE('',*,*,#1341,.F.);
#1798=ORIENTED_EDGE('',*,*,#1342,.F.);
#1799=ORIENTED_EDGE('',*,*,#1343,.F.);
#1800=ORIENTED_EDGE('',*,*,#1344,.F.);
#1801=ORIENTED_EDGE('',*,*,#1345,.F.);
#1802=ORIENTED_EDGE('',*,*,#1346,.F.);
#1803=ORIENTED_EDGE('',*,*,#1347,.F.);
#1804=ORIENTED_EDGE('',*,*,#1348,.F.);
#1805=ORIENTED_EDGE('',*,*,#1349,.F.);
#1806=ORIENTED_EDGE('',*,*,#1350,.F.);
#1807=ORIENTED_EDGE('',*,*,#1351,.F.);
#1808=ORIENTED_EDGE('',*,*,#1352,.F.);
#1809=ORIENTED_EDGE('',*,*,#1353,.F.);
#1810=ORIENTED_EDGE('',*,*,#1354,.F.);
#1811=ORIENTED_EDGE('',*,*,#1355,.F.);
#1812=ORIENTED_EDGE('',*,*,#1356,.F.);
#1813=ORIENTED_EDGE('',*,*,#1357,.F.);
#1814=ORIENTED_EDGE('',*,*,#1358,.F.);
#1815=ORIENTED_EDGE('',*,*,#1359,.F.);
#1816=ORIENTED_EDGE('',*,*,#1360,.F.);
#1817=ORIENTED_EDGE('',*,*,#1361,.F.);
#1818=ORIENTED_EDGE('',*,*,#1362,.F.);
#1819=ORIENTED_EDGE('',*,*,#1363,.F.);
#1820=ORIENTED_EDGE('',*,*,#1364,.T.);
#1821=ORIENTED_EDGE('',*,*,#1365,.F.);
#1822=ORIENTED_EDGE('',*,*,#1364,.F.);
#1823=ORIENTED_EDGE('',*,*,#1366,.F.);
#1824=ORIENTED_EDGE('',*,*,#1367,.T.);
#1825=ORIENTED_EDGE('',*,*,#1368,.F.);
#1826=ORIENTED_EDGE('',*,*,#1369,.F.);
#1827=ORIENTED_EDGE('',*,*,#1367,.F.);
#1828=ORIENTED_EDGE('',*,*,#1366,.T.);
#1829=ORIENTED_EDGE('',*,*,#1365,.T.);
#1830=ORIENTED_EDGE('',*,*,#1370,.F.);
#1831=ORIENTED_EDGE('',*,*,#1271,.F.);
#1832=ORIENTED_EDGE('',*,*,#1270,.F.);
#1833=ORIENTED_EDGE('',*,*,#1269,.F.);
#1834=ORIENTED_EDGE('',*,*,#1268,.F.);
#1835=ORIENTED_EDGE('',*,*,#1267,.F.);
#1836=ORIENTED_EDGE('',*,*,#1266,.F.);
#1837=ORIENTED_EDGE('',*,*,#1265,.F.);
#1838=ORIENTED_EDGE('',*,*,#1264,.F.);
#1839=ORIENTED_EDGE('',*,*,#1263,.F.);
#1840=ORIENTED_EDGE('',*,*,#1262,.F.);
#1841=ORIENTED_EDGE('',*,*,#1261,.F.);
#1842=ORIENTED_EDGE('',*,*,#1260,.F.);
#1843=ORIENTED_EDGE('',*,*,#1259,.F.);
#1844=ORIENTED_EDGE('',*,*,#1258,.F.);
#1845=ORIENTED_EDGE('',*,*,#1257,.F.);
#1846=ORIENTED_EDGE('',*,*,#1256,.F.);
#1847=ORIENTED_EDGE('',*,*,#1255,.F.);
#1848=ORIENTED_EDGE('',*,*,#1254,.F.);
#1849=ORIENTED_EDGE('',*,*,#1253,.F.);
#1850=ORIENTED_EDGE('',*,*,#1252,.F.);
#1851=ORIENTED_EDGE('',*,*,#1251,.F.);
#1852=ORIENTED_EDGE('',*,*,#1250,.F.);
#1853=ORIENTED_EDGE('',*,*,#1249,.F.);
#1854=ORIENTED_EDGE('',*,*,#1248,.F.);
#1855=ORIENTED_EDGE('',*,*,#1247,.F.);
#1856=ORIENTED_EDGE('',*,*,#1246,.F.);
#1857=ORIENTED_EDGE('',*,*,#1245,.F.);
#1858=ORIENTED_EDGE('',*,*,#1244,.F.);
#1859=ORIENTED_EDGE('',*,*,#1243,.F.);
#1860=ORIENTED_EDGE('',*,*,#1242,.F.);
#1861=ORIENTED_EDGE('',*,*,#1241,.F.);
#1862=ORIENTED_EDGE('',*,*,#1240,.F.);
#1863=ORIENTED_EDGE('',*,*,#1239,.F.);
#1864=ORIENTED_EDGE('',*,*,#1238,.F.);
#1865=ORIENTED_EDGE('',*,*,#1237,.F.);
#1866=ORIENTED_EDGE('',*,*,#1236,.F.);
#1867=ORIENTED_EDGE('',*,*,#1235,.F.);
#1868=ORIENTED_EDGE('',*,*,#1234,.F.);
#1869=ORIENTED_EDGE('',*,*,#1233,.F.);
#1870=ORIENTED_EDGE('',*,*,#1371,.F.);
#1871=ORIENTED_EDGE('',*,*,#1372,.T.);
#1872=ORIENTED_EDGE('',*,*,#1311,.T.);
#1873=ORIENTED_EDGE('',*,*,#1362,.T.);
#1874=ORIENTED_EDGE('',*,*,#1361,.T.);
#1875=ORIENTED_EDGE('',*,*,#1360,.T.);
#1876=ORIENTED_EDGE('',*,*,#1359,.T.);
#1877=ORIENTED_EDGE('',*,*,#1358,.T.);
#1878=ORIENTED_EDGE('',*,*,#1357,.T.);
#1879=ORIENTED_EDGE('',*,*,#1356,.T.);
#1880=ORIENTED_EDGE('',*,*,#1355,.T.);
#1881=ORIENTED_EDGE('',*,*,#1354,.T.);
#1882=ORIENTED_EDGE('',*,*,#1353,.T.);
#1883=ORIENTED_EDGE('',*,*,#1352,.T.);
#1884=ORIENTED_EDGE('',*,*,#1351,.T.);
#1885=ORIENTED_EDGE('',*,*,#1350,.T.);
#1886=ORIENTED_EDGE('',*,*,#1349,.T.);
#1887=ORIENTED_EDGE('',*,*,#1348,.T.);
#1888=ORIENTED_EDGE('',*,*,#1347,.T.);
#1889=ORIENTED_EDGE('',*,*,#1346,.T.);
#1890=ORIENTED_EDGE('',*,*,#1345,.T.);
#1891=ORIENTED_EDGE('',*,*,#1344,.T.);
#1892=ORIENTED_EDGE('',*,*,#1343,.T.);
#1893=ORIENTED_EDGE('',*,*,#1342,.T.);
#1894=ORIENTED_EDGE('',*,*,#1341,.T.);
#1895=ORIENTED_EDGE('',*,*,#1340,.T.);
#1896=ORIENTED_EDGE('',*,*,#1339,.T.);
#1897=ORIENTED_EDGE('',*,*,#1373,.F.);
#1898=ORIENTED_EDGE('',*,*,#1337,.F.);
#1899=ORIENTED_EDGE('',*,*,#1336,.F.);
#1900=ORIENTED_EDGE('',*,*,#1335,.F.);
#1901=ORIENTED_EDGE('',*,*,#1334,.F.);
#1902=ORIENTED_EDGE('',*,*,#1333,.F.);
#1903=ORIENTED_EDGE('',*,*,#1332,.F.);
#1904=ORIENTED_EDGE('',*,*,#1331,.F.);
#1905=ORIENTED_EDGE('',*,*,#1330,.F.);
#1906=ORIENTED_EDGE('',*,*,#1329,.F.);
#1907=ORIENTED_EDGE('',*,*,#1328,.F.);
#1908=ORIENTED_EDGE('',*,*,#1327,.F.);
#1909=ORIENTED_EDGE('',*,*,#1326,.F.);
#1910=ORIENTED_EDGE('',*,*,#1325,.F.);
#1911=ORIENTED_EDGE('',*,*,#1324,.F.);
#1912=ORIENTED_EDGE('',*,*,#1323,.F.);
#1913=ORIENTED_EDGE('',*,*,#1322,.F.);
#1914=ORIENTED_EDGE('',*,*,#1321,.F.);
#1915=ORIENTED_EDGE('',*,*,#1320,.F.);
#1916=ORIENTED_EDGE('',*,*,#1319,.F.);
#1917=ORIENTED_EDGE('',*,*,#1318,.F.);
#1918=ORIENTED_EDGE('',*,*,#1317,.F.);
#1919=ORIENTED_EDGE('',*,*,#1316,.F.);
#1920=ORIENTED_EDGE('',*,*,#1315,.F.);
#1921=ORIENTED_EDGE('',*,*,#1314,.F.);
#1922=ORIENTED_EDGE('',*,*,#1313,.F.);
#1923=ORIENTED_EDGE('',*,*,#1374,.F.);
#1924=ORIENTED_EDGE('',*,*,#1231,.F.);
#1925=ORIENTED_EDGE('',*,*,#1310,.F.);
#1926=ORIENTED_EDGE('',*,*,#1309,.F.);
#1927=ORIENTED_EDGE('',*,*,#1308,.F.);
#1928=ORIENTED_EDGE('',*,*,#1307,.F.);
#1929=ORIENTED_EDGE('',*,*,#1306,.F.);
#1930=ORIENTED_EDGE('',*,*,#1305,.F.);
#1931=ORIENTED_EDGE('',*,*,#1304,.F.);
#1932=ORIENTED_EDGE('',*,*,#1303,.F.);
#1933=ORIENTED_EDGE('',*,*,#1302,.F.);
#1934=ORIENTED_EDGE('',*,*,#1301,.F.);
#1935=ORIENTED_EDGE('',*,*,#1300,.F.);
#1936=ORIENTED_EDGE('',*,*,#1299,.F.);
#1937=ORIENTED_EDGE('',*,*,#1298,.F.);
#1938=ORIENTED_EDGE('',*,*,#1297,.F.);
#1939=ORIENTED_EDGE('',*,*,#1296,.F.);
#1940=ORIENTED_EDGE('',*,*,#1295,.F.);
#1941=ORIENTED_EDGE('',*,*,#1294,.F.);
#1942=ORIENTED_EDGE('',*,*,#1293,.F.);
#1943=ORIENTED_EDGE('',*,*,#1292,.F.);
#1944=ORIENTED_EDGE('',*,*,#1291,.F.);
#1945=ORIENTED_EDGE('',*,*,#1290,.F.);
#1946=ORIENTED_EDGE('',*,*,#1289,.F.);
#1947=ORIENTED_EDGE('',*,*,#1288,.F.);
#1948=ORIENTED_EDGE('',*,*,#1287,.F.);
#1949=ORIENTED_EDGE('',*,*,#1286,.F.);
#1950=ORIENTED_EDGE('',*,*,#1285,.F.);
#1951=ORIENTED_EDGE('',*,*,#1284,.F.);
#1952=ORIENTED_EDGE('',*,*,#1283,.F.);
#1953=ORIENTED_EDGE('',*,*,#1282,.F.);
#1954=ORIENTED_EDGE('',*,*,#1281,.F.);
#1955=ORIENTED_EDGE('',*,*,#1280,.F.);
#1956=ORIENTED_EDGE('',*,*,#1279,.F.);
#1957=ORIENTED_EDGE('',*,*,#1278,.F.);
#1958=ORIENTED_EDGE('',*,*,#1277,.F.);
#1959=ORIENTED_EDGE('',*,*,#1276,.F.);
#1960=ORIENTED_EDGE('',*,*,#1275,.F.);
#1961=ORIENTED_EDGE('',*,*,#1274,.F.);
#1962=ORIENTED_EDGE('',*,*,#1273,.F.);
#1963=ORIENTED_EDGE('',*,*,#1375,.F.);
#1964=ORIENTED_EDGE('',*,*,#1376,.F.);
#1965=ORIENTED_EDGE('',*,*,#1377,.F.);
#1966=ORIENTED_EDGE('',*,*,#1378,.F.);
#1967=ORIENTED_EDGE('',*,*,#1379,.F.);
#1968=ORIENTED_EDGE('',*,*,#1380,.F.);
#1969=ORIENTED_EDGE('',*,*,#1381,.F.);
#1970=ORIENTED_EDGE('',*,*,#1382,.F.);
#1971=ORIENTED_EDGE('',*,*,#1383,.F.);
#1972=ORIENTED_EDGE('',*,*,#1384,.F.);
#1973=ORIENTED_EDGE('',*,*,#1385,.F.);
#1974=ORIENTED_EDGE('',*,*,#1386,.F.);
#1975=ORIENTED_EDGE('',*,*,#1387,.F.);
#1976=ORIENTED_EDGE('',*,*,#1388,.F.);
#1977=ORIENTED_EDGE('',*,*,#1389,.F.);
#1978=ORIENTED_EDGE('',*,*,#1390,.F.);
#1979=ORIENTED_EDGE('',*,*,#1391,.F.);
#1980=ORIENTED_EDGE('',*,*,#1392,.F.);
#1981=ORIENTED_EDGE('',*,*,#1393,.F.);
#1982=ORIENTED_EDGE('',*,*,#1394,.F.);
#1983=ORIENTED_EDGE('',*,*,#1395,.F.);
#1984=ORIENTED_EDGE('',*,*,#1396,.F.);
#1985=ORIENTED_EDGE('',*,*,#1397,.F.);
#1986=ORIENTED_EDGE('',*,*,#1398,.F.);
#1987=ORIENTED_EDGE('',*,*,#1399,.F.);
#1988=ORIENTED_EDGE('',*,*,#1400,.F.);
#1989=ORIENTED_EDGE('',*,*,#1401,.F.);
#1990=ORIENTED_EDGE('',*,*,#1402,.F.);
#1991=ORIENTED_EDGE('',*,*,#1403,.F.);
#1992=ORIENTED_EDGE('',*,*,#1404,.F.);
#1993=ORIENTED_EDGE('',*,*,#1405,.F.);
#1994=ORIENTED_EDGE('',*,*,#1406,.F.);
#1995=ORIENTED_EDGE('',*,*,#1407,.F.);
#1996=ORIENTED_EDGE('',*,*,#1408,.F.);
#1997=ORIENTED_EDGE('',*,*,#1409,.F.);
#1998=ORIENTED_EDGE('',*,*,#1410,.F.);
#1999=ORIENTED_EDGE('',*,*,#1411,.F.);
#2000=ORIENTED_EDGE('',*,*,#1412,.F.);
#2001=ORIENTED_EDGE('',*,*,#1413,.F.);
#2002=ORIENTED_EDGE('',*,*,#1414,.F.);
#2003=ORIENTED_EDGE('',*,*,#1415,.F.);
#2004=ORIENTED_EDGE('',*,*,#1416,.F.);
#2005=ORIENTED_EDGE('',*,*,#1417,.F.);
#2006=ORIENTED_EDGE('',*,*,#1418,.F.);
#2007=ORIENTED_EDGE('',*,*,#1419,.F.);
#2008=ORIENTED_EDGE('',*,*,#1420,.F.);
#2009=ORIENTED_EDGE('',*,*,#1421,.F.);
#2010=ORIENTED_EDGE('',*,*,#1422,.F.);
#2011=ORIENTED_EDGE('',*,*,#1423,.F.);
#2012=ORIENTED_EDGE('',*,*,#1424,.F.);
#2013=ORIENTED_EDGE('',*,*,#1425,.F.);
#2014=ORIENTED_EDGE('',*,*,#1426,.F.);
#2015=ORIENTED_EDGE('',*,*,#1427,.F.);
#2016=ORIENTED_EDGE('',*,*,#1428,.F.);
#2017=ORIENTED_EDGE('',*,*,#1429,.F.);
#2018=ORIENTED_EDGE('',*,*,#1430,.F.);
#2019=ORIENTED_EDGE('',*,*,#1431,.F.);
#2020=ORIENTED_EDGE('',*,*,#1432,.F.);
#2021=ORIENTED_EDGE('',*,*,#1433,.F.);
#2022=ORIENTED_EDGE('',*,*,#1434,.F.);
#2023=ORIENTED_EDGE('',*,*,#1435,.F.);
#2024=ORIENTED_EDGE('',*,*,#1436,.F.);
#2025=ORIENTED_EDGE('',*,*,#1437,.F.);
#2026=ORIENTED_EDGE('',*,*,#1438,.F.);
#2027=ORIENTED_EDGE('',*,*,#1439,.F.);
#2028=ORIENTED_EDGE('',*,*,#1440,.F.);
#2029=ORIENTED_EDGE('',*,*,#1441,.F.);
#2030=ORIENTED_EDGE('',*,*,#1442,.F.);
#2031=ORIENTED_EDGE('',*,*,#1443,.F.);
#2032=ORIENTED_EDGE('',*,*,#1444,.F.);
#2033=ORIENTED_EDGE('',*,*,#1445,.F.);
#2034=ORIENTED_EDGE('',*,*,#1446,.F.);
#2035=ORIENTED_EDGE('',*,*,#1447,.F.);
#2036=ORIENTED_EDGE('',*,*,#1448,.F.);
#2037=ORIENTED_EDGE('',*,*,#1449,.F.);
#2038=ORIENTED_EDGE('',*,*,#1450,.F.);
#2039=ORIENTED_EDGE('',*,*,#1451,.F.);
#2040=ORIENTED_EDGE('',*,*,#1452,.F.);
#2041=ORIENTED_EDGE('',*,*,#1453,.F.);
#2042=ORIENTED_EDGE('',*,*,#1454,.F.);
#2043=ORIENTED_EDGE('',*,*,#1455,.F.);
#2044=ORIENTED_EDGE('',*,*,#1456,.F.);
#2045=ORIENTED_EDGE('',*,*,#1457,.F.);
#2046=ORIENTED_EDGE('',*,*,#1458,.F.);
#2047=ORIENTED_EDGE('',*,*,#1459,.F.);
#2048=ORIENTED_EDGE('',*,*,#1460,.F.);
#2049=ORIENTED_EDGE('',*,*,#1461,.F.);
#2050=ORIENTED_EDGE('',*,*,#1462,.F.);
#2051=ORIENTED_EDGE('',*,*,#1463,.F.);
#2052=ORIENTED_EDGE('',*,*,#1464,.F.);
#2053=ORIENTED_EDGE('',*,*,#1465,.F.);
#2054=ORIENTED_EDGE('',*,*,#1466,.F.);
#2055=ORIENTED_EDGE('',*,*,#1467,.F.);
#2056=ORIENTED_EDGE('',*,*,#1468,.F.);
#2057=ORIENTED_EDGE('',*,*,#1469,.F.);
#2058=ORIENTED_EDGE('',*,*,#1470,.F.);
#2059=ORIENTED_EDGE('',*,*,#1471,.F.);
#2060=ORIENTED_EDGE('',*,*,#1472,.F.);
#2061=ORIENTED_EDGE('',*,*,#1473,.F.);
#2062=ORIENTED_EDGE('',*,*,#1474,.F.);
#2063=ORIENTED_EDGE('',*,*,#1475,.F.);
#2064=ORIENTED_EDGE('',*,*,#1476,.F.);
#2065=ORIENTED_EDGE('',*,*,#1477,.F.);
#2066=ORIENTED_EDGE('',*,*,#1478,.F.);
#2067=ORIENTED_EDGE('',*,*,#1479,.F.);
#2068=ORIENTED_EDGE('',*,*,#1480,.F.);
#2069=ORIENTED_EDGE('',*,*,#1481,.F.);
#2070=ORIENTED_EDGE('',*,*,#1482,.F.);
#2071=ORIENTED_EDGE('',*,*,#1483,.F.);
#2072=ORIENTED_EDGE('',*,*,#1484,.F.);
#2073=ORIENTED_EDGE('',*,*,#1485,.F.);
#2074=ORIENTED_EDGE('',*,*,#1486,.F.);
#2075=ORIENTED_EDGE('',*,*,#1487,.F.);
#2076=ORIENTED_EDGE('',*,*,#1488,.F.);
#2077=ORIENTED_EDGE('',*,*,#1489,.F.);
#2078=ORIENTED_EDGE('',*,*,#1490,.F.);
#2079=ORIENTED_EDGE('',*,*,#1491,.F.);
#2080=ORIENTED_EDGE('',*,*,#1492,.F.);
#2081=ORIENTED_EDGE('',*,*,#1493,.F.);
#2082=ORIENTED_EDGE('',*,*,#1494,.F.);
#2083=ORIENTED_EDGE('',*,*,#1495,.F.);
#2084=ORIENTED_EDGE('',*,*,#1496,.F.);
#2085=ORIENTED_EDGE('',*,*,#1497,.F.);
#2086=ORIENTED_EDGE('',*,*,#1498,.F.);
#2087=ORIENTED_EDGE('',*,*,#1499,.F.);
#2088=ORIENTED_EDGE('',*,*,#1500,.F.);
#2089=ORIENTED_EDGE('',*,*,#1501,.F.);
#2090=ORIENTED_EDGE('',*,*,#1502,.F.);
#2091=ORIENTED_EDGE('',*,*,#1503,.F.);
#2092=ORIENTED_EDGE('',*,*,#1504,.F.);
#2093=ORIENTED_EDGE('',*,*,#1505,.F.);
#2094=ORIENTED_EDGE('',*,*,#1506,.F.);
#2095=ORIENTED_EDGE('',*,*,#1507,.F.);
#2096=ORIENTED_EDGE('',*,*,#1508,.F.);
#2097=ORIENTED_EDGE('',*,*,#1509,.F.);
#2098=ORIENTED_EDGE('',*,*,#1510,.F.);
#2099=ORIENTED_EDGE('',*,*,#1511,.F.);
#2100=ORIENTED_EDGE('',*,*,#1512,.F.);
#2101=ORIENTED_EDGE('',*,*,#1513,.F.);
#2102=ORIENTED_EDGE('',*,*,#1514,.F.);
#2103=ORIENTED_EDGE('',*,*,#1515,.F.);
#2104=ORIENTED_EDGE('',*,*,#1516,.F.);
#2105=ORIENTED_EDGE('',*,*,#1517,.F.);
#2106=ORIENTED_EDGE('',*,*,#1518,.F.);
#2107=ORIENTED_EDGE('',*,*,#1519,.F.);
#2108=ORIENTED_EDGE('',*,*,#1520,.F.);
#2109=ORIENTED_EDGE('',*,*,#1521,.F.);
#2110=ORIENTED_EDGE('',*,*,#1522,.F.);
#2111=ORIENTED_EDGE('',*,*,#1523,.F.);
#2112=ORIENTED_EDGE('',*,*,#1524,.F.);
#2113=ORIENTED_EDGE('',*,*,#1525,.F.);
#2114=ORIENTED_EDGE('',*,*,#1526,.F.);
#2115=ORIENTED_EDGE('',*,*,#1527,.F.);
#2116=ORIENTED_EDGE('',*,*,#1528,.F.);
#2117=ORIENTED_EDGE('',*,*,#1529,.F.);
#2118=ORIENTED_EDGE('',*,*,#1530,.F.);
#2119=ORIENTED_EDGE('',*,*,#1531,.F.);
#2120=ORIENTED_EDGE('',*,*,#1377,.T.);
#2121=ORIENTED_EDGE('',*,*,#1532,.F.);
#2122=ORIENTED_EDGE('',*,*,#1381,.T.);
#2123=ORIENTED_EDGE('',*,*,#1533,.F.);
#2124=ORIENTED_EDGE('',*,*,#1385,.T.);
#2125=ORIENTED_EDGE('',*,*,#1534,.F.);
#2126=ORIENTED_EDGE('',*,*,#1389,.T.);
#2127=ORIENTED_EDGE('',*,*,#1535,.F.);
#2128=ORIENTED_EDGE('',*,*,#1393,.T.);
#2129=ORIENTED_EDGE('',*,*,#1536,.F.);
#2130=ORIENTED_EDGE('',*,*,#1397,.T.);
#2131=ORIENTED_EDGE('',*,*,#1537,.F.);
#2132=ORIENTED_EDGE('',*,*,#1401,.T.);
#2133=ORIENTED_EDGE('',*,*,#1538,.F.);
#2134=ORIENTED_EDGE('',*,*,#1405,.T.);
#2135=ORIENTED_EDGE('',*,*,#1539,.F.);
#2136=ORIENTED_EDGE('',*,*,#1409,.T.);
#2137=ORIENTED_EDGE('',*,*,#1540,.F.);
#2138=ORIENTED_EDGE('',*,*,#1413,.T.);
#2139=ORIENTED_EDGE('',*,*,#1541,.F.);
#2140=ORIENTED_EDGE('',*,*,#1418,.T.);
#2141=ORIENTED_EDGE('',*,*,#1542,.F.);
#2142=ORIENTED_EDGE('',*,*,#1422,.T.);
#2143=ORIENTED_EDGE('',*,*,#1543,.F.);
#2144=ORIENTED_EDGE('',*,*,#1426,.T.);
#2145=ORIENTED_EDGE('',*,*,#1544,.F.);
#2146=ORIENTED_EDGE('',*,*,#1430,.T.);
#2147=ORIENTED_EDGE('',*,*,#1545,.F.);
#2148=ORIENTED_EDGE('',*,*,#1434,.T.);
#2149=ORIENTED_EDGE('',*,*,#1546,.F.);
#2150=ORIENTED_EDGE('',*,*,#1438,.T.);
#2151=ORIENTED_EDGE('',*,*,#1547,.F.);
#2152=ORIENTED_EDGE('',*,*,#1442,.T.);
#2153=ORIENTED_EDGE('',*,*,#1548,.F.);
#2154=ORIENTED_EDGE('',*,*,#1446,.T.);
#2155=ORIENTED_EDGE('',*,*,#1549,.F.);
#2156=ORIENTED_EDGE('',*,*,#1450,.T.);
#2157=ORIENTED_EDGE('',*,*,#1550,.F.);
#2158=ORIENTED_EDGE('',*,*,#1454,.T.);
#2159=ORIENTED_EDGE('',*,*,#1551,.F.);
#2160=ORIENTED_EDGE('',*,*,#1458,.T.);
#2161=ORIENTED_EDGE('',*,*,#1552,.F.);
#2162=ORIENTED_EDGE('',*,*,#1462,.T.);
#2163=ORIENTED_EDGE('',*,*,#1553,.F.);
#2164=ORIENTED_EDGE('',*,*,#1466,.T.);
#2165=ORIENTED_EDGE('',*,*,#1554,.F.);
#2166=ORIENTED_EDGE('',*,*,#1470,.T.);
#2167=ORIENTED_EDGE('',*,*,#1555,.F.);
#2168=ORIENTED_EDGE('',*,*,#1474,.T.);
#2169=ORIENTED_EDGE('',*,*,#1556,.F.);
#2170=ORIENTED_EDGE('',*,*,#1478,.T.);
#2171=ORIENTED_EDGE('',*,*,#1557,.F.);
#2172=ORIENTED_EDGE('',*,*,#1482,.T.);
#2173=ORIENTED_EDGE('',*,*,#1558,.F.);
#2174=ORIENTED_EDGE('',*,*,#1486,.T.);
#2175=ORIENTED_EDGE('',*,*,#1559,.F.);
#2176=ORIENTED_EDGE('',*,*,#1490,.T.);
#2177=ORIENTED_EDGE('',*,*,#1560,.F.);
#2178=ORIENTED_EDGE('',*,*,#1494,.T.);
#2179=ORIENTED_EDGE('',*,*,#1561,.F.);
#2180=ORIENTED_EDGE('',*,*,#1498,.T.);
#2181=ORIENTED_EDGE('',*,*,#1562,.F.);
#2182=ORIENTED_EDGE('',*,*,#1502,.T.);
#2183=ORIENTED_EDGE('',*,*,#1563,.F.);
#2184=ORIENTED_EDGE('',*,*,#1506,.T.);
#2185=ORIENTED_EDGE('',*,*,#1564,.F.);
#2186=ORIENTED_EDGE('',*,*,#1510,.T.);
#2187=ORIENTED_EDGE('',*,*,#1565,.F.);
#2188=ORIENTED_EDGE('',*,*,#1514,.T.);
#2189=ORIENTED_EDGE('',*,*,#1566,.F.);
#2190=ORIENTED_EDGE('',*,*,#1518,.T.);
#2191=ORIENTED_EDGE('',*,*,#1567,.F.);
#2192=ORIENTED_EDGE('',*,*,#1522,.T.);
#2193=ORIENTED_EDGE('',*,*,#1568,.F.);
#2194=ORIENTED_EDGE('',*,*,#1526,.T.);
#2195=ORIENTED_EDGE('',*,*,#1569,.F.);
#2196=ORIENTED_EDGE('',*,*,#1530,.T.);
#2197=ORIENTED_EDGE('',*,*,#1570,.F.);
#2198=ORIENTED_EDGE('',*,*,#1571,.T.);
#2199=ORIENTED_EDGE('',*,*,#1572,.F.);
#2200=ORIENTED_EDGE('',*,*,#1529,.T.);
#2201=ORIENTED_EDGE('',*,*,#1573,.F.);
#2202=ORIENTED_EDGE('',*,*,#1574,.T.);
#2203=ORIENTED_EDGE('',*,*,#1570,.T.);
#2204=ORIENTED_EDGE('',*,*,#1525,.T.);
#2205=ORIENTED_EDGE('',*,*,#1575,.F.);
#2206=ORIENTED_EDGE('',*,*,#1531,.T.);
#2207=ORIENTED_EDGE('',*,*,#1569,.T.);
#2208=ORIENTED_EDGE('',*,*,#1521,.T.);
#2209=ORIENTED_EDGE('',*,*,#1576,.F.);
#2210=ORIENTED_EDGE('',*,*,#1527,.T.);
#2211=ORIENTED_EDGE('',*,*,#1568,.T.);
#2212=ORIENTED_EDGE('',*,*,#1517,.T.);
#2213=ORIENTED_EDGE('',*,*,#1577,.F.);
#2214=ORIENTED_EDGE('',*,*,#1523,.T.);
#2215=ORIENTED_EDGE('',*,*,#1567,.T.);
#2216=ORIENTED_EDGE('',*,*,#1513,.T.);
#2217=ORIENTED_EDGE('',*,*,#1578,.F.);
#2218=ORIENTED_EDGE('',*,*,#1519,.T.);
#2219=ORIENTED_EDGE('',*,*,#1566,.T.);
#2220=ORIENTED_EDGE('',*,*,#1509,.T.);
#2221=ORIENTED_EDGE('',*,*,#1579,.F.);
#2222=ORIENTED_EDGE('',*,*,#1515,.T.);
#2223=ORIENTED_EDGE('',*,*,#1565,.T.);
#2224=ORIENTED_EDGE('',*,*,#1505,.T.);
#2225=ORIENTED_EDGE('',*,*,#1580,.F.);
#2226=ORIENTED_EDGE('',*,*,#1511,.T.);
#2227=ORIENTED_EDGE('',*,*,#1564,.T.);
#2228=ORIENTED_EDGE('',*,*,#1501,.T.);
#2229=ORIENTED_EDGE('',*,*,#1581,.F.);
#2230=ORIENTED_EDGE('',*,*,#1507,.T.);
#2231=ORIENTED_EDGE('',*,*,#1563,.T.);
#2232=ORIENTED_EDGE('',*,*,#1497,.T.);
#2233=ORIENTED_EDGE('',*,*,#1582,.F.);
#2234=ORIENTED_EDGE('',*,*,#1503,.T.);
#2235=ORIENTED_EDGE('',*,*,#1562,.T.);
#2236=ORIENTED_EDGE('',*,*,#1493,.T.);
#2237=ORIENTED_EDGE('',*,*,#1583,.F.);
#2238=ORIENTED_EDGE('',*,*,#1499,.T.);
#2239=ORIENTED_EDGE('',*,*,#1561,.T.);
#2240=ORIENTED_EDGE('',*,*,#1489,.T.);
#2241=ORIENTED_EDGE('',*,*,#1584,.F.);
#2242=ORIENTED_EDGE('',*,*,#1495,.T.);
#2243=ORIENTED_EDGE('',*,*,#1560,.T.);
#2244=ORIENTED_EDGE('',*,*,#1485,.T.);
#2245=ORIENTED_EDGE('',*,*,#1585,.F.);
#2246=ORIENTED_EDGE('',*,*,#1491,.T.);
#2247=ORIENTED_EDGE('',*,*,#1559,.T.);
#2248=ORIENTED_EDGE('',*,*,#1481,.T.);
#2249=ORIENTED_EDGE('',*,*,#1586,.F.);
#2250=ORIENTED_EDGE('',*,*,#1487,.T.);
#2251=ORIENTED_EDGE('',*,*,#1558,.T.);
#2252=ORIENTED_EDGE('',*,*,#1477,.T.);
#2253=ORIENTED_EDGE('',*,*,#1587,.F.);
#2254=ORIENTED_EDGE('',*,*,#1483,.T.);
#2255=ORIENTED_EDGE('',*,*,#1557,.T.);
#2256=ORIENTED_EDGE('',*,*,#1473,.T.);
#2257=ORIENTED_EDGE('',*,*,#1588,.F.);
#2258=ORIENTED_EDGE('',*,*,#1479,.T.);
#2259=ORIENTED_EDGE('',*,*,#1556,.T.);
#2260=ORIENTED_EDGE('',*,*,#1469,.T.);
#2261=ORIENTED_EDGE('',*,*,#1589,.F.);
#2262=ORIENTED_EDGE('',*,*,#1475,.T.);
#2263=ORIENTED_EDGE('',*,*,#1555,.T.);
#2264=ORIENTED_EDGE('',*,*,#1465,.T.);
#2265=ORIENTED_EDGE('',*,*,#1590,.F.);
#2266=ORIENTED_EDGE('',*,*,#1471,.T.);
#2267=ORIENTED_EDGE('',*,*,#1554,.T.);
#2268=ORIENTED_EDGE('',*,*,#1461,.T.);
#2269=ORIENTED_EDGE('',*,*,#1591,.F.);
#2270=ORIENTED_EDGE('',*,*,#1467,.T.);
#2271=ORIENTED_EDGE('',*,*,#1553,.T.);
#2272=ORIENTED_EDGE('',*,*,#1457,.T.);
#2273=ORIENTED_EDGE('',*,*,#1592,.F.);
#2274=ORIENTED_EDGE('',*,*,#1463,.T.);
#2275=ORIENTED_EDGE('',*,*,#1552,.T.);
#2276=ORIENTED_EDGE('',*,*,#1453,.T.);
#2277=ORIENTED_EDGE('',*,*,#1593,.F.);
#2278=ORIENTED_EDGE('',*,*,#1459,.T.);
#2279=ORIENTED_EDGE('',*,*,#1551,.T.);
#2280=ORIENTED_EDGE('',*,*,#1449,.T.);
#2281=ORIENTED_EDGE('',*,*,#1594,.F.);
#2282=ORIENTED_EDGE('',*,*,#1455,.T.);
#2283=ORIENTED_EDGE('',*,*,#1550,.T.);
#2284=ORIENTED_EDGE('',*,*,#1445,.T.);
#2285=ORIENTED_EDGE('',*,*,#1595,.F.);
#2286=ORIENTED_EDGE('',*,*,#1451,.T.);
#2287=ORIENTED_EDGE('',*,*,#1549,.T.);
#2288=ORIENTED_EDGE('',*,*,#1441,.T.);
#2289=ORIENTED_EDGE('',*,*,#1596,.F.);
#2290=ORIENTED_EDGE('',*,*,#1447,.T.);
#2291=ORIENTED_EDGE('',*,*,#1548,.T.);
#2292=ORIENTED_EDGE('',*,*,#1437,.T.);
#2293=ORIENTED_EDGE('',*,*,#1597,.F.);
#2294=ORIENTED_EDGE('',*,*,#1443,.T.);
#2295=ORIENTED_EDGE('',*,*,#1547,.T.);
#2296=ORIENTED_EDGE('',*,*,#1433,.T.);
#2297=ORIENTED_EDGE('',*,*,#1598,.F.);
#2298=ORIENTED_EDGE('',*,*,#1439,.T.);
#2299=ORIENTED_EDGE('',*,*,#1546,.T.);
#2300=ORIENTED_EDGE('',*,*,#1429,.T.);
#2301=ORIENTED_EDGE('',*,*,#1599,.F.);
#2302=ORIENTED_EDGE('',*,*,#1435,.T.);
#2303=ORIENTED_EDGE('',*,*,#1545,.T.);
#2304=ORIENTED_EDGE('',*,*,#1425,.T.);
#2305=ORIENTED_EDGE('',*,*,#1600,.F.);
#2306=ORIENTED_EDGE('',*,*,#1431,.T.);
#2307=ORIENTED_EDGE('',*,*,#1544,.T.);
#2308=ORIENTED_EDGE('',*,*,#1421,.T.);
#2309=ORIENTED_EDGE('',*,*,#1601,.F.);
#2310=ORIENTED_EDGE('',*,*,#1427,.T.);
#2311=ORIENTED_EDGE('',*,*,#1543,.T.);
#2312=ORIENTED_EDGE('',*,*,#1417,.T.);
#2313=ORIENTED_EDGE('',*,*,#1602,.F.);
#2314=ORIENTED_EDGE('',*,*,#1423,.T.);
#2315=ORIENTED_EDGE('',*,*,#1542,.T.);
#2316=ORIENTED_EDGE('',*,*,#1412,.T.);
#2317=ORIENTED_EDGE('',*,*,#1603,.F.);
#2318=ORIENTED_EDGE('',*,*,#1419,.T.);
#2319=ORIENTED_EDGE('',*,*,#1541,.T.);
#2320=ORIENTED_EDGE('',*,*,#1408,.T.);
#2321=ORIENTED_EDGE('',*,*,#1604,.F.);
#2322=ORIENTED_EDGE('',*,*,#1414,.T.);
#2323=ORIENTED_EDGE('',*,*,#1540,.T.);
#2324=ORIENTED_EDGE('',*,*,#1404,.T.);
#2325=ORIENTED_EDGE('',*,*,#1605,.F.);
#2326=ORIENTED_EDGE('',*,*,#1410,.T.);
#2327=ORIENTED_EDGE('',*,*,#1539,.T.);
#2328=ORIENTED_EDGE('',*,*,#1400,.T.);
#2329=ORIENTED_EDGE('',*,*,#1606,.F.);
#2330=ORIENTED_EDGE('',*,*,#1406,.T.);
#2331=ORIENTED_EDGE('',*,*,#1538,.T.);
#2332=ORIENTED_EDGE('',*,*,#1396,.T.);
#2333=ORIENTED_EDGE('',*,*,#1607,.F.);
#2334=ORIENTED_EDGE('',*,*,#1402,.T.);
#2335=ORIENTED_EDGE('',*,*,#1537,.T.);
#2336=ORIENTED_EDGE('',*,*,#1392,.T.);
#2337=ORIENTED_EDGE('',*,*,#1608,.F.);
#2338=ORIENTED_EDGE('',*,*,#1398,.T.);
#2339=ORIENTED_EDGE('',*,*,#1536,.T.);
#2340=ORIENTED_EDGE('',*,*,#1388,.T.);
#2341=ORIENTED_EDGE('',*,*,#1609,.F.);
#2342=ORIENTED_EDGE('',*,*,#1394,.T.);
#2343=ORIENTED_EDGE('',*,*,#1535,.T.);
#2344=ORIENTED_EDGE('',*,*,#1384,.T.);
#2345=ORIENTED_EDGE('',*,*,#1610,.F.);
#2346=ORIENTED_EDGE('',*,*,#1390,.T.);
#2347=ORIENTED_EDGE('',*,*,#1534,.T.);
#2348=ORIENTED_EDGE('',*,*,#1380,.T.);
#2349=ORIENTED_EDGE('',*,*,#1611,.F.);
#2350=ORIENTED_EDGE('',*,*,#1386,.T.);
#2351=ORIENTED_EDGE('',*,*,#1533,.T.);
#2352=ORIENTED_EDGE('',*,*,#1376,.T.);
#2353=ORIENTED_EDGE('',*,*,#1612,.F.);
#2354=ORIENTED_EDGE('',*,*,#1382,.T.);
#2355=ORIENTED_EDGE('',*,*,#1532,.T.);
#2356=ORIENTED_EDGE('',*,*,#1368,.T.);
#2357=ORIENTED_EDGE('',*,*,#1369,.T.);
#2358=ORIENTED_EDGE('',*,*,#1613,.T.);
#2359=ORIENTED_EDGE('',*,*,#1415,.T.);
#2360=ORIENTED_EDGE('',*,*,#1604,.T.);
#2361=ORIENTED_EDGE('',*,*,#1407,.T.);
#2362=ORIENTED_EDGE('',*,*,#1605,.T.);
#2363=ORIENTED_EDGE('',*,*,#1403,.T.);
#2364=ORIENTED_EDGE('',*,*,#1606,.T.);
#2365=ORIENTED_EDGE('',*,*,#1399,.T.);
#2366=ORIENTED_EDGE('',*,*,#1607,.T.);
#2367=ORIENTED_EDGE('',*,*,#1395,.T.);
#2368=ORIENTED_EDGE('',*,*,#1608,.T.);
#2369=ORIENTED_EDGE('',*,*,#1391,.T.);
#2370=ORIENTED_EDGE('',*,*,#1609,.T.);
#2371=ORIENTED_EDGE('',*,*,#1387,.T.);
#2372=ORIENTED_EDGE('',*,*,#1610,.T.);
#2373=ORIENTED_EDGE('',*,*,#1383,.T.);
#2374=ORIENTED_EDGE('',*,*,#1611,.T.);
#2375=ORIENTED_EDGE('',*,*,#1379,.T.);
#2376=ORIENTED_EDGE('',*,*,#1612,.T.);
#2377=ORIENTED_EDGE('',*,*,#1375,.T.);
#2378=ORIENTED_EDGE('',*,*,#1614,.T.);
#2379=ORIENTED_EDGE('',*,*,#1615,.T.);
#2380=ORIENTED_EDGE('',*,*,#1573,.T.);
#2381=ORIENTED_EDGE('',*,*,#1528,.T.);
#2382=ORIENTED_EDGE('',*,*,#1575,.T.);
#2383=ORIENTED_EDGE('',*,*,#1524,.T.);
#2384=ORIENTED_EDGE('',*,*,#1576,.T.);
#2385=ORIENTED_EDGE('',*,*,#1520,.T.);
#2386=ORIENTED_EDGE('',*,*,#1577,.T.);
#2387=ORIENTED_EDGE('',*,*,#1516,.T.);
#2388=ORIENTED_EDGE('',*,*,#1578,.T.);
#2389=ORIENTED_EDGE('',*,*,#1512,.T.);
#2390=ORIENTED_EDGE('',*,*,#1579,.T.);
#2391=ORIENTED_EDGE('',*,*,#1508,.T.);
#2392=ORIENTED_EDGE('',*,*,#1580,.T.);
#2393=ORIENTED_EDGE('',*,*,#1504,.T.);
#2394=ORIENTED_EDGE('',*,*,#1581,.T.);
#2395=ORIENTED_EDGE('',*,*,#1500,.T.);
#2396=ORIENTED_EDGE('',*,*,#1582,.T.);
#2397=ORIENTED_EDGE('',*,*,#1496,.T.);
#2398=ORIENTED_EDGE('',*,*,#1583,.T.);
#2399=ORIENTED_EDGE('',*,*,#1492,.T.);
#2400=ORIENTED_EDGE('',*,*,#1584,.T.);
#2401=ORIENTED_EDGE('',*,*,#1488,.T.);
#2402=ORIENTED_EDGE('',*,*,#1585,.T.);
#2403=ORIENTED_EDGE('',*,*,#1484,.T.);
#2404=ORIENTED_EDGE('',*,*,#1586,.T.);
#2405=ORIENTED_EDGE('',*,*,#1480,.T.);
#2406=ORIENTED_EDGE('',*,*,#1587,.T.);
#2407=ORIENTED_EDGE('',*,*,#1476,.T.);
#2408=ORIENTED_EDGE('',*,*,#1588,.T.);
#2409=ORIENTED_EDGE('',*,*,#1472,.T.);
#2410=ORIENTED_EDGE('',*,*,#1589,.T.);
#2411=ORIENTED_EDGE('',*,*,#1468,.T.);
#2412=ORIENTED_EDGE('',*,*,#1590,.T.);
#2413=ORIENTED_EDGE('',*,*,#1464,.T.);
#2414=ORIENTED_EDGE('',*,*,#1591,.T.);
#2415=ORIENTED_EDGE('',*,*,#1460,.T.);
#2416=ORIENTED_EDGE('',*,*,#1592,.T.);
#2417=ORIENTED_EDGE('',*,*,#1456,.T.);
#2418=ORIENTED_EDGE('',*,*,#1593,.T.);
#2419=ORIENTED_EDGE('',*,*,#1452,.T.);
#2420=ORIENTED_EDGE('',*,*,#1594,.T.);
#2421=ORIENTED_EDGE('',*,*,#1448,.T.);
#2422=ORIENTED_EDGE('',*,*,#1595,.T.);
#2423=ORIENTED_EDGE('',*,*,#1444,.T.);
#2424=ORIENTED_EDGE('',*,*,#1596,.T.);
#2425=ORIENTED_EDGE('',*,*,#1440,.T.);
#2426=ORIENTED_EDGE('',*,*,#1597,.T.);
#2427=ORIENTED_EDGE('',*,*,#1436,.T.);
#2428=ORIENTED_EDGE('',*,*,#1598,.T.);
#2429=ORIENTED_EDGE('',*,*,#1432,.T.);
#2430=ORIENTED_EDGE('',*,*,#1599,.T.);
#2431=ORIENTED_EDGE('',*,*,#1428,.T.);
#2432=ORIENTED_EDGE('',*,*,#1600,.T.);
#2433=ORIENTED_EDGE('',*,*,#1424,.T.);
#2434=ORIENTED_EDGE('',*,*,#1601,.T.);
#2435=ORIENTED_EDGE('',*,*,#1420,.T.);
#2436=ORIENTED_EDGE('',*,*,#1602,.T.);
#2437=ORIENTED_EDGE('',*,*,#1416,.T.);
#2438=ORIENTED_EDGE('',*,*,#1603,.T.);
#2439=ORIENTED_EDGE('',*,*,#1411,.T.);
#2440=ORIENTED_EDGE('',*,*,#1613,.F.);
#2441=ORIENTED_EDGE('',*,*,#1615,.F.);
#2442=ORIENTED_EDGE('',*,*,#1616,.F.);
#2443=ORIENTED_EDGE('',*,*,#1571,.F.);
#2444=ORIENTED_EDGE('',*,*,#1574,.F.);
#2445=ORIENTED_EDGE('',*,*,#1378,.T.);
#2446=ORIENTED_EDGE('',*,*,#1572,.T.);
#2447=ORIENTED_EDGE('',*,*,#1616,.T.);
#2448=ORIENTED_EDGE('',*,*,#1614,.F.);
#2449=ORIENTED_EDGE('',*,*,#1363,.T.);
#2450=ORIENTED_EDGE('',*,*,#1374,.T.);
#2451=ORIENTED_EDGE('',*,*,#1312,.T.);
#2452=ORIENTED_EDGE('',*,*,#1372,.F.);
#2453=ORIENTED_EDGE('',*,*,#1371,.T.);
#2454=ORIENTED_EDGE('',*,*,#1232,.F.);
#2455=ORIENTED_EDGE('',*,*,#1373,.T.);
#2456=ORIENTED_EDGE('',*,*,#1272,.T.);
#2457=ORIENTED_EDGE('',*,*,#1370,.T.);
#2458=ORIENTED_EDGE('',*,*,#1338,.T.);
#2459=ORIENTED_EDGE('',*,*,#1617,.F.);
#2460=ORIENTED_EDGE('',*,*,#1618,.T.);
#2461=ORIENTED_EDGE('',*,*,#1619,.T.);
#2462=ORIENTED_EDGE('',*,*,#1618,.F.);
#2463=ORIENTED_EDGE('',*,*,#1620,.T.);
#2464=ORIENTED_EDGE('',*,*,#1621,.T.);
#2465=ORIENTED_EDGE('',*,*,#1617,.T.);
#2466=ORIENTED_EDGE('',*,*,#1621,.F.);
#2467=ORIENTED_EDGE('',*,*,#1622,.F.);
#2468=ORIENTED_EDGE('',*,*,#1623,.T.);
#2469=ORIENTED_EDGE('',*,*,#1620,.F.);
#2470=ORIENTED_EDGE('',*,*,#1623,.F.);
#2471=ORIENTED_EDGE('',*,*,#1624,.F.);
#2472=ORIENTED_EDGE('',*,*,#1625,.F.);
#2473=ORIENTED_EDGE('',*,*,#1626,.T.);
#2474=ORIENTED_EDGE('',*,*,#1622,.T.);
#2475=ORIENTED_EDGE('',*,*,#1626,.F.);
#2476=ORIENTED_EDGE('',*,*,#1627,.T.);
#2477=ORIENTED_EDGE('',*,*,#1624,.T.);
#2478=ORIENTED_EDGE('',*,*,#1625,.T.);
#2479=ORIENTED_EDGE('',*,*,#1627,.F.);
#2480=ORIENTED_EDGE('',*,*,#1628,.F.);
#2481=ORIENTED_EDGE('',*,*,#1629,.F.);
#2482=ORIENTED_EDGE('',*,*,#1630,.F.);
#2483=ORIENTED_EDGE('',*,*,#1631,.F.);
#2484=ORIENTED_EDGE('',*,*,#1632,.T.);
#2485=ORIENTED_EDGE('',*,*,#1628,.T.);
#2486=ORIENTED_EDGE('',*,*,#1629,.T.);
#2487=ORIENTED_EDGE('',*,*,#1632,.F.);
#2488=ORIENTED_EDGE('',*,*,#1633,.F.);
#2489=ORIENTED_EDGE('',*,*,#1630,.T.);
#2490=ORIENTED_EDGE('',*,*,#1631,.T.);
#2491=ORIENTED_EDGE('',*,*,#1633,.T.);
#2492=ORIENTED_EDGE('',*,*,#1634,.F.);
#2493=ORIENTED_EDGE('',*,*,#1635,.F.);
#2494=ORIENTED_EDGE('',*,*,#1619,.F.);
#2495=ORIENTED_EDGE('',*,*,#1636,.T.);
#2496=ORIENTED_EDGE('',*,*,#1634,.T.);
#2497=ORIENTED_EDGE('',*,*,#1635,.T.);
#2498=ORIENTED_EDGE('',*,*,#1636,.F.);
#2499=ORIENTED_EDGE('',*,*,#1637,.F.);
#2500=ORIENTED_EDGE('',*,*,#1638,.T.);
#2501=ORIENTED_EDGE('',*,*,#1639,.T.);
#2502=ORIENTED_EDGE('',*,*,#1638,.F.);
#2503=ORIENTED_EDGE('',*,*,#1640,.T.);
#2504=ORIENTED_EDGE('',*,*,#1641,.T.);
#2505=ORIENTED_EDGE('',*,*,#1637,.T.);
#2506=ORIENTED_EDGE('',*,*,#1641,.F.);
#2507=ORIENTED_EDGE('',*,*,#1642,.F.);
#2508=ORIENTED_EDGE('',*,*,#1643,.T.);
#2509=ORIENTED_EDGE('',*,*,#1640,.F.);
#2510=ORIENTED_EDGE('',*,*,#1643,.F.);
#2511=ORIENTED_EDGE('',*,*,#1644,.F.);
#2512=ORIENTED_EDGE('',*,*,#1645,.F.);
#2513=ORIENTED_EDGE('',*,*,#1646,.T.);
#2514=ORIENTED_EDGE('',*,*,#1642,.T.);
#2515=ORIENTED_EDGE('',*,*,#1646,.F.);
#2516=ORIENTED_EDGE('',*,*,#1647,.T.);
#2517=ORIENTED_EDGE('',*,*,#1644,.T.);
#2518=ORIENTED_EDGE('',*,*,#1645,.T.);
#2519=ORIENTED_EDGE('',*,*,#1647,.F.);
#2520=ORIENTED_EDGE('',*,*,#1648,.F.);
#2521=ORIENTED_EDGE('',*,*,#1649,.F.);
#2522=ORIENTED_EDGE('',*,*,#1650,.F.);
#2523=ORIENTED_EDGE('',*,*,#1651,.F.);
#2524=ORIENTED_EDGE('',*,*,#1652,.T.);
#2525=ORIENTED_EDGE('',*,*,#1648,.T.);
#2526=ORIENTED_EDGE('',*,*,#1649,.T.);
#2527=ORIENTED_EDGE('',*,*,#1652,.F.);
#2528=ORIENTED_EDGE('',*,*,#1653,.F.);
#2529=ORIENTED_EDGE('',*,*,#1650,.T.);
#2530=ORIENTED_EDGE('',*,*,#1651,.T.);
#2531=ORIENTED_EDGE('',*,*,#1653,.T.);
#2532=ORIENTED_EDGE('',*,*,#1654,.F.);
#2533=ORIENTED_EDGE('',*,*,#1655,.F.);
#2534=ORIENTED_EDGE('',*,*,#1639,.F.);
#2535=ORIENTED_EDGE('',*,*,#1656,.T.);
#2536=ORIENTED_EDGE('',*,*,#1654,.T.);
#2537=ORIENTED_EDGE('',*,*,#1655,.T.);
#2538=ORIENTED_EDGE('',*,*,#1656,.F.);
#2539=ORIENTED_EDGE('',*,*,#1657,.T.);
#2540=ORIENTED_EDGE('',*,*,#1658,.T.);
#2541=ORIENTED_EDGE('',*,*,#1659,.F.);
#2542=ORIENTED_EDGE('',*,*,#1658,.F.);
#2543=ORIENTED_EDGE('',*,*,#1659,.T.);
#2544=ORIENTED_EDGE('',*,*,#1657,.F.);
#2545=ORIENTED_EDGE('',*,*,#1660,.F.);
#2546=ORIENTED_EDGE('',*,*,#1661,.F.);
#2547=ORIENTED_EDGE('',*,*,#1662,.F.);
#2548=ORIENTED_EDGE('',*,*,#1663,.F.);
#2549=ORIENTED_EDGE('',*,*,#1662,.T.);
#2550=ORIENTED_EDGE('',*,*,#1664,.F.);
#2551=ORIENTED_EDGE('',*,*,#1665,.T.);
#2552=ORIENTED_EDGE('',*,*,#1666,.F.);
#2553=ORIENTED_EDGE('',*,*,#1667,.F.);
#2554=ORIENTED_EDGE('',*,*,#1668,.T.);
#2555=ORIENTED_EDGE('',*,*,#1669,.T.);
#2556=ORIENTED_EDGE('',*,*,#1670,.T.);
#2557=ORIENTED_EDGE('',*,*,#1671,.T.);
#2558=ORIENTED_EDGE('',*,*,#1664,.T.);
#2559=ORIENTED_EDGE('',*,*,#1661,.T.);
#2560=ORIENTED_EDGE('',*,*,#1672,.T.);
#2561=ORIENTED_EDGE('',*,*,#1673,.T.);
#2562=ORIENTED_EDGE('',*,*,#1668,.F.);
#2563=ORIENTED_EDGE('',*,*,#1660,.T.);
#2564=ORIENTED_EDGE('',*,*,#1674,.F.);
#2565=ORIENTED_EDGE('',*,*,#1675,.F.);
#2566=ORIENTED_EDGE('',*,*,#1672,.F.);
#2567=ORIENTED_EDGE('',*,*,#1675,.T.);
#2568=ORIENTED_EDGE('',*,*,#1676,.F.);
#2569=ORIENTED_EDGE('',*,*,#1677,.F.);
#2570=ORIENTED_EDGE('',*,*,#1678,.F.);
#2571=ORIENTED_EDGE('',*,*,#1669,.F.);
#2572=ORIENTED_EDGE('',*,*,#1673,.F.);
#2573=ORIENTED_EDGE('',*,*,#1678,.T.);
#2574=ORIENTED_EDGE('',*,*,#1679,.F.);
#2575=ORIENTED_EDGE('',*,*,#1680,.F.);
#2576=ORIENTED_EDGE('',*,*,#1670,.F.);
#2577=ORIENTED_EDGE('',*,*,#1680,.T.);
#2578=ORIENTED_EDGE('',*,*,#1681,.F.);
#2579=ORIENTED_EDGE('',*,*,#1665,.F.);
#2580=ORIENTED_EDGE('',*,*,#1671,.F.);
#2581=ORIENTED_EDGE('',*,*,#1682,.F.);
#2582=ORIENTED_EDGE('',*,*,#1683,.T.);
#2583=ORIENTED_EDGE('',*,*,#1663,.T.);
#2584=ORIENTED_EDGE('',*,*,#1666,.T.);
#2585=ORIENTED_EDGE('',*,*,#1681,.T.);
#2586=ORIENTED_EDGE('',*,*,#1679,.T.);
#2587=ORIENTED_EDGE('',*,*,#1677,.T.);
#2588=ORIENTED_EDGE('',*,*,#1684,.T.);
#2589=ORIENTED_EDGE('',*,*,#1682,.T.);
#2590=ORIENTED_EDGE('',*,*,#1684,.F.);
#2591=ORIENTED_EDGE('',*,*,#1676,.T.);
#2592=ORIENTED_EDGE('',*,*,#1674,.T.);
#2593=ORIENTED_EDGE('',*,*,#1667,.T.);
#2594=ORIENTED_EDGE('',*,*,#1685,.F.);
#2595=ORIENTED_EDGE('',*,*,#1685,.T.);
#2596=ORIENTED_EDGE('',*,*,#1686,.T.);
#2597=ORIENTED_EDGE('',*,*,#1683,.F.);
#2598=ORIENTED_EDGE('',*,*,#1686,.F.);
#2599=CYLINDRICAL_SURFACE('',#2870,2.4505);
#2600=CYLINDRICAL_SURFACE('',#2873,1.99475);
#2601=CYLINDRICAL_SURFACE('',#2876,4.);
#2602=CYLINDRICAL_SURFACE('',#2879,4.5);
#2603=CYLINDRICAL_SURFACE('',#2884,0.25);
#2604=CYLINDRICAL_SURFACE('',#2886,0.25);
#2605=CYLINDRICAL_SURFACE('',#2888,0.25);
#2606=CYLINDRICAL_SURFACE('',#2890,0.25);
#2607=CYLINDRICAL_SURFACE('',#2892,0.25);
#2608=CYLINDRICAL_SURFACE('',#2894,0.25);
#2609=CYLINDRICAL_SURFACE('',#2896,0.25);
#2610=CYLINDRICAL_SURFACE('',#2898,0.25);
#2611=CYLINDRICAL_SURFACE('',#2900,0.25);
#2612=CYLINDRICAL_SURFACE('',#2902,0.25);
#2613=CYLINDRICAL_SURFACE('',#2904,0.25);
#2614=CYLINDRICAL_SURFACE('',#2906,0.25);
#2615=CYLINDRICAL_SURFACE('',#2908,0.25);
#2616=CYLINDRICAL_SURFACE('',#2910,0.25);
#2617=CYLINDRICAL_SURFACE('',#2912,0.25);
#2618=CYLINDRICAL_SURFACE('',#2914,0.25);
#2619=CYLINDRICAL_SURFACE('',#2916,0.25);
#2620=CYLINDRICAL_SURFACE('',#2918,0.25);
#2621=CYLINDRICAL_SURFACE('',#2920,0.25);
#2622=CYLINDRICAL_SURFACE('',#2922,0.25);
#2623=CYLINDRICAL_SURFACE('',#2924,0.25);
#2624=CYLINDRICAL_SURFACE('',#2926,0.25);
#2625=CYLINDRICAL_SURFACE('',#2928,0.25);
#2626=CYLINDRICAL_SURFACE('',#2930,0.25);
#2627=CYLINDRICAL_SURFACE('',#2932,0.25);
#2628=CYLINDRICAL_SURFACE('',#2934,0.25);
#2629=CYLINDRICAL_SURFACE('',#2936,0.25);
#2630=CYLINDRICAL_SURFACE('',#2938,0.25);
#2631=CYLINDRICAL_SURFACE('',#2940,0.25);
#2632=CYLINDRICAL_SURFACE('',#2942,0.25);
#2633=CYLINDRICAL_SURFACE('',#2944,0.25);
#2634=CYLINDRICAL_SURFACE('',#2946,0.25);
#2635=CYLINDRICAL_SURFACE('',#2948,0.25);
#2636=CYLINDRICAL_SURFACE('',#2950,0.25);
#2637=CYLINDRICAL_SURFACE('',#2952,0.25);
#2638=CYLINDRICAL_SURFACE('',#2954,0.25);
#2639=CYLINDRICAL_SURFACE('',#2956,0.25);
#2640=CYLINDRICAL_SURFACE('',#2958,0.25);
#2641=CYLINDRICAL_SURFACE('',#2960,0.25);
#2642=CYLINDRICAL_SURFACE('',#3004,5.5);
#2643=CYLINDRICAL_SURFACE('',#3006,5.5);
#2644=CYLINDRICAL_SURFACE('',#3008,5.5);
#2645=CYLINDRICAL_SURFACE('',#3010,5.5);
#2646=CYLINDRICAL_SURFACE('',#3012,5.5);
#2647=CYLINDRICAL_SURFACE('',#3014,5.5);
#2648=CYLINDRICAL_SURFACE('',#3016,5.5);
#2649=CYLINDRICAL_SURFACE('',#3018,5.5);
#2650=CYLINDRICAL_SURFACE('',#3020,5.5);
#2651=CYLINDRICAL_SURFACE('',#3022,5.5);
#2652=CYLINDRICAL_SURFACE('',#3024,5.5);
#2653=CYLINDRICAL_SURFACE('',#3026,5.5);
#2654=CYLINDRICAL_SURFACE('',#3028,5.5);
#2655=CYLINDRICAL_SURFACE('',#3030,5.5);
#2656=CYLINDRICAL_SURFACE('',#3032,5.5);
#2657=CYLINDRICAL_SURFACE('',#3034,5.5);
#2658=CYLINDRICAL_SURFACE('',#3036,5.5);
#2659=CYLINDRICAL_SURFACE('',#3038,5.5);
#2660=CYLINDRICAL_SURFACE('',#3040,5.5);
#2661=CYLINDRICAL_SURFACE('',#3042,5.5);
#2662=CYLINDRICAL_SURFACE('',#3044,5.5);
#2663=CYLINDRICAL_SURFACE('',#3046,5.5);
#2664=CYLINDRICAL_SURFACE('',#3048,5.5);
#2665=CYLINDRICAL_SURFACE('',#3050,5.5);
#2666=CYLINDRICAL_SURFACE('',#3052,5.5);
#2667=CYLINDRICAL_SURFACE('',#3054,5.5);
#2668=CYLINDRICAL_SURFACE('',#3056,5.5);
#2669=CYLINDRICAL_SURFACE('',#3058,5.5);
#2670=CYLINDRICAL_SURFACE('',#3060,5.5);
#2671=CYLINDRICAL_SURFACE('',#3062,5.5);
#2672=CYLINDRICAL_SURFACE('',#3064,5.5);
#2673=CYLINDRICAL_SURFACE('',#3066,5.5);
#2674=CYLINDRICAL_SURFACE('',#3068,5.5);
#2675=CYLINDRICAL_SURFACE('',#3070,5.5);
#2676=CYLINDRICAL_SURFACE('',#3072,5.5);
#2677=CYLINDRICAL_SURFACE('',#3074,5.5);
#2678=CYLINDRICAL_SURFACE('',#3076,5.5);
#2679=CYLINDRICAL_SURFACE('',#3078,5.5);
#2680=CYLINDRICAL_SURFACE('',#3080,5.5);
#2681=CYLINDRICAL_SURFACE('',#3085,0.25);
#2682=CYLINDRICAL_SURFACE('',#3086,5.5);
#2683=CYLINDRICAL_SURFACE('',#3102,2.5);
#2684=CYLINDRICAL_SURFACE('',#3120,2.5);
#2685=CYLINDRICAL_SURFACE('',#3143,1.666);
#2686=ADVANCED_FACE('',(#299),#2599,.T.);
#2687=ADVANCED_FACE('',(#300),#2600,.T.);
#2688=ADVANCED_FACE('',(#301),#2601,.F.);
#2689=ADVANCED_FACE('',(#302),#2602,.T.);
#2690=ADVANCED_FACE('',(#303,#87),#91,.T.);
#2691=ADVANCED_FACE('',(#304),#84,.F.);
#2692=ADVANCED_FACE('',(#305),#85,.F.);
#2693=ADVANCED_FACE('',(#306),#2603,.F.);
#2694=ADVANCED_FACE('',(#307),#2604,.F.);
#2695=ADVANCED_FACE('',(#308),#2605,.F.);
#2696=ADVANCED_FACE('',(#309),#2606,.F.);
#2697=ADVANCED_FACE('',(#310),#2607,.F.);
#2698=ADVANCED_FACE('',(#311),#2608,.F.);
#2699=ADVANCED_FACE('',(#312),#2609,.F.);
#2700=ADVANCED_FACE('',(#313),#2610,.F.);
#2701=ADVANCED_FACE('',(#314),#2611,.F.);
#2702=ADVANCED_FACE('',(#315),#2612,.F.);
#2703=ADVANCED_FACE('',(#316),#2613,.F.);
#2704=ADVANCED_FACE('',(#317),#2614,.F.);
#2705=ADVANCED_FACE('',(#318),#2615,.F.);
#2706=ADVANCED_FACE('',(#319),#2616,.F.);
#2707=ADVANCED_FACE('',(#320),#2617,.F.);
#2708=ADVANCED_FACE('',(#321),#2618,.F.);
#2709=ADVANCED_FACE('',(#322),#2619,.F.);
#2710=ADVANCED_FACE('',(#323),#2620,.F.);
#2711=ADVANCED_FACE('',(#324),#2621,.F.);
#2712=ADVANCED_FACE('',(#325),#2622,.F.);
#2713=ADVANCED_FACE('',(#326),#2623,.F.);
#2714=ADVANCED_FACE('',(#327),#2624,.F.);
#2715=ADVANCED_FACE('',(#328),#2625,.F.);
#2716=ADVANCED_FACE('',(#329),#2626,.F.);
#2717=ADVANCED_FACE('',(#330),#2627,.F.);
#2718=ADVANCED_FACE('',(#331),#2628,.F.);
#2719=ADVANCED_FACE('',(#332),#2629,.F.);
#2720=ADVANCED_FACE('',(#333),#2630,.F.);
#2721=ADVANCED_FACE('',(#334),#2631,.F.);
#2722=ADVANCED_FACE('',(#335),#2632,.F.);
#2723=ADVANCED_FACE('',(#336),#2633,.F.);
#2724=ADVANCED_FACE('',(#337),#2634,.F.);
#2725=ADVANCED_FACE('',(#338),#2635,.F.);
#2726=ADVANCED_FACE('',(#339),#2636,.F.);
#2727=ADVANCED_FACE('',(#340),#2637,.F.);
#2728=ADVANCED_FACE('',(#341),#2638,.F.);
#2729=ADVANCED_FACE('',(#342),#2639,.F.);
#2730=ADVANCED_FACE('',(#343),#2640,.F.);
#2731=ADVANCED_FACE('',(#344),#2641,.F.);
#2732=ADVANCED_FACE('',(#345),#92,.F.);
#2733=ADVANCED_FACE('',(#346),#2642,.T.);
#2734=ADVANCED_FACE('',(#347),#2643,.T.);
#2735=ADVANCED_FACE('',(#348),#2644,.T.);
#2736=ADVANCED_FACE('',(#349),#2645,.T.);
#2737=ADVANCED_FACE('',(#350),#2646,.T.);
#2738=ADVANCED_FACE('',(#351),#2647,.T.);
#2739=ADVANCED_FACE('',(#352),#2648,.T.);
#2740=ADVANCED_FACE('',(#353),#2649,.T.);
#2741=ADVANCED_FACE('',(#354),#2650,.T.);
#2742=ADVANCED_FACE('',(#355),#2651,.T.);
#2743=ADVANCED_FACE('',(#356),#2652,.T.);
#2744=ADVANCED_FACE('',(#357),#2653,.T.);
#2745=ADVANCED_FACE('',(#358),#2654,.T.);
#2746=ADVANCED_FACE('',(#359),#2655,.T.);
#2747=ADVANCED_FACE('',(#360),#2656,.T.);
#2748=ADVANCED_FACE('',(#361),#2657,.T.);
#2749=ADVANCED_FACE('',(#362),#2658,.T.);
#2750=ADVANCED_FACE('',(#363),#2659,.T.);
#2751=ADVANCED_FACE('',(#364),#2660,.T.);
#2752=ADVANCED_FACE('',(#365),#2661,.T.);
#2753=ADVANCED_FACE('',(#366),#2662,.T.);
#2754=ADVANCED_FACE('',(#367),#2663,.T.);
#2755=ADVANCED_FACE('',(#368),#2664,.T.);
#2756=ADVANCED_FACE('',(#369),#2665,.T.);
#2757=ADVANCED_FACE('',(#370),#2666,.T.);
#2758=ADVANCED_FACE('',(#371),#2667,.T.);
#2759=ADVANCED_FACE('',(#372),#2668,.T.);
#2760=ADVANCED_FACE('',(#373),#2669,.T.);
#2761=ADVANCED_FACE('',(#374),#2670,.T.);
#2762=ADVANCED_FACE('',(#375),#2671,.T.);
#2763=ADVANCED_FACE('',(#376),#2672,.T.);
#2764=ADVANCED_FACE('',(#377),#2673,.T.);
#2765=ADVANCED_FACE('',(#378),#2674,.T.);
#2766=ADVANCED_FACE('',(#379),#2675,.T.);
#2767=ADVANCED_FACE('',(#380),#2676,.T.);
#2768=ADVANCED_FACE('',(#381),#2677,.T.);
#2769=ADVANCED_FACE('',(#382),#2678,.T.);
#2770=ADVANCED_FACE('',(#383),#2679,.T.);
#2771=ADVANCED_FACE('',(#384),#2680,.T.);
#2772=ADVANCED_FACE('',(#385),#77,.T.);
#2773=ADVANCED_FACE('',(#386),#2681,.F.);
#2774=ADVANCED_FACE('',(#387),#2682,.T.);
#2775=ADVANCED_FACE('',(#388,#88),#93,.T.);
#2776=ADVANCED_FACE('',(#389),#94,.T.);
#2777=ADVANCED_FACE('',(#390),#51,.T.);
#2778=ADVANCED_FACE('',(#391),#78,.T.);
#2779=ADVANCED_FACE('',(#392),#52,.F.);
#2780=ADVANCED_FACE('',(#393),#79,.F.);
#2781=ADVANCED_FACE('',(#394),#47,.T.);
#2782=ADVANCED_FACE('',(#395),#2683,.F.);
#2783=ADVANCED_FACE('',(#396),#48,.T.);
#2784=ADVANCED_FACE('',(#397),#80,.T.);
#2785=ADVANCED_FACE('',(#398),#53,.T.);
#2786=ADVANCED_FACE('',(#399),#81,.T.);
#2787=ADVANCED_FACE('',(#400),#54,.F.);
#2788=ADVANCED_FACE('',(#401),#82,.F.);
#2789=ADVANCED_FACE('',(#402),#49,.T.);
#2790=ADVANCED_FACE('',(#403),#2684,.F.);
#2791=ADVANCED_FACE('',(#404),#50,.T.);
#2792=ADVANCED_FACE('',(#405),#83,.T.);
#2793=ADVANCED_FACE('',(#406),#86,.T.);
#2794=ADVANCED_FACE('',(#407),#95,.F.);
#2795=ADVANCED_FACE('',(#408),#96,.T.);
#2796=ADVANCED_FACE('',(#409),#97,.F.);
#2797=ADVANCED_FACE('',(#410),#98,.F.);
#2798=ADVANCED_FACE('',(#411),#55,.T.);
#2799=ADVANCED_FACE('',(#412),#99,.F.);
#2800=ADVANCED_FACE('',(#413),#100,.F.);
#2801=ADVANCED_FACE('',(#414),#101,.F.);
#2802=ADVANCED_FACE('',(#415),#102,.F.);
#2803=ADVANCED_FACE('',(#416,#89),#103,.T.);
#2804=ADVANCED_FACE('',(#417),#56,.T.);
#2805=ADVANCED_FACE('',(#418,#90),#104,.T.);
#2806=ADVANCED_FACE('',(#419),#2685,.F.);
#2807=CLOSED_SHELL('',(#2686,#2687,#2688,#2689,#2690,#2691,#2692,#2693,
#2694,#2695,#2696,#2697,#2698,#2699,#2700,#2701,#2702,#2703,#2704,#2705,
#2706,#2707,#2708,#2709,#2710,#2711,#2712,#2713,#2714,#2715,#2716,#2717,
#2718,#2719,#2720,#2721,#2722,#2723,#2724,#2725,#2726,#2727,#2728,#2729,
#2730,#2731,#2732,#2733,#2734,#2735,#2736,#2737,#2738,#2739,#2740,#2741,
#2742,#2743,#2744,#2745,#2746,#2747,#2748,#2749,#2750,#2751,#2752,#2753,
#2754,#2755,#2756,#2757,#2758,#2759,#2760,#2761,#2762,#2763,#2764,#2765,
#2766,#2767,#2768,#2769,#2770,#2771,#2772,#2773,#2774,#2775,#2776));
#2808=CLOSED_SHELL('',(#2777,#2778,#2779,#2780,#2781,#2782,#2783,#2784));
#2809=CLOSED_SHELL('',(#2785,#2786,#2787,#2788,#2789,#2790,#2791,#2792));
#2810=CLOSED_SHELL('',(#2793,#2794,#2795));
#2811=CLOSED_SHELL('',(#2796,#2797,#2798,#2799,#2800,#2801,#2802,#2803,
#2804,#2805,#2806));
#2812=DERIVED_UNIT_ELEMENT(#2822,1.);
#2813=DERIVED_UNIT_ELEMENT(#33476,-3.);
#2814=DERIVED_UNIT_ELEMENT(#2822,1.);
#2815=DERIVED_UNIT_ELEMENT(#33476,-3.);
#2816=DERIVED_UNIT_ELEMENT(#2822,1.);
#2817=DERIVED_UNIT_ELEMENT(#33476,-3.);
#2818=DERIVED_UNIT_ELEMENT(#2822,1.);
#2819=DERIVED_UNIT_ELEMENT(#33476,-3.);
#2820=DERIVED_UNIT_ELEMENT(#2822,1.);
#2821=DERIVED_UNIT_ELEMENT(#33476,-3.);
#2822=(
MASS_UNIT()
NAMED_UNIT(*)
SI_UNIT(.KILO.,.GRAM.)
);
#2823=DERIVED_UNIT((#2812,#2813));
#2824=DERIVED_UNIT((#2814,#2815));
#2825=DERIVED_UNIT((#2816,#2817));
#2826=DERIVED_UNIT((#2818,#2819));
#2827=DERIVED_UNIT((#2820,#2821));
#2828=MEASURE_REPRESENTATION_ITEM('density measure',
POSITIVE_RATIO_MEASURE(7850.),#2823);
#2829=MEASURE_REPRESENTATION_ITEM('density measure',
POSITIVE_RATIO_MEASURE(7850.),#2824);
#2830=MEASURE_REPRESENTATION_ITEM('density measure',
POSITIVE_RATIO_MEASURE(7850.),#2825);
#2831=MEASURE_REPRESENTATION_ITEM('density measure',
POSITIVE_RATIO_MEASURE(7850.),#2826);
#2832=MEASURE_REPRESENTATION_ITEM('density measure',
POSITIVE_RATIO_MEASURE(7750.),#2827);
#2833=PROPERTY_DEFINITION_REPRESENTATION(#2858,#2843);
#2834=PROPERTY_DEFINITION_REPRESENTATION(#2859,#2844);
#2835=PROPERTY_DEFINITION_REPRESENTATION(#2860,#2845);
#2836=PROPERTY_DEFINITION_REPRESENTATION(#2861,#2846);
#2837=PROPERTY_DEFINITION_REPRESENTATION(#2862,#2847);
#2838=PROPERTY_DEFINITION_REPRESENTATION(#2863,#2848);
#2839=PROPERTY_DEFINITION_REPRESENTATION(#2864,#2849);
#2840=PROPERTY_DEFINITION_REPRESENTATION(#2865,#2850);
#2841=PROPERTY_DEFINITION_REPRESENTATION(#2866,#2851);
#2842=PROPERTY_DEFINITION_REPRESENTATION(#2867,#2852);
#2843=REPRESENTATION('material name',(#2853),#33469);
#2844=REPRESENTATION('density',(#2828),#33469);
#2845=REPRESENTATION('material name',(#2854),#33470);
#2846=REPRESENTATION('density',(#2829),#33470);
#2847=REPRESENTATION('material name',(#2855),#33471);
#2848=REPRESENTATION('density',(#2830),#33471);
#2849=REPRESENTATION('material name',(#2856),#33472);
#2850=REPRESENTATION('density',(#2831),#33472);
#2851=REPRESENTATION('material name',(#2857),#33473);
#2852=REPRESENTATION('density',(#2832),#33473);
#2853=DESCRIPTIVE_REPRESENTATION_ITEM('Steel','Steel');
#2854=DESCRIPTIVE_REPRESENTATION_ITEM('Steel','Steel');
#2855=DESCRIPTIVE_REPRESENTATION_ITEM('Steel','Steel');
#2856=DESCRIPTIVE_REPRESENTATION_ITEM('Steel','Steel');
#2857=DESCRIPTIVE_REPRESENTATION_ITEM('Steel Grade 2H, Plain',
'Steel Grade 2H, Plain');
#2858=PROPERTY_DEFINITION('material property','material name',#33504);
#2859=PROPERTY_DEFINITION('material property','density of part',#33504);
#2860=PROPERTY_DEFINITION('material property','material name',#33505);
#2861=PROPERTY_DEFINITION('material property','density of part',#33505);
#2862=PROPERTY_DEFINITION('material property','material name',#33506);
#2863=PROPERTY_DEFINITION('material property','density of part',#33506);
#2864=PROPERTY_DEFINITION('material property','material name',#33507);
#2865=PROPERTY_DEFINITION('material property','density of part',#33507);
#2866=PROPERTY_DEFINITION('material property','material name',#33508);
#2867=PROPERTY_DEFINITION('material property','density of part',#33508);
#2868=AXIS2_PLACEMENT_3D('',#3808,#3149,#3150);
#2869=AXIS2_PLACEMENT_3D('',#3809,#3151,#3152);
#2870=AXIS2_PLACEMENT_3D('',#3810,#3153,#3154);
#2871=AXIS2_PLACEMENT_3D('',#3820,#3155,#3156);
#2872=AXIS2_PLACEMENT_3D('',#7359,#3157,#3158);
#2873=AXIS2_PLACEMENT_3D('',#10889,#3159,#3160);
#2874=AXIS2_PLACEMENT_3D('',#11491,#3161,#3162);
#2875=AXIS2_PLACEMENT_3D('',#19798,#3163,#3164);
#2876=AXIS2_PLACEMENT_3D('',#27454,#3165,#3166);
#2877=AXIS2_PLACEMENT_3D('',#27456,#3167,#3168);
#2878=AXIS2_PLACEMENT_3D('',#27459,#3170,#3171);
#2879=AXIS2_PLACEMENT_3D('',#27460,#3172,#3173);
#2880=AXIS2_PLACEMENT_3D('',#27462,#3174,#3175);
#2881=AXIS2_PLACEMENT_3D('',#27466,#3177,#3178);
#2882=AXIS2_PLACEMENT_3D('',#27467,#3179,#3180);
#2883=AXIS2_PLACEMENT_3D('',#27468,#3181,#3182);
#2884=AXIS2_PLACEMENT_3D('',#29757,#3183,#3184);
#2885=AXIS2_PLACEMENT_3D('',#29797,#3186,#3187);
#2886=AXIS2_PLACEMENT_3D('',#29799,#3189,#3190);
#2887=AXIS2_PLACEMENT_3D('',#29839,#3192,#3193);
#2888=AXIS2_PLACEMENT_3D('',#29841,#3195,#3196);
#2889=AXIS2_PLACEMENT_3D('',#29881,#3198,#3199);
#2890=AXIS2_PLACEMENT_3D('',#29883,#3201,#3202);
#2891=AXIS2_PLACEMENT_3D('',#29923,#3204,#3205);
#2892=AXIS2_PLACEMENT_3D('',#29925,#3207,#3208);
#2893=AXIS2_PLACEMENT_3D('',#29965,#3210,#3211);
#2894=AXIS2_PLACEMENT_3D('',#29967,#3213,#3214);
#2895=AXIS2_PLACEMENT_3D('',#30007,#3216,#3217);
#2896=AXIS2_PLACEMENT_3D('',#30009,#3219,#3220);
#2897=AXIS2_PLACEMENT_3D('',#30049,#3222,#3223);
#2898=AXIS2_PLACEMENT_3D('',#30051,#3225,#3226);
#2899=AXIS2_PLACEMENT_3D('',#30091,#3228,#3229);
#2900=AXIS2_PLACEMENT_3D('',#30093,#3231,#3232);
#2901=AXIS2_PLACEMENT_3D('',#30133,#3234,#3235);
#2902=AXIS2_PLACEMENT_3D('',#30135,#3237,#3238);
#2903=AXIS2_PLACEMENT_3D('',#30161,#3240,#3241);
#2904=AXIS2_PLACEMENT_3D('',#30182,#3243,#3244);
#2905=AXIS2_PLACEMENT_3D('',#30222,#3246,#3247);
#2906=AXIS2_PLACEMENT_3D('',#30224,#3249,#3250);
#2907=AXIS2_PLACEMENT_3D('',#30264,#3252,#3253);
#2908=AXIS2_PLACEMENT_3D('',#30266,#3255,#3256);
#2909=AXIS2_PLACEMENT_3D('',#30306,#3258,#3259);
#2910=AXIS2_PLACEMENT_3D('',#30308,#3261,#3262);
#2911=AXIS2_PLACEMENT_3D('',#30348,#3264,#3265);
#2912=AXIS2_PLACEMENT_3D('',#30350,#3267,#3268);
#2913=AXIS2_PLACEMENT_3D('',#30390,#3270,#3271);
#2914=AXIS2_PLACEMENT_3D('',#30392,#3273,#3274);
#2915=AXIS2_PLACEMENT_3D('',#30432,#3276,#3277);
#2916=AXIS2_PLACEMENT_3D('',#30434,#3279,#3280);
#2917=AXIS2_PLACEMENT_3D('',#30474,#3282,#3283);
#2918=AXIS2_PLACEMENT_3D('',#30476,#3285,#3286);
#2919=AXIS2_PLACEMENT_3D('',#30516,#3288,#3289);
#2920=AXIS2_PLACEMENT_3D('',#30518,#3291,#3292);
#2921=AXIS2_PLACEMENT_3D('',#30558,#3294,#3295);
#2922=AXIS2_PLACEMENT_3D('',#30560,#3297,#3298);
#2923=AXIS2_PLACEMENT_3D('',#30600,#3300,#3301);
#2924=AXIS2_PLACEMENT_3D('',#30602,#3303,#3304);
#2925=AXIS2_PLACEMENT_3D('',#30642,#3306,#3307);
#2926=AXIS2_PLACEMENT_3D('',#30644,#3309,#3310);
#2927=AXIS2_PLACEMENT_3D('',#30684,#3312,#3313);
#2928=AXIS2_PLACEMENT_3D('',#30686,#3315,#3316);
#2929=AXIS2_PLACEMENT_3D('',#30726,#3318,#3319);
#2930=AXIS2_PLACEMENT_3D('',#30728,#3321,#3322);
#2931=AXIS2_PLACEMENT_3D('',#30768,#3324,#3325);
#2932=AXIS2_PLACEMENT_3D('',#30770,#3327,#3328);
#2933=AXIS2_PLACEMENT_3D('',#30810,#3330,#3331);
#2934=AXIS2_PLACEMENT_3D('',#30812,#3333,#3334);
#2935=AXIS2_PLACEMENT_3D('',#30852,#3336,#3337);
#2936=AXIS2_PLACEMENT_3D('',#30854,#3339,#3340);
#2937=AXIS2_PLACEMENT_3D('',#30894,#3342,#3343);
#2938=AXIS2_PLACEMENT_3D('',#30896,#3345,#3346);
#2939=AXIS2_PLACEMENT_3D('',#30936,#3348,#3349);
#2940=AXIS2_PLACEMENT_3D('',#30938,#3351,#3352);
#2941=AXIS2_PLACEMENT_3D('',#30978,#3354,#3355);
#2942=AXIS2_PLACEMENT_3D('',#30980,#3357,#3358);
#2943=AXIS2_PLACEMENT_3D('',#31020,#3360,#3361);
#2944=AXIS2_PLACEMENT_3D('',#31022,#3363,#3364);
#2945=AXIS2_PLACEMENT_3D('',#31062,#3366,#3367);
#2946=AXIS2_PLACEMENT_3D('',#31064,#3369,#3370);
#2947=AXIS2_PLACEMENT_3D('',#31104,#3372,#3373);
#2948=AXIS2_PLACEMENT_3D('',#31106,#3375,#3376);
#2949=AXIS2_PLACEMENT_3D('',#31146,#3378,#3379);
#2950=AXIS2_PLACEMENT_3D('',#31148,#3381,#3382);
#2951=AXIS2_PLACEMENT_3D('',#31188,#3384,#3385);
#2952=AXIS2_PLACEMENT_3D('',#31190,#3387,#3388);
#2953=AXIS2_PLACEMENT_3D('',#31230,#3390,#3391);
#2954=AXIS2_PLACEMENT_3D('',#31232,#3393,#3394);
#2955=AXIS2_PLACEMENT_3D('',#31272,#3396,#3397);
#2956=AXIS2_PLACEMENT_3D('',#31274,#3399,#3400);
#2957=AXIS2_PLACEMENT_3D('',#31314,#3402,#3403);
#2958=AXIS2_PLACEMENT_3D('',#31316,#3405,#3406);
#2959=AXIS2_PLACEMENT_3D('',#31356,#3408,#3409);
#2960=AXIS2_PLACEMENT_3D('',#31358,#3411,#3412);
#2961=AXIS2_PLACEMENT_3D('',#31398,#3414,#3415);
#2962=AXIS2_PLACEMENT_3D('',#31400,#3417,#3418);
#2963=AXIS2_PLACEMENT_3D('',#31401,#3419,#3420);
#2964=AXIS2_PLACEMENT_3D('',#31402,#3421,#3422);
#2965=AXIS2_PLACEMENT_3D('',#31403,#3423,#3424);
#2966=AXIS2_PLACEMENT_3D('',#31404,#3425,#3426);
#2967=AXIS2_PLACEMENT_3D('',#31405,#3427,#3428);
#2968=AXIS2_PLACEMENT_3D('',#31406,#3429,#3430);
#2969=AXIS2_PLACEMENT_3D('',#31407,#3431,#3432);
#2970=AXIS2_PLACEMENT_3D('',#31408,#3433,#3434);
#2971=AXIS2_PLACEMENT_3D('',#31409,#3435,#3436);
#2972=AXIS2_PLACEMENT_3D('',#31410,#3437,#3438);
#2973=AXIS2_PLACEMENT_3D('',#31411,#3439,#3440);
#2974=AXIS2_PLACEMENT_3D('',#31412,#3441,#3442);
#2975=AXIS2_PLACEMENT_3D('',#31413,#3443,#3444);
#2976=AXIS2_PLACEMENT_3D('',#31414,#3445,#3446);
#2977=AXIS2_PLACEMENT_3D('',#31415,#3447,#3448);
#2978=AXIS2_PLACEMENT_3D('',#31416,#3449,#3450);
#2979=AXIS2_PLACEMENT_3D('',#31417,#3451,#3452);
#2980=AXIS2_PLACEMENT_3D('',#31418,#3453,#3454);
#2981=AXIS2_PLACEMENT_3D('',#31419,#3455,#3456);
#2982=AXIS2_PLACEMENT_3D('',#31420,#3457,#3458);
#2983=AXIS2_PLACEMENT_3D('',#31421,#3459,#3460);
#2984=AXIS2_PLACEMENT_3D('',#31422,#3461,#3462);
#2985=AXIS2_PLACEMENT_3D('',#31423,#3463,#3464);
#2986=AXIS2_PLACEMENT_3D('',#31424,#3465,#3466);
#2987=AXIS2_PLACEMENT_3D('',#31425,#3467,#3468);
#2988=AXIS2_PLACEMENT_3D('',#31426,#3469,#3470);
#2989=AXIS2_PLACEMENT_3D('',#31427,#3471,#3472);
#2990=AXIS2_PLACEMENT_3D('',#31428,#3473,#3474);
#2991=AXIS2_PLACEMENT_3D('',#31429,#3475,#3476);
#2992=AXIS2_PLACEMENT_3D('',#31430,#3477,#3478);
#2993=AXIS2_PLACEMENT_3D('',#31431,#3479,#3480);
#2994=AXIS2_PLACEMENT_3D('',#31432,#3481,#3482);
#2995=AXIS2_PLACEMENT_3D('',#31433,#3483,#3484);
#2996=AXIS2_PLACEMENT_3D('',#31434,#3485,#3486);
#2997=AXIS2_PLACEMENT_3D('',#31435,#3487,#3488);
#2998=AXIS2_PLACEMENT_3D('',#31436,#3489,#3490);
#2999=AXIS2_PLACEMENT_3D('',#31437,#3491,#3492);
#3000=AXIS2_PLACEMENT_3D('',#31438,#3493,#3494);
#3001=AXIS2_PLACEMENT_3D('',#31440,#3495,#3496);
#3002=AXIS2_PLACEMENT_3D('',#31442,#3497,#3498);
#3003=AXIS2_PLACEMENT_3D('',#31443,#3499,#3500);
#3004=AXIS2_PLACEMENT_3D('',#31444,#3501,#3502);
#3005=AXIS2_PLACEMENT_3D('',#31446,#3503,#3504);
#3006=AXIS2_PLACEMENT_3D('',#31448,#3506,#3507);
#3007=AXIS2_PLACEMENT_3D('',#31449,#3508,#3509);
#3008=AXIS2_PLACEMENT_3D('',#31450,#3510,#3511);
#3009=AXIS2_PLACEMENT_3D('',#31451,#3512,#3513);
#3010=AXIS2_PLACEMENT_3D('',#31452,#3514,#3515);
#3011=AXIS2_PLACEMENT_3D('',#31453,#3516,#3517);
#3012=AXIS2_PLACEMENT_3D('',#31454,#3518,#3519);
#3013=AXIS2_PLACEMENT_3D('',#31455,#3520,#3521);
#3014=AXIS2_PLACEMENT_3D('',#31456,#3522,#3523);
#3015=AXIS2_PLACEMENT_3D('',#31457,#3524,#3525);
#3016=AXIS2_PLACEMENT_3D('',#31458,#3526,#3527);
#3017=AXIS2_PLACEMENT_3D('',#31459,#3528,#3529);
#3018=AXIS2_PLACEMENT_3D('',#31460,#3530,#3531);
#3019=AXIS2_PLACEMENT_3D('',#31461,#3532,#3533);
#3020=AXIS2_PLACEMENT_3D('',#31462,#3534,#3535);
#3021=AXIS2_PLACEMENT_3D('',#31463,#3536,#3537);
#3022=AXIS2_PLACEMENT_3D('',#31464,#3538,#3539);
#3023=AXIS2_PLACEMENT_3D('',#31465,#3540,#3541);
#3024=AXIS2_PLACEMENT_3D('',#31466,#3542,#3543);
#3025=AXIS2_PLACEMENT_3D('',#31467,#3544,#3545);
#3026=AXIS2_PLACEMENT_3D('',#31468,#3546,#3547);
#3027=AXIS2_PLACEMENT_3D('',#31469,#3548,#3549);
#3028=AXIS2_PLACEMENT_3D('',#31470,#3550,#3551);
#3029=AXIS2_PLACEMENT_3D('',#31471,#3552,#3553);
#3030=AXIS2_PLACEMENT_3D('',#31472,#3554,#3555);
#3031=AXIS2_PLACEMENT_3D('',#31473,#3556,#3557);
#3032=AXIS2_PLACEMENT_3D('',#31474,#3558,#3559);
#3033=AXIS2_PLACEMENT_3D('',#31475,#3560,#3561);
#3034=AXIS2_PLACEMENT_3D('',#31476,#3562,#3563);
#3035=AXIS2_PLACEMENT_3D('',#31477,#3564,#3565);
#3036=AXIS2_PLACEMENT_3D('',#31478,#3566,#3567);
#3037=AXIS2_PLACEMENT_3D('',#31479,#3568,#3569);
#3038=AXIS2_PLACEMENT_3D('',#31480,#3570,#3571);
#3039=AXIS2_PLACEMENT_3D('',#31481,#3572,#3573);
#3040=AXIS2_PLACEMENT_3D('',#31482,#3574,#3575);
#3041=AXIS2_PLACEMENT_3D('',#31483,#3576,#3577);
#3042=AXIS2_PLACEMENT_3D('',#31484,#3578,#3579);
#3043=AXIS2_PLACEMENT_3D('',#31485,#3580,#3581);
#3044=AXIS2_PLACEMENT_3D('',#31486,#3582,#3583);
#3045=AXIS2_PLACEMENT_3D('',#31487,#3584,#3585);
#3046=AXIS2_PLACEMENT_3D('',#31488,#3586,#3587);
#3047=AXIS2_PLACEMENT_3D('',#31489,#3588,#3589);
#3048=AXIS2_PLACEMENT_3D('',#31490,#3590,#3591);
#3049=AXIS2_PLACEMENT_3D('',#31491,#3592,#3593);
#3050=AXIS2_PLACEMENT_3D('',#31492,#3594,#3595);
#3051=AXIS2_PLACEMENT_3D('',#31493,#3596,#3597);
#3052=AXIS2_PLACEMENT_3D('',#31494,#3598,#3599);
#3053=AXIS2_PLACEMENT_3D('',#31495,#3600,#3601);
#3054=AXIS2_PLACEMENT_3D('',#31496,#3602,#3603);
#3055=AXIS2_PLACEMENT_3D('',#31497,#3604,#3605);
#3056=AXIS2_PLACEMENT_3D('',#31498,#3606,#3607);
#3057=AXIS2_PLACEMENT_3D('',#31499,#3608,#3609);
#3058=AXIS2_PLACEMENT_3D('',#31500,#3610,#3611);
#3059=AXIS2_PLACEMENT_3D('',#31501,#3612,#3613);
#3060=AXIS2_PLACEMENT_3D('',#31502,#3614,#3615);
#3061=AXIS2_PLACEMENT_3D('',#31503,#3616,#3617);
#3062=AXIS2_PLACEMENT_3D('',#31504,#3618,#3619);
#3063=AXIS2_PLACEMENT_3D('',#31505,#3620,#3621);
#3064=AXIS2_PLACEMENT_3D('',#31506,#3622,#3623);
#3065=AXIS2_PLACEMENT_3D('',#31507,#3624,#3625);
#3066=AXIS2_PLACEMENT_3D('',#31508,#3626,#3627);
#3067=AXIS2_PLACEMENT_3D('',#31509,#3628,#3629);
#3068=AXIS2_PLACEMENT_3D('',#31510,#3630,#3631);
#3069=AXIS2_PLACEMENT_3D('',#31511,#3632,#3633);
#3070=AXIS2_PLACEMENT_3D('',#31512,#3634,#3635);
#3071=AXIS2_PLACEMENT_3D('',#31513,#3636,#3637);
#3072=AXIS2_PLACEMENT_3D('',#31514,#3638,#3639);
#3073=AXIS2_PLACEMENT_3D('',#31515,#3640,#3641);
#3074=AXIS2_PLACEMENT_3D('',#31516,#3642,#3643);
#3075=AXIS2_PLACEMENT_3D('',#31517,#3644,#3645);
#3076=AXIS2_PLACEMENT_3D('',#31518,#3646,#3647);
#3077=AXIS2_PLACEMENT_3D('',#31519,#3648,#3649);
#3078=AXIS2_PLACEMENT_3D('',#31520,#3650,#3651);
#3079=AXIS2_PLACEMENT_3D('',#31521,#3652,#3653);
#3080=AXIS2_PLACEMENT_3D('',#31522,#3654,#3655);
#3081=AXIS2_PLACEMENT_3D('',#31523,#3656,#3657);
#3082=AXIS2_PLACEMENT_3D('',#31524,#3658,#3659);
#3083=AXIS2_PLACEMENT_3D('',#31525,#3660,#3661);
#3084=AXIS2_PLACEMENT_3D('',#31527,#3662,#3663);
#3085=AXIS2_PLACEMENT_3D('',#31562,#3664,#3665);
#3086=AXIS2_PLACEMENT_3D('',#31564,#3667,#3668);
#3087=AXIS2_PLACEMENT_3D('',#31565,#3669,#3670);
#3088=AXIS2_PLACEMENT_3D('',#31566,#3671,#3672);
#3089=AXIS2_PLACEMENT_3D('',#31567,#3673,#3674);
#3090=AXIS2_PLACEMENT_3D('',#31568,#3675,#3676);
#3091=AXIS2_PLACEMENT_3D('',#31570,#3677,#3678);
#3092=AXIS2_PLACEMENT_3D('',#31573,#3680,#3681);
#3093=AXIS2_PLACEMENT_3D('',#31574,#3682,#3683);
#3094=AXIS2_PLACEMENT_3D('',#31576,#3684,#3685);
#3095=AXIS2_PLACEMENT_3D('',#31577,#3686,#3687);
#3096=AXIS2_PLACEMENT_3D('',#31578,#3688,#3689);
#3097=AXIS2_PLACEMENT_3D('',#31580,#3690,#3691);
#3098=AXIS2_PLACEMENT_3D('',#31582,#3693,#3694);
#3099=AXIS2_PLACEMENT_3D('',#31585,#3695,#3696);
#3100=AXIS2_PLACEMENT_3D('',#31586,#3697,#3698);
#3101=AXIS2_PLACEMENT_3D('',#31587,#3699,#3700);
#3102=AXIS2_PLACEMENT_3D('',#31880,#3701,#3702);
#3103=AXIS2_PLACEMENT_3D('',#32056,#3704,#3705);
#3104=AXIS2_PLACEMENT_3D('',#32057,#3706,#3707);
#3105=AXIS2_PLACEMENT_3D('',#32058,#3708,#3709);
#3106=AXIS2_PLACEMENT_3D('',#32059,#3710,#3711);
#3107=AXIS2_PLACEMENT_3D('',#32060,#3712,#3713);
#3108=AXIS2_PLACEMENT_3D('',#32061,#3714,#3715);
#3109=AXIS2_PLACEMENT_3D('',#32063,#3716,#3717);
#3110=AXIS2_PLACEMENT_3D('',#32066,#3719,#3720);
#3111=AXIS2_PLACEMENT_3D('',#32067,#3721,#3722);
#3112=AXIS2_PLACEMENT_3D('',#32069,#3723,#3724);
#3113=AXIS2_PLACEMENT_3D('',#32070,#3725,#3726);
#3114=AXIS2_PLACEMENT_3D('',#32071,#3727,#3728);
#3115=AXIS2_PLACEMENT_3D('',#32073,#3729,#3730);
#3116=AXIS2_PLACEMENT_3D('',#32075,#3732,#3733);
#3117=AXIS2_PLACEMENT_3D('',#32078,#3734,#3735);
#3118=AXIS2_PLACEMENT_3D('',#32079,#3736,#3737);
#3119=AXIS2_PLACEMENT_3D('',#32080,#3738,#3739);
#3120=AXIS2_PLACEMENT_3D('',#32373,#3740,#3741);
#3121=AXIS2_PLACEMENT_3D('',#32549,#3743,#3744);
#3122=AXIS2_PLACEMENT_3D('',#32550,#3745,#3746);
#3123=AXIS2_PLACEMENT_3D('',#32551,#3747,#3748);
#3124=AXIS2_PLACEMENT_3D('',#32552,#3749,#3750);
#3125=AXIS2_PLACEMENT_3D('',#32553,#3751,#3752);
#3126=AXIS2_PLACEMENT_3D('',#33369,#3753,#3754);
#3127=AXIS2_PLACEMENT_3D('',#33370,#3755,#3756);
#3128=AXIS2_PLACEMENT_3D('',#33371,#3757,#3758);
#3129=AXIS2_PLACEMENT_3D('',#33372,#3759,#3760);
#3130=AXIS2_PLACEMENT_3D('',#33385,#3763,#3764);
#3131=AXIS2_PLACEMENT_3D('',#33395,#3766,#3767);
#3132=AXIS2_PLACEMENT_3D('',#33397,#3768,#3769);
#3133=AXIS2_PLACEMENT_3D('',#33418,#3771,#3772);
#3134=AXIS2_PLACEMENT_3D('',#33424,#3774,#3775);
#3135=AXIS2_PLACEMENT_3D('',#33434,#3777,#3778);
#3136=AXIS2_PLACEMENT_3D('',#33440,#3780,#3781);
#3137=AXIS2_PLACEMENT_3D('',#33444,#3782,#3783);
#3138=AXIS2_PLACEMENT_3D('',#33446,#3784,#3785);
#3139=AXIS2_PLACEMENT_3D('',#33448,#3786,#3787);
#3140=AXIS2_PLACEMENT_3D('',#33449,#3788,#3789);
#3141=AXIS2_PLACEMENT_3D('',#33451,#3791,#3792);
#3142=AXIS2_PLACEMENT_3D('',#33453,#3793,#3794);
#3143=AXIS2_PLACEMENT_3D('',#33454,#3795,#3796);
#3144=AXIS2_PLACEMENT_3D('',#33456,#3798,#3799);
#3145=AXIS2_PLACEMENT_3D('',#33457,#3800,#3801);
#3146=AXIS2_PLACEMENT_3D('',#33458,#3802,#3803);
#3147=AXIS2_PLACEMENT_3D('',#33459,#3804,#3805);
#3148=AXIS2_PLACEMENT_3D('',#33460,#3806,#3807);
#3149=DIRECTION('axis',(0.,0.,1.));
#3150=DIRECTION('refdir',(1.,0.,0.));
#3151=DIRECTION('axis',(0.,0.,1.));
#3152=DIRECTION('refdir',(1.,0.,0.));
#3153=DIRECTION('center_axis',(0.,0.,1.));
#3154=DIRECTION('ref_axis',(1.,0.,0.));
#3155=DIRECTION('center_axis',(0.,0.,-1.));
#3156=DIRECTION('ref_axis',(1.,0.,0.));
#3157=DIRECTION('center_axis',(0.,0.,-1.));
#3158=DIRECTION('ref_axis',(1.,0.,0.));
#3159=DIRECTION('center_axis',(0.,0.,1.));
#3160=DIRECTION('ref_axis',(1.,-3.42306004707827E-13,0.));
#3161=DIRECTION('center_axis',(0.,0.,-1.));
#3162=DIRECTION('ref_axis',(1.,-3.42306004707827E-13,0.));
#3163=DIRECTION('center_axis',(0.,0.,1.));
#3164=DIRECTION('ref_axis',(1.,-3.42306004707827E-13,0.));
#3165=DIRECTION('center_axis',(0.,0.,1.));
#3166=DIRECTION('ref_axis',(-1.,0.,0.));
#3167=DIRECTION('center_axis',(0.,0.,1.));
#3168=DIRECTION('ref_axis',(-1.,0.,0.));
#3169=DIRECTION('',(0.,0.,1.));
#3170=DIRECTION('center_axis',(0.,0.,-1.));
#3171=DIRECTION('ref_axis',(-1.,0.,0.));
#3172=DIRECTION('center_axis',(0.,0.,1.));
#3173=DIRECTION('ref_axis',(-1.,0.,0.));
#3174=DIRECTION('center_axis',(0.,0.,1.));
#3175=DIRECTION('ref_axis',(-1.,0.,0.));
#3176=DIRECTION('',(0.,0.,-1.));
#3177=DIRECTION('center_axis',(0.,0.,-1.));
#3178=DIRECTION('ref_axis',(1.,0.,0.));
#3179=DIRECTION('center_axis',(0.,0.,-1.));
#3180=DIRECTION('ref_axis',(1.,0.,0.));
#3181=DIRECTION('center_axis',(0.,0.,1.));
#3182=DIRECTION('ref_axis',(-1.,0.,0.));
#3183=DIRECTION('center_axis',(0.,0.,1.));
#3184=DIRECTION('ref_axis',(0.987688340595138,-0.156434465040231,0.));
#3185=DIRECTION('',(0.,0.,1.));
#3186=DIRECTION('center_axis',(0.,0.,1.));
#3187=DIRECTION('ref_axis',(0.987688340595138,-0.156434465040231,0.));
#3188=DIRECTION('',(0.,0.,-1.));
#3189=DIRECTION('center_axis',(0.,0.,1.));
#3190=DIRECTION('ref_axis',(0.951056516295154,-0.309016994374948,0.));
#3191=DIRECTION('',(0.,0.,1.));
#3192=DIRECTION('center_axis',(0.,0.,1.));
#3193=DIRECTION('ref_axis',(0.951056516295154,-0.309016994374948,0.));
#3194=DIRECTION('',(0.,0.,-1.));
#3195=DIRECTION('center_axis',(0.,0.,1.));
#3196=DIRECTION('ref_axis',(0.891006524188368,-0.453990499739547,0.));
#3197=DIRECTION('',(0.,0.,1.));
#3198=DIRECTION('center_axis',(0.,0.,1.));
#3199=DIRECTION('ref_axis',(0.891006524188368,-0.453990499739547,0.));
#3200=DIRECTION('',(0.,0.,-1.));
#3201=DIRECTION('center_axis',(0.,0.,1.));
#3202=DIRECTION('ref_axis',(0.809016994374947,-0.587785252292473,0.));
#3203=DIRECTION('',(0.,0.,1.));
#3204=DIRECTION('center_axis',(0.,0.,1.));
#3205=DIRECTION('ref_axis',(0.809016994374947,-0.587785252292473,0.));
#3206=DIRECTION('',(0.,0.,-1.));
#3207=DIRECTION('center_axis',(0.,0.,1.));
#3208=DIRECTION('ref_axis',(0.707106781186547,-0.707106781186548,0.));
#3209=DIRECTION('',(0.,0.,1.));
#3210=DIRECTION('center_axis',(0.,0.,1.));
#3211=DIRECTION('ref_axis',(0.707106781186547,-0.707106781186548,0.));
#3212=DIRECTION('',(0.,0.,-1.));
#3213=DIRECTION('center_axis',(0.,0.,1.));
#3214=DIRECTION('ref_axis',(0.587785252292473,-0.809016994374948,0.));
#3215=DIRECTION('',(0.,0.,1.));
#3216=DIRECTION('center_axis',(0.,0.,1.));
#3217=DIRECTION('ref_axis',(0.587785252292473,-0.809016994374948,0.));
#3218=DIRECTION('',(0.,0.,-1.));
#3219=DIRECTION('center_axis',(0.,0.,1.));
#3220=DIRECTION('ref_axis',(0.453990499739547,-0.891006524188368,0.));
#3221=DIRECTION('',(0.,0.,1.));
#3222=DIRECTION('center_axis',(0.,0.,1.));
#3223=DIRECTION('ref_axis',(0.453990499739547,-0.891006524188368,0.));
#3224=DIRECTION('',(0.,0.,-1.));
#3225=DIRECTION('center_axis',(0.,0.,1.));
#3226=DIRECTION('ref_axis',(0.309016994374947,-0.951056516295154,0.));
#3227=DIRECTION('',(0.,0.,1.));
#3228=DIRECTION('center_axis',(0.,0.,1.));
#3229=DIRECTION('ref_axis',(0.309016994374947,-0.951056516295154,0.));
#3230=DIRECTION('',(0.,0.,-1.));
#3231=DIRECTION('center_axis',(0.,0.,1.));
#3232=DIRECTION('ref_axis',(0.156434465040231,-0.987688340595138,0.));
#3233=DIRECTION('',(0.,0.,1.));
#3234=DIRECTION('center_axis',(0.,0.,1.));
#3235=DIRECTION('ref_axis',(0.156434465040231,-0.987688340595138,0.));
#3236=DIRECTION('',(0.,0.,-1.));
#3237=DIRECTION('center_axis',(0.,0.,1.));
#3238=DIRECTION('ref_axis',(-1.73472347597681E-16,-1.,0.));
#3239=DIRECTION('',(0.,0.,1.));
#3240=DIRECTION('center_axis',(0.,0.,1.));
#3241=DIRECTION('ref_axis',(-1.73472347597681E-16,-1.,0.));
#3242=DIRECTION('',(0.,0.,-1.));
#3243=DIRECTION('center_axis',(0.,0.,1.));
#3244=DIRECTION('ref_axis',(-0.156434465040231,-0.987688340595138,0.));
#3245=DIRECTION('',(0.,0.,1.));
#3246=DIRECTION('center_axis',(0.,0.,1.));
#3247=DIRECTION('ref_axis',(-0.156434465040231,-0.987688340595138,0.));
#3248=DIRECTION('',(0.,0.,-1.));
#3249=DIRECTION('center_axis',(0.,0.,1.));
#3250=DIRECTION('ref_axis',(-0.309016994374948,-0.951056516295154,0.));
#3251=DIRECTION('',(0.,0.,1.));
#3252=DIRECTION('center_axis',(0.,0.,1.));
#3253=DIRECTION('ref_axis',(-0.309016994374948,-0.951056516295154,0.));
#3254=DIRECTION('',(0.,0.,-1.));
#3255=DIRECTION('center_axis',(0.,0.,1.));
#3256=DIRECTION('ref_axis',(-0.453990499739547,-0.891006524188368,0.));
#3257=DIRECTION('',(0.,0.,1.));
#3258=DIRECTION('center_axis',(0.,0.,1.));
#3259=DIRECTION('ref_axis',(-0.453990499739547,-0.891006524188368,0.));
#3260=DIRECTION('',(0.,0.,-1.));
#3261=DIRECTION('center_axis',(0.,0.,1.));
#3262=DIRECTION('ref_axis',(-0.587785252292473,-0.809016994374947,0.));
#3263=DIRECTION('',(0.,0.,1.));
#3264=DIRECTION('center_axis',(0.,0.,1.));
#3265=DIRECTION('ref_axis',(-0.587785252292473,-0.809016994374947,0.));
#3266=DIRECTION('',(0.,0.,-1.));
#3267=DIRECTION('center_axis',(0.,0.,1.));
#3268=DIRECTION('ref_axis',(-0.707106781186548,-0.707106781186548,0.));
#3269=DIRECTION('',(0.,0.,1.));
#3270=DIRECTION('center_axis',(0.,0.,1.));
#3271=DIRECTION('ref_axis',(-0.707106781186548,-0.707106781186548,0.));
#3272=DIRECTION('',(0.,0.,-1.));
#3273=DIRECTION('center_axis',(0.,0.,1.));
#3274=DIRECTION('ref_axis',(-0.809016994374947,-0.587785252292473,0.));
#3275=DIRECTION('',(0.,0.,1.));
#3276=DIRECTION('center_axis',(0.,0.,1.));
#3277=DIRECTION('ref_axis',(-0.809016994374947,-0.587785252292473,0.));
#3278=DIRECTION('',(0.,0.,-1.));
#3279=DIRECTION('center_axis',(0.,0.,1.));
#3280=DIRECTION('ref_axis',(-0.891006524188368,-0.453990499739547,0.));
#3281=DIRECTION('',(0.,0.,1.));
#3282=DIRECTION('center_axis',(0.,0.,1.));
#3283=DIRECTION('ref_axis',(-0.891006524188368,-0.453990499739547,0.));
#3284=DIRECTION('',(0.,0.,-1.));
#3285=DIRECTION('center_axis',(0.,0.,1.));
#3286=DIRECTION('ref_axis',(-0.951056516295154,-0.309016994374947,0.));
#3287=DIRECTION('',(0.,0.,1.));
#3288=DIRECTION('center_axis',(0.,0.,1.));
#3289=DIRECTION('ref_axis',(-0.951056516295154,-0.309016994374947,0.));
#3290=DIRECTION('',(0.,0.,-1.));
#3291=DIRECTION('center_axis',(0.,0.,1.));
#3292=DIRECTION('ref_axis',(-0.987688340595138,-0.156434465040231,0.));
#3293=DIRECTION('',(0.,0.,1.));
#3294=DIRECTION('center_axis',(0.,0.,1.));
#3295=DIRECTION('ref_axis',(-0.987688340595138,-0.156434465040231,0.));
#3296=DIRECTION('',(0.,0.,-1.));
#3297=DIRECTION('center_axis',(0.,0.,1.));
#3298=DIRECTION('ref_axis',(-1.,1.04083408558608E-16,0.));
#3299=DIRECTION('',(0.,0.,1.));
#3300=DIRECTION('center_axis',(0.,0.,1.));
#3301=DIRECTION('ref_axis',(-1.,1.04083408558608E-16,0.));
#3302=DIRECTION('',(0.,0.,-1.));
#3303=DIRECTION('center_axis',(0.,0.,1.));
#3304=DIRECTION('ref_axis',(-0.987688340595138,0.156434465040231,0.));
#3305=DIRECTION('',(0.,0.,1.));
#3306=DIRECTION('center_axis',(0.,0.,1.));
#3307=DIRECTION('ref_axis',(-0.987688340595138,0.156434465040231,0.));
#3308=DIRECTION('',(0.,0.,-1.));
#3309=DIRECTION('center_axis',(0.,0.,1.));
#3310=DIRECTION('ref_axis',(-0.951056516295154,0.309016994374948,0.));
#3311=DIRECTION('',(0.,0.,1.));
#3312=DIRECTION('center_axis',(0.,0.,1.));
#3313=DIRECTION('ref_axis',(-0.951056516295154,0.309016994374948,0.));
#3314=DIRECTION('',(0.,0.,-1.));
#3315=DIRECTION('center_axis',(0.,0.,1.));
#3316=DIRECTION('ref_axis',(-0.891006524188368,0.453990499739547,0.));
#3317=DIRECTION('',(0.,0.,1.));
#3318=DIRECTION('center_axis',(0.,0.,1.));
#3319=DIRECTION('ref_axis',(-0.891006524188368,0.453990499739547,0.));
#3320=DIRECTION('',(0.,0.,-1.));
#3321=DIRECTION('center_axis',(0.,0.,1.));
#3322=DIRECTION('ref_axis',(-0.809016994374947,0.587785252292473,0.));
#3323=DIRECTION('',(0.,0.,1.));
#3324=DIRECTION('center_axis',(0.,0.,1.));
#3325=DIRECTION('ref_axis',(-0.809016994374947,0.587785252292473,0.));
#3326=DIRECTION('',(0.,0.,-1.));
#3327=DIRECTION('center_axis',(0.,0.,1.));
#3328=DIRECTION('ref_axis',(-0.707106781186548,0.707106781186548,0.));
#3329=DIRECTION('',(0.,0.,1.));
#3330=DIRECTION('center_axis',(0.,0.,1.));
#3331=DIRECTION('ref_axis',(-0.707106781186548,0.707106781186548,0.));
#3332=DIRECTION('',(0.,0.,-1.));
#3333=DIRECTION('center_axis',(0.,0.,1.));
#3334=DIRECTION('ref_axis',(-0.587785252292473,0.809016994374947,0.));
#3335=DIRECTION('',(0.,0.,1.));
#3336=DIRECTION('center_axis',(0.,0.,1.));
#3337=DIRECTION('ref_axis',(-0.587785252292473,0.809016994374947,0.));
#3338=DIRECTION('',(0.,0.,-1.));
#3339=DIRECTION('center_axis',(0.,0.,1.));
#3340=DIRECTION('ref_axis',(-0.453990499739547,0.891006524188368,0.));
#3341=DIRECTION('',(0.,0.,1.));
#3342=DIRECTION('center_axis',(0.,0.,1.));
#3343=DIRECTION('ref_axis',(-0.453990499739547,0.891006524188368,0.));
#3344=DIRECTION('',(0.,0.,-1.));
#3345=DIRECTION('center_axis',(0.,0.,1.));
#3346=DIRECTION('ref_axis',(-0.309016994374947,0.951056516295154,0.));
#3347=DIRECTION('',(0.,0.,1.));
#3348=DIRECTION('center_axis',(0.,0.,1.));
#3349=DIRECTION('ref_axis',(-0.309016994374947,0.951056516295154,0.));
#3350=DIRECTION('',(0.,0.,-1.));
#3351=DIRECTION('center_axis',(0.,0.,1.));
#3352=DIRECTION('ref_axis',(-0.156434465040231,0.987688340595138,0.));
#3353=DIRECTION('',(0.,0.,1.));
#3354=DIRECTION('center_axis',(0.,0.,1.));
#3355=DIRECTION('ref_axis',(-0.156434465040231,0.987688340595138,0.));
#3356=DIRECTION('',(0.,0.,-1.));
#3357=DIRECTION('center_axis',(0.,0.,1.));
#3358=DIRECTION('ref_axis',(3.46944695195361E-17,1.,0.));
#3359=DIRECTION('',(0.,0.,1.));
#3360=DIRECTION('center_axis',(0.,0.,1.));
#3361=DIRECTION('ref_axis',(3.46944695195361E-17,1.,0.));
#3362=DIRECTION('',(0.,0.,-1.));
#3363=DIRECTION('center_axis',(0.,0.,1.));
#3364=DIRECTION('ref_axis',(0.156434465040231,0.987688340595138,0.));
#3365=DIRECTION('',(0.,0.,1.));
#3366=DIRECTION('center_axis',(0.,0.,1.));
#3367=DIRECTION('ref_axis',(0.156434465040231,0.987688340595138,0.));
#3368=DIRECTION('',(0.,0.,-1.));
#3369=DIRECTION('center_axis',(0.,0.,1.));
#3370=DIRECTION('ref_axis',(0.309016994374948,0.951056516295154,0.));
#3371=DIRECTION('',(0.,0.,1.));
#3372=DIRECTION('center_axis',(0.,0.,1.));
#3373=DIRECTION('ref_axis',(0.309016994374948,0.951056516295154,0.));
#3374=DIRECTION('',(0.,0.,-1.));
#3375=DIRECTION('center_axis',(0.,0.,1.));
#3376=DIRECTION('ref_axis',(0.453990499739547,0.891006524188368,0.));
#3377=DIRECTION('',(0.,0.,1.));
#3378=DIRECTION('center_axis',(0.,0.,1.));
#3379=DIRECTION('ref_axis',(0.453990499739547,0.891006524188368,0.));
#3380=DIRECTION('',(0.,0.,-1.));
#3381=DIRECTION('center_axis',(0.,0.,1.));
#3382=DIRECTION('ref_axis',(0.587785252292473,0.809016994374947,0.));
#3383=DIRECTION('',(0.,0.,1.));
#3384=DIRECTION('center_axis',(0.,0.,1.));
#3385=DIRECTION('ref_axis',(0.587785252292473,0.809016994374947,0.));
#3386=DIRECTION('',(0.,0.,-1.));
#3387=DIRECTION('center_axis',(0.,0.,1.));
#3388=DIRECTION('ref_axis',(0.707106781186548,0.707106781186548,0.));
#3389=DIRECTION('',(0.,0.,1.));
#3390=DIRECTION('center_axis',(0.,0.,1.));
#3391=DIRECTION('ref_axis',(0.707106781186548,0.707106781186548,0.));
#3392=DIRECTION('',(0.,0.,-1.));
#3393=DIRECTION('center_axis',(0.,0.,1.));
#3394=DIRECTION('ref_axis',(0.809016994374947,0.587785252292473,0.));
#3395=DIRECTION('',(0.,0.,1.));
#3396=DIRECTION('center_axis',(0.,0.,1.));
#3397=DIRECTION('ref_axis',(0.809016994374947,0.587785252292473,0.));
#3398=DIRECTION('',(0.,0.,-1.));
#3399=DIRECTION('center_axis',(0.,0.,1.));
#3400=DIRECTION('ref_axis',(0.891006524188368,0.453990499739547,0.));
#3401=DIRECTION('',(0.,0.,1.));
#3402=DIRECTION('center_axis',(0.,0.,1.));
#3403=DIRECTION('ref_axis',(0.891006524188368,0.453990499739547,0.));
#3404=DIRECTION('',(0.,0.,-1.));
#3405=DIRECTION('center_axis',(0.,0.,1.));
#3406=DIRECTION('ref_axis',(0.951056516295154,0.309016994374947,0.));
#3407=DIRECTION('',(0.,0.,1.));
#3408=DIRECTION('center_axis',(0.,0.,1.));
#3409=DIRECTION('ref_axis',(0.951056516295154,0.309016994374947,0.));
#3410=DIRECTION('',(0.,0.,-1.));
#3411=DIRECTION('center_axis',(0.,0.,1.));
#3412=DIRECTION('ref_axis',(0.987688340595138,0.156434465040231,0.));
#3413=DIRECTION('',(0.,0.,1.));
#3414=DIRECTION('center_axis',(0.,0.,1.));
#3415=DIRECTION('ref_axis',(0.987688340595138,0.156434465040231,0.));
#3416=DIRECTION('',(0.,0.,-1.));
#3417=DIRECTION('center_axis',(0.,0.,1.));
#3418=DIRECTION('ref_axis',(1.,0.,0.));
#3419=DIRECTION('center_axis',(0.,0.,1.));
#3420=DIRECTION('ref_axis',(1.,0.,0.));
#3421=DIRECTION('center_axis',(0.,0.,1.));
#3422=DIRECTION('ref_axis',(1.,0.,0.));
#3423=DIRECTION('center_axis',(0.,0.,1.));
#3424=DIRECTION('ref_axis',(1.,0.,0.));
#3425=DIRECTION('center_axis',(0.,0.,1.));
#3426=DIRECTION('ref_axis',(1.,0.,0.));
#3427=DIRECTION('center_axis',(0.,0.,1.));
#3428=DIRECTION('ref_axis',(1.,0.,0.));
#3429=DIRECTION('center_axis',(0.,0.,1.));
#3430=DIRECTION('ref_axis',(1.,0.,0.));
#3431=DIRECTION('center_axis',(0.,0.,1.));
#3432=DIRECTION('ref_axis',(1.,0.,0.));
#3433=DIRECTION('center_axis',(0.,0.,1.));
#3434=DIRECTION('ref_axis',(1.,0.,0.));
#3435=DIRECTION('center_axis',(0.,0.,1.));
#3436=DIRECTION('ref_axis',(1.,0.,0.));
#3437=DIRECTION('center_axis',(0.,0.,1.));
#3438=DIRECTION('ref_axis',(1.,0.,0.));
#3439=DIRECTION('center_axis',(0.,0.,1.));
#3440=DIRECTION('ref_axis',(1.,0.,0.));
#3441=DIRECTION('center_axis',(0.,0.,1.));
#3442=DIRECTION('ref_axis',(1.,0.,0.));
#3443=DIRECTION('center_axis',(0.,0.,1.));
#3444=DIRECTION('ref_axis',(1.,0.,0.));
#3445=DIRECTION('center_axis',(0.,0.,1.));
#3446=DIRECTION('ref_axis',(1.,0.,0.));
#3447=DIRECTION('center_axis',(0.,0.,1.));
#3448=DIRECTION('ref_axis',(1.,0.,0.));
#3449=DIRECTION('center_axis',(0.,0.,1.));
#3450=DIRECTION('ref_axis',(1.,0.,0.));
#3451=DIRECTION('center_axis',(0.,0.,1.));
#3452=DIRECTION('ref_axis',(1.,0.,0.));
#3453=DIRECTION('center_axis',(0.,0.,1.));
#3454=DIRECTION('ref_axis',(1.,0.,0.));
#3455=DIRECTION('center_axis',(0.,0.,1.));
#3456=DIRECTION('ref_axis',(1.,0.,0.));
#3457=DIRECTION('center_axis',(0.,0.,1.));
#3458=DIRECTION('ref_axis',(1.,0.,0.));
#3459=DIRECTION('center_axis',(0.,0.,1.));
#3460=DIRECTION('ref_axis',(1.,0.,0.));
#3461=DIRECTION('center_axis',(0.,0.,1.));
#3462=DIRECTION('ref_axis',(1.,0.,0.));
#3463=DIRECTION('center_axis',(0.,0.,1.));
#3464=DIRECTION('ref_axis',(1.,0.,0.));
#3465=DIRECTION('center_axis',(0.,0.,1.));
#3466=DIRECTION('ref_axis',(1.,0.,0.));
#3467=DIRECTION('center_axis',(0.,0.,1.));
#3468=DIRECTION('ref_axis',(1.,0.,0.));
#3469=DIRECTION('center_axis',(0.,0.,1.));
#3470=DIRECTION('ref_axis',(1.,0.,0.));
#3471=DIRECTION('center_axis',(0.,0.,1.));
#3472=DIRECTION('ref_axis',(1.,0.,0.));
#3473=DIRECTION('center_axis',(0.,0.,1.));
#3474=DIRECTION('ref_axis',(1.,0.,0.));
#3475=DIRECTION('center_axis',(0.,0.,1.));
#3476=DIRECTION('ref_axis',(1.,0.,0.));
#3477=DIRECTION('center_axis',(0.,0.,1.));
#3478=DIRECTION('ref_axis',(1.,0.,0.));
#3479=DIRECTION('center_axis',(0.,0.,1.));
#3480=DIRECTION('ref_axis',(1.,0.,0.));
#3481=DIRECTION('center_axis',(0.,0.,1.));
#3482=DIRECTION('ref_axis',(1.,0.,0.));
#3483=DIRECTION('center_axis',(0.,0.,1.));
#3484=DIRECTION('ref_axis',(1.,0.,0.));
#3485=DIRECTION('center_axis',(0.,0.,1.));
#3486=DIRECTION('ref_axis',(1.,0.,0.));
#3487=DIRECTION('center_axis',(0.,0.,1.));
#3488=DIRECTION('ref_axis',(1.,0.,0.));
#3489=DIRECTION('center_axis',(0.,0.,1.));
#3490=DIRECTION('ref_axis',(1.,0.,0.));
#3491=DIRECTION('center_axis',(0.,0.,1.));
#3492=DIRECTION('ref_axis',(1.,0.,0.));
#3493=DIRECTION('center_axis',(0.,0.,1.));
#3494=DIRECTION('ref_axis',(1.,0.,0.));
#3495=DIRECTION('center_axis',(0.,0.,1.));
#3496=DIRECTION('ref_axis',(1.,0.,0.));
#3497=DIRECTION('center_axis',(0.,0.,1.));
#3498=DIRECTION('ref_axis',(1.,0.,0.));
#3499=DIRECTION('center_axis',(0.,0.,1.));
#3500=DIRECTION('ref_axis',(1.,0.,0.));
#3501=DIRECTION('center_axis',(0.,0.,1.));
#3502=DIRECTION('ref_axis',(1.,0.,0.));
#3503=DIRECTION('center_axis',(0.,0.,1.));
#3504=DIRECTION('ref_axis',(1.,0.,0.));
#3505=DIRECTION('',(0.,0.,-1.));
#3506=DIRECTION('center_axis',(0.,0.,1.));
#3507=DIRECTION('ref_axis',(1.,0.,0.));
#3508=DIRECTION('center_axis',(0.,0.,1.));
#3509=DIRECTION('ref_axis',(1.,0.,0.));
#3510=DIRECTION('center_axis',(0.,0.,1.));
#3511=DIRECTION('ref_axis',(1.,0.,0.));
#3512=DIRECTION('center_axis',(0.,0.,1.));
#3513=DIRECTION('ref_axis',(1.,0.,0.));
#3514=DIRECTION('center_axis',(0.,0.,1.));
#3515=DIRECTION('ref_axis',(1.,0.,0.));
#3516=DIRECTION('center_axis',(0.,0.,1.));
#3517=DIRECTION('ref_axis',(1.,0.,0.));
#3518=DIRECTION('center_axis',(0.,0.,1.));
#3519=DIRECTION('ref_axis',(1.,0.,0.));
#3520=DIRECTION('center_axis',(0.,0.,1.));
#3521=DIRECTION('ref_axis',(1.,0.,0.));
#3522=DIRECTION('center_axis',(0.,0.,1.));
#3523=DIRECTION('ref_axis',(1.,0.,0.));
#3524=DIRECTION('center_axis',(0.,0.,1.));
#3525=DIRECTION('ref_axis',(1.,0.,0.));
#3526=DIRECTION('center_axis',(0.,0.,1.));
#3527=DIRECTION('ref_axis',(1.,0.,0.));
#3528=DIRECTION('center_axis',(0.,0.,1.));
#3529=DIRECTION('ref_axis',(1.,0.,0.));
#3530=DIRECTION('center_axis',(0.,0.,1.));
#3531=DIRECTION('ref_axis',(1.,0.,0.));
#3532=DIRECTION('center_axis',(0.,0.,1.));
#3533=DIRECTION('ref_axis',(1.,0.,0.));
#3534=DIRECTION('center_axis',(0.,0.,1.));
#3535=DIRECTION('ref_axis',(1.,0.,0.));
#3536=DIRECTION('center_axis',(0.,0.,1.));
#3537=DIRECTION('ref_axis',(1.,0.,0.));
#3538=DIRECTION('center_axis',(0.,0.,1.));
#3539=DIRECTION('ref_axis',(1.,0.,0.));
#3540=DIRECTION('center_axis',(0.,0.,1.));
#3541=DIRECTION('ref_axis',(1.,0.,0.));
#3542=DIRECTION('center_axis',(0.,0.,1.));
#3543=DIRECTION('ref_axis',(1.,0.,0.));
#3544=DIRECTION('center_axis',(0.,0.,1.));
#3545=DIRECTION('ref_axis',(1.,0.,0.));
#3546=DIRECTION('center_axis',(0.,0.,1.));
#3547=DIRECTION('ref_axis',(1.,0.,0.));
#3548=DIRECTION('center_axis',(0.,0.,1.));
#3549=DIRECTION('ref_axis',(1.,0.,0.));
#3550=DIRECTION('center_axis',(0.,0.,1.));
#3551=DIRECTION('ref_axis',(1.,0.,0.));
#3552=DIRECTION('center_axis',(0.,0.,1.));
#3553=DIRECTION('ref_axis',(1.,0.,0.));
#3554=DIRECTION('center_axis',(0.,0.,1.));
#3555=DIRECTION('ref_axis',(1.,0.,0.));
#3556=DIRECTION('center_axis',(0.,0.,1.));
#3557=DIRECTION('ref_axis',(1.,0.,0.));
#3558=DIRECTION('center_axis',(0.,0.,1.));
#3559=DIRECTION('ref_axis',(1.,0.,0.));
#3560=DIRECTION('center_axis',(0.,0.,1.));
#3561=DIRECTION('ref_axis',(1.,0.,0.));
#3562=DIRECTION('center_axis',(0.,0.,1.));
#3563=DIRECTION('ref_axis',(1.,0.,0.));
#3564=DIRECTION('center_axis',(0.,0.,1.));
#3565=DIRECTION('ref_axis',(1.,0.,0.));
#3566=DIRECTION('center_axis',(0.,0.,1.));
#3567=DIRECTION('ref_axis',(1.,0.,0.));
#3568=DIRECTION('center_axis',(0.,0.,1.));
#3569=DIRECTION('ref_axis',(1.,0.,0.));
#3570=DIRECTION('center_axis',(0.,0.,1.));
#3571=DIRECTION('ref_axis',(1.,0.,0.));
#3572=DIRECTION('center_axis',(0.,0.,1.));
#3573=DIRECTION('ref_axis',(1.,0.,0.));
#3574=DIRECTION('center_axis',(0.,0.,1.));
#3575=DIRECTION('ref_axis',(1.,0.,0.));
#3576=DIRECTION('center_axis',(0.,0.,1.));
#3577=DIRECTION('ref_axis',(1.,0.,0.));
#3578=DIRECTION('center_axis',(0.,0.,1.));
#3579=DIRECTION('ref_axis',(1.,0.,0.));
#3580=DIRECTION('center_axis',(0.,0.,1.));
#3581=DIRECTION('ref_axis',(1.,0.,0.));
#3582=DIRECTION('center_axis',(0.,0.,1.));
#3583=DIRECTION('ref_axis',(1.,0.,0.));
#3584=DIRECTION('center_axis',(0.,0.,1.));
#3585=DIRECTION('ref_axis',(1.,0.,0.));
#3586=DIRECTION('center_axis',(0.,0.,1.));
#3587=DIRECTION('ref_axis',(1.,0.,0.));
#3588=DIRECTION('center_axis',(0.,0.,1.));
#3589=DIRECTION('ref_axis',(1.,0.,0.));
#3590=DIRECTION('center_axis',(0.,0.,1.));
#3591=DIRECTION('ref_axis',(1.,0.,0.));
#3592=DIRECTION('center_axis',(0.,0.,1.));
#3593=DIRECTION('ref_axis',(1.,0.,0.));
#3594=DIRECTION('center_axis',(0.,0.,1.));
#3595=DIRECTION('ref_axis',(1.,0.,0.));
#3596=DIRECTION('center_axis',(0.,0.,1.));
#3597=DIRECTION('ref_axis',(1.,0.,0.));
#3598=DIRECTION('center_axis',(0.,0.,1.));
#3599=DIRECTION('ref_axis',(1.,0.,0.));
#3600=DIRECTION('center_axis',(0.,0.,1.));
#3601=DIRECTION('ref_axis',(1.,0.,0.));
#3602=DIRECTION('center_axis',(0.,0.,1.));
#3603=DIRECTION('ref_axis',(1.,0.,0.));
#3604=DIRECTION('center_axis',(0.,0.,1.));
#3605=DIRECTION('ref_axis',(1.,0.,0.));
#3606=DIRECTION('center_axis',(0.,0.,1.));
#3607=DIRECTION('ref_axis',(1.,0.,0.));
#3608=DIRECTION('center_axis',(0.,0.,1.));
#3609=DIRECTION('ref_axis',(1.,0.,0.));
#3610=DIRECTION('center_axis',(0.,0.,1.));
#3611=DIRECTION('ref_axis',(1.,0.,0.));
#3612=DIRECTION('center_axis',(0.,0.,1.));
#3613=DIRECTION('ref_axis',(1.,0.,0.));
#3614=DIRECTION('center_axis',(0.,0.,1.));
#3615=DIRECTION('ref_axis',(1.,0.,0.));
#3616=DIRECTION('center_axis',(0.,0.,1.));
#3617=DIRECTION('ref_axis',(1.,0.,0.));
#3618=DIRECTION('center_axis',(0.,0.,1.));
#3619=DIRECTION('ref_axis',(1.,0.,0.));
#3620=DIRECTION('center_axis',(0.,0.,1.));
#3621=DIRECTION('ref_axis',(1.,0.,0.));
#3622=DIRECTION('center_axis',(0.,0.,1.));
#3623=DIRECTION('ref_axis',(1.,0.,0.));
#3624=DIRECTION('center_axis',(0.,0.,1.));
#3625=DIRECTION('ref_axis',(1.,0.,0.));
#3626=DIRECTION('center_axis',(0.,0.,1.));
#3627=DIRECTION('ref_axis',(1.,0.,0.));
#3628=DIRECTION('center_axis',(0.,0.,1.));
#3629=DIRECTION('ref_axis',(1.,0.,0.));
#3630=DIRECTION('center_axis',(0.,0.,1.));
#3631=DIRECTION('ref_axis',(1.,0.,0.));
#3632=DIRECTION('center_axis',(0.,0.,1.));
#3633=DIRECTION('ref_axis',(1.,0.,0.));
#3634=DIRECTION('center_axis',(0.,0.,1.));
#3635=DIRECTION('ref_axis',(1.,0.,0.));
#3636=DIRECTION('center_axis',(0.,0.,1.));
#3637=DIRECTION('ref_axis',(1.,0.,0.));
#3638=DIRECTION('center_axis',(0.,0.,1.));
#3639=DIRECTION('ref_axis',(1.,0.,0.));
#3640=DIRECTION('center_axis',(0.,0.,1.));
#3641=DIRECTION('ref_axis',(1.,0.,0.));
#3642=DIRECTION('center_axis',(0.,0.,1.));
#3643=DIRECTION('ref_axis',(1.,0.,0.));
#3644=DIRECTION('center_axis',(0.,0.,1.));
#3645=DIRECTION('ref_axis',(1.,0.,0.));
#3646=DIRECTION('center_axis',(0.,0.,1.));
#3647=DIRECTION('ref_axis',(1.,0.,0.));
#3648=DIRECTION('center_axis',(0.,0.,1.));
#3649=DIRECTION('ref_axis',(1.,0.,0.));
#3650=DIRECTION('center_axis',(0.,0.,1.));
#3651=DIRECTION('ref_axis',(1.,0.,0.));
#3652=DIRECTION('center_axis',(0.,0.,1.));
#3653=DIRECTION('ref_axis',(1.,0.,0.));
#3654=DIRECTION('center_axis',(0.,0.,1.));
#3655=DIRECTION('ref_axis',(1.,0.,0.));
#3656=DIRECTION('center_axis',(0.,0.,1.));
#3657=DIRECTION('ref_axis',(1.,0.,0.));
#3658=DIRECTION('center_axis',(0.,0.,1.));
#3659=DIRECTION('ref_axis',(1.,0.,0.));
#3660=DIRECTION('center_axis',(1.22464679914735E-16,-1.,0.));
#3661=DIRECTION('ref_axis',(-1.,-1.22464679914735E-16,0.));
#3662=DIRECTION('center_axis',(0.,0.,1.));
#3663=DIRECTION('ref_axis',(1.,0.,0.));
#3664=DIRECTION('center_axis',(0.,0.,1.));
#3665=DIRECTION('ref_axis',(1.,0.,0.));
#3666=DIRECTION('',(0.,0.,1.));
#3667=DIRECTION('center_axis',(0.,0.,1.));
#3668=DIRECTION('ref_axis',(1.,0.,0.));
#3669=DIRECTION('center_axis',(0.,0.,1.));
#3670=DIRECTION('ref_axis',(1.,0.,0.));
#3671=DIRECTION('center_axis',(0.,0.,1.));
#3672=DIRECTION('ref_axis',(1.,0.,0.));
#3673=DIRECTION('axis',(0.,0.,1.));
#3674=DIRECTION('refdir',(1.,0.,0.));
#3675=DIRECTION('center_axis',(0.,0.,1.));
#3676=DIRECTION('ref_axis',(1.,0.,0.));
#3677=DIRECTION('center_axis',(0.,0.,1.));
#3678=DIRECTION('ref_axis',(-1.,0.,0.));
#3679=DIRECTION('',(0.819152044288992,1.00317192905353E-16,-0.573576436351045));
#3680=DIRECTION('center_axis',(0.,0.,1.));
#3681=DIRECTION('ref_axis',(1.,0.,0.));
#3682=DIRECTION('center_axis',(0.,0.,1.));
#3683=DIRECTION('ref_axis',(1.,0.,0.));
#3684=DIRECTION('center_axis',(0.,0.,-1.));
#3685=DIRECTION('ref_axis',(-1.,0.,0.));
#3686=DIRECTION('center_axis',(1.22464679914735E-16,-1.,0.));
#3687=DIRECTION('ref_axis',(-1.,-1.22464679914735E-16,0.));
#3688=DIRECTION('center_axis',(0.,0.,1.));
#3689=DIRECTION('ref_axis',(1.,0.,0.));
#3690=DIRECTION('center_axis',(0.,0.,1.));
#3691=DIRECTION('ref_axis',(1.,0.,0.));
#3692=DIRECTION('',(-0.819152044288992,-1.00317192905353E-16,0.573576436351045));
#3693=DIRECTION('center_axis',(0.,0.,1.));
#3694=DIRECTION('ref_axis',(1.,0.,0.));
#3695=DIRECTION('center_axis',(0.,0.,1.));
#3696=DIRECTION('ref_axis',(1.,0.,0.));
#3697=DIRECTION('center_axis',(0.,0.,1.));
#3698=DIRECTION('ref_axis',(1.,0.,0.));
#3699=DIRECTION('center_axis',(-1.22464679914735E-16,1.,0.));
#3700=DIRECTION('ref_axis',(-1.,-1.22464679914735E-16,0.));
#3701=DIRECTION('center_axis',(0.,0.,1.));
#3702=DIRECTION('ref_axis',(1.,0.,0.));
#3703=DIRECTION('',(0.,0.,1.));
#3704=DIRECTION('center_axis',(0.,0.,1.));
#3705=DIRECTION('ref_axis',(1.,0.,0.));
#3706=DIRECTION('center_axis',(0.,0.,1.));
#3707=DIRECTION('ref_axis',(1.,0.,0.));
#3708=DIRECTION('center_axis',(0.,0.,1.));
#3709=DIRECTION('ref_axis',(1.,0.,0.));
#3710=DIRECTION('center_axis',(1.22464679914735E-16,-1.,0.));
#3711=DIRECTION('ref_axis',(-1.,-1.22464679914735E-16,0.));
#3712=DIRECTION('axis',(0.,0.,1.));
#3713=DIRECTION('refdir',(1.,0.,0.));
#3714=DIRECTION('center_axis',(1.22464679914735E-16,0.,-1.));
#3715=DIRECTION('ref_axis',(-1.,0.,-1.22464679914735E-16));
#3716=DIRECTION('center_axis',(1.22464679914735E-16,0.,-1.));
#3717=DIRECTION('ref_axis',(1.,0.,1.22464679914735E-16));
#3718=DIRECTION('',(-0.819152044288992,1.00317192905353E-16,0.573576436351045));
#3719=DIRECTION('center_axis',(1.22464679914735E-16,0.,-1.));
#3720=DIRECTION('ref_axis',(-1.,0.,-1.22464679914735E-16));
#3721=DIRECTION('center_axis',(1.22464679914735E-16,0.,-1.));
#3722=DIRECTION('ref_axis',(-1.,0.,-2.06690039817172E-16));
#3723=DIRECTION('center_axis',(-1.22464679914735E-16,0.,1.));
#3724=DIRECTION('ref_axis',(1.,0.,1.22464679914735E-16));
#3725=DIRECTION('center_axis',(-1.22464679914735E-16,-1.,-1.49975978266185E-32));
#3726=DIRECTION('ref_axis',(1.,-1.22464679914735E-16,0.));
#3727=DIRECTION('center_axis',(1.22464679914735E-16,0.,-1.));
#3728=DIRECTION('ref_axis',(-1.,0.,-1.22464679914735E-16));
#3729=DIRECTION('center_axis',(1.22464679914735E-16,0.,-1.));
#3730=DIRECTION('ref_axis',(-1.,0.,-1.22464679914735E-16));
#3731=DIRECTION('',(0.819152044288992,-1.00317192905353E-16,-0.573576436351045));
#3732=DIRECTION('center_axis',(1.22464679914735E-16,0.,-1.));
#3733=DIRECTION('ref_axis',(-1.,0.,0.));
#3734=DIRECTION('center_axis',(1.22464679914735E-16,0.,-1.));
#3735=DIRECTION('ref_axis',(-1.,0.,-1.22464679914735E-16));
#3736=DIRECTION('center_axis',(1.22464679914735E-16,0.,-1.));
#3737=DIRECTION('ref_axis',(-1.,0.,-1.22464679914735E-16));
#3738=DIRECTION('center_axis',(1.22464679914735E-16,1.,1.49975978266185E-32));
#3739=DIRECTION('ref_axis',(1.,-1.22464679914735E-16,0.));
#3740=DIRECTION('center_axis',(1.22464679914735E-16,0.,-1.));
#3741=DIRECTION('ref_axis',(-1.,0.,-1.22464679914735E-16));
#3742=DIRECTION('',(1.22464679914735E-16,0.,-1.));
#3743=DIRECTION('center_axis',(1.22464679914735E-16,0.,-1.));
#3744=DIRECTION('ref_axis',(-1.,0.,-1.22464679914735E-16));
#3745=DIRECTION('center_axis',(1.22464679914735E-16,0.,-1.));
#3746=DIRECTION('ref_axis',(-1.,0.,-1.22464679914735E-16));
#3747=DIRECTION('center_axis',(1.22464679914735E-16,0.,-1.));
#3748=DIRECTION('ref_axis',(-1.,0.,0.));
#3749=DIRECTION('center_axis',(-1.22464679914735E-16,-1.,-1.49975978266185E-32));
#3750=DIRECTION('ref_axis',(1.,-1.22464679914735E-16,0.));
#3751=DIRECTION('axis',(0.,0.,1.));
#3752=DIRECTION('refdir',(1.,0.,0.));
#3753=DIRECTION('center_axis',(1.22464679914735E-15,1.,0.));
#3754=DIRECTION('ref_axis',(0.,0.,1.));
#3755=DIRECTION('center_axis',(0.,1.,0.));
#3756=DIRECTION('ref_axis',(0.,0.,1.));
#3757=DIRECTION('axis',(0.,0.,1.));
#3758=DIRECTION('refdir',(1.,0.,0.));
#3759=DIRECTION('center_axis',(0.499999999999999,-0.866025403784439,0.));
#3760=DIRECTION('ref_axis',(-0.866025403784439,-0.499999999999999,0.));
#3761=DIRECTION('',(0.,0.,1.));
#3762=DIRECTION('',(0.,0.,-1.));
#3763=DIRECTION('center_axis',(1.,-6.86060968596774E-16,0.));
#3764=DIRECTION('ref_axis',(-6.86060968596774E-16,-1.,0.));
#3765=DIRECTION('',(0.,0.,1.));
#3766=DIRECTION('center_axis',(0.,0.,1.));
#3767=DIRECTION('ref_axis',(-1.,0.,0.));
#3768=DIRECTION('center_axis',(0.,0.,-1.));
#3769=DIRECTION('ref_axis',(1.,0.,0.));
#3770=DIRECTION('',(0.90630778703665,-1.10990693043675E-16,0.4226182617407));
#3771=DIRECTION('center_axis',(-0.500000000000001,-0.866025403784438,0.));
#3772=DIRECTION('ref_axis',(-0.866025403784438,0.500000000000001,0.));
#3773=DIRECTION('',(0.,0.,1.));
#3774=DIRECTION('center_axis',(-1.,8.0852564851151E-16,0.));
#3775=DIRECTION('ref_axis',(8.0852564851151E-16,1.,0.));
#3776=DIRECTION('',(0.,0.,1.));
#3777=DIRECTION('center_axis',(-0.499999999999999,0.866025403784439,0.));
#3778=DIRECTION('ref_axis',(0.866025403784439,0.499999999999999,0.));
#3779=DIRECTION('',(0.,0.,1.));
#3780=DIRECTION('center_axis',(0.500000000000001,0.866025403784438,0.));
#3781=DIRECTION('ref_axis',(0.866025403784438,-0.500000000000001,0.));
#3782=DIRECTION('center_axis',(0.,0.,1.));
#3783=DIRECTION('ref_axis',(1.,0.,0.));
#3784=DIRECTION('center_axis',(0.,0.,-1.));
#3785=DIRECTION('ref_axis',(1.,0.,0.));
#3786=DIRECTION('center_axis',(0.,0.,1.));
#3787=DIRECTION('ref_axis',(-1.,0.,0.));
#3788=DIRECTION('center_axis',(0.,0.,-1.));
#3789=DIRECTION('ref_axis',(-1.,0.,0.));
#3790=DIRECTION('',(-0.906307787036652,1.10990693043676E-16,0.422618261740694));
#3791=DIRECTION('center_axis',(0.,0.,-1.));
#3792=DIRECTION('ref_axis',(-1.,0.,0.));
#3793=DIRECTION('center_axis',(0.,0.,-1.));
#3794=DIRECTION('ref_axis',(-1.,0.,0.));
#3795=DIRECTION('center_axis',(0.,0.,-1.));
#3796=DIRECTION('ref_axis',(-1.,0.,0.));
#3797=DIRECTION('',(0.,0.,1.));
#3798=DIRECTION('',(0.,0.,1.));
#3799=DIRECTION('',(1.,0.,0.));
#3800=DIRECTION('',(-6.75927761365802E-16,-1.82500828378151E-21,1.));
#3801=DIRECTION('',(0.999845047128833,0.0176034579538952,1.91490496553357E-15));
#3802=DIRECTION('',(0.,0.,1.));
#3803=DIRECTION('',(1.,0.,0.));
#3804=DIRECTION('',(0.,0.,1.));
#3805=DIRECTION('',(1.,0.,0.));
#3806=DIRECTION('',(0.,0.,1.));
#3807=DIRECTION('',(1.,0.,0.));
#3808=CARTESIAN_POINT('',(0.,0.,0.));
#3809=CARTESIAN_POINT('',(0.,0.,0.));
#3810=CARTESIAN_POINT('Origin',(0.,0.,0.));
#3811=CARTESIAN_POINT('',(-2.45356474526275,0.00152995343032009,5.25782749621206));
#3812=CARTESIAN_POINT('',(1.07686357729864,2.20575430139124,5.00004572388937));
#3813=CARTESIAN_POINT('Ctrl Pts',(-2.45356474526275,0.00152995343032009,
5.25782749621206));
#3814=CARTESIAN_POINT('Ctrl Pts',(-2.45409117603731,0.080350384053512,5.25371719896929));
#3815=CARTESIAN_POINT('Ctrl Pts',(-2.41487113252746,0.971399642855625,5.2072215692543));
#3816=CARTESIAN_POINT('Ctrl Pts',(-1.36218010227536,2.52198105473234,5.12129431181338));
#3817=CARTESIAN_POINT('Ctrl Pts',(0.395824647622223,2.53385365630773,5.03947735161525));
#3818=CARTESIAN_POINT('Ctrl Pts',(1.07686357729864,2.20575430139124,5.00004572388937));
#3819=CARTESIAN_POINT('',(-1.07508846035114,2.20207516956615,5.));
#3820=CARTESIAN_POINT('Origin',(0.,0.,5.));
#3821=CARTESIAN_POINT('',(-2.45049860469171,0.00261503422208265,5.14217250381425));
#3822=CARTESIAN_POINT('Ctrl Pts',(-1.07508846035114,2.20207516956616,4.99999999999999));
#3823=CARTESIAN_POINT('Ctrl Pts',(-1.14997601337418,2.16551386358001,5.00432999723329));
#3824=CARTESIAN_POINT('Ctrl Pts',(-1.22304980119226,2.12510255608252,5.00865999446659));
#3825=CARTESIAN_POINT('Ctrl Pts',(-1.29390582758922,2.08104732270332,5.01298999169989));
#3826=CARTESIAN_POINT('Ctrl Pts',(-1.36471897746647,2.03701874810219,5.01731736875787));
#3827=CARTESIAN_POINT('Ctrl Pts',(-1.43331666889977,1.98935086391144,5.02164474581584));
#3828=CARTESIAN_POINT('Ctrl Pts',(-1.49932095835489,1.9382948469822,5.02597212287382));
#3829=CARTESIAN_POINT('Ctrl Pts',(-1.56531867275687,1.88724391602582,5.03029906885778));
#3830=CARTESIAN_POINT('Ctrl Pts',(-1.62872314993186,1.83280578064197,5.03462601484175));
#3831=CARTESIAN_POINT('Ctrl Pts',(-1.68918738086506,1.77527356830609,5.03895296082571));
#3832=CARTESIAN_POINT('Ctrl Pts',(-1.7496502279544,1.717742672709,5.04327980777893));
#3833=CARTESIAN_POINT('Ctrl Pts',(-1.80717264793702,1.65711813963895,5.04760665473215));
#3834=CARTESIAN_POINT('Ctrl Pts',(-1.86144348904875,1.59373096445982,5.05193350168537));
#3835=CARTESIAN_POINT('Ctrl Pts',(-1.91572620376788,1.53032992116261,5.05626129528472));
#3836=CARTESIAN_POINT('Ctrl Pts',(-1.96675564225295,1.46416536295762,5.06058908888408));
#3837=CARTESIAN_POINT('Ctrl Pts',(-2.01426073044554,1.39560164795869,5.06491688248343));
#3838=CARTESIAN_POINT('Ctrl Pts',(-2.06178769630728,1.32700635709431,5.06924666917532));
#3839=CARTESIAN_POINT('Ctrl Pts',(-2.1057868362227,1.25601006801191,5.07357645586721));
#3840=CARTESIAN_POINT('Ctrl Pts',(-2.14603079884992,1.18300552001569,5.0779062425591));
#3841=CARTESIAN_POINT('Ctrl Pts',(-2.18633477118484,1.10989211142771,5.08224248560412));
#3842=CARTESIAN_POINT('Ctrl Pts',(-2.22287217294086,1.03476484378008,5.08657872864913));
#3843=CARTESIAN_POINT('Ctrl Pts',(-2.25546198297408,0.958040444531769,5.09091497169414));
#3844=CARTESIAN_POINT('Ctrl Pts',(-2.28807677467307,0.881257232320273,5.09525453867919));
#3845=CARTESIAN_POINT('Ctrl Pts',(-2.3167377947772,0.802874856085788,5.09959410566424));
#3846=CARTESIAN_POINT('Ctrl Pts',(-2.3413133247558,0.723327149580979,5.10393367264929));
#3847=CARTESIAN_POINT('Ctrl Pts',(-2.36593742471167,0.643622228550178,5.10828181616026));
#3848=CARTESIAN_POINT('Ctrl Pts',(-2.38645979089026,0.562747795751204,5.11262995967123));
#3849=CARTESIAN_POINT('Ctrl Pts',(-2.40279937300748,0.481150104515044,5.1169781031822));
#3850=CARTESIAN_POINT('Ctrl Pts',(-2.41554830353427,0.417483647854612,5.12037073459371));
#3851=CARTESIAN_POINT('Ctrl Pts',(-2.4257518367838,0.353377142239134,5.12376336600522));
#3852=CARTESIAN_POINT('Ctrl Pts',(-2.4333934596506,0.289044149793245,5.12715599741673));
#3853=CARTESIAN_POINT('Ctrl Pts',(-2.44466794097471,0.194126992207884,5.13216149954048));
#3854=CARTESIAN_POINT('Ctrl Pts',(-2.45039629736826,0.0984852538315921,
5.13716700166423));
#3855=CARTESIAN_POINT('Ctrl Pts',(-2.45049860469117,0.00261503472503235,
5.14217250378799));
#3856=CARTESIAN_POINT('',(-2.45037982140539,0.00118543379578927,5.94217245212152));
#3857=CARTESIAN_POINT('Ctrl Pts',(-2.45049860469171,0.00261503422208265,
5.14217250381425));
#3858=CARTESIAN_POINT('Ctrl Pts',(-2.45058302321086,-0.0764919471070318,
5.14630277666366));
#3859=CARTESIAN_POINT('Ctrl Pts',(-2.44683272820233,-0.155776824651178,
5.15043304951307));
#3860=CARTESIAN_POINT('Ctrl Pts',(-2.43922269256381,-0.234825267128065,
5.15456332236248));
#3861=CARTESIAN_POINT('Ctrl Pts',(-2.43156489589117,-0.314369822308958,
5.15871951704877));
#3862=CARTESIAN_POINT('Ctrl Pts',(-2.41999865856044,-0.393674469734343,
5.16287571173506));
#3863=CARTESIAN_POINT('Ctrl Pts',(-2.40455179794988,-0.472314409028569,
5.16703190642135));
#3864=CARTESIAN_POINT('Ctrl Pts',(-2.38923709986016,-0.550281509169413,
5.17115254092615));
#3865=CARTESIAN_POINT('Ctrl Pts',(-2.37010800517999,-0.627594741949263,
5.17527317543095));
#3866=CARTESIAN_POINT('Ctrl Pts',(-2.34724361971563,-0.703844897476893,
5.17939380993574));
#3867=CARTESIAN_POINT('Ctrl Pts',(-2.32439056232828,-0.780057275140982,
5.18351240288709));
#3868=CARTESIAN_POINT('Ctrl Pts',(-2.29780602312865,-0.855207153541872,
5.18763099583844));
#3869=CARTESIAN_POINT('Ctrl Pts',(-2.26761965700325,-0.928897917519714,
5.19174958878978));
#3870=CARTESIAN_POINT('Ctrl Pts',(-2.23743809527637,-1.00257695303062,5.19586752623454));
#3871=CARTESIAN_POINT('Ctrl Pts',(-2.20365602983411,-1.0747968840735,5.1999854636793));
#3872=CARTESIAN_POINT('Ctrl Pts',(-2.16645157775396,-1.14518025273202,5.20410340112406));
#3873=CARTESIAN_POINT('Ctrl Pts',(-2.12864982133805,-1.21669360151161,5.20828745059984));
#3874=CARTESIAN_POINT('Ctrl Pts',(-2.08731503604085,-1.28631042558811,5.21247150007563));
#3875=CARTESIAN_POINT('Ctrl Pts',(-2.04268202130169,-1.3536618521074,5.21665554955141));
#3876=CARTESIAN_POINT('Ctrl Pts',(-1.99869777550263,-1.42003428328317,5.22077878123661));
#3877=CARTESIAN_POINT('Ctrl Pts',(-1.9515109020942,-1.48420638414124,5.2249020129218));
#3878=CARTESIAN_POINT('Ctrl Pts',(-1.90138785861859,-1.54585719298317,5.229025244607));
#3879=CARTESIAN_POINT('Ctrl Pts',(-1.85015584055906,-1.60887202873456,5.23323970297808));
#3880=CARTESIAN_POINT('Ctrl Pts',(-1.79585653538997,-1.66925227002323,5.23745416134915));
#3881=CARTESIAN_POINT('Ctrl Pts',(-1.73881377385387,-1.72669537262832,5.24166861972023));
#3882=CARTESIAN_POINT('Ctrl Pts',(-1.68177101231777,-1.78413847523342,5.24588307809131));
#3883=CARTESIAN_POINT('Ctrl Pts',(-1.62198524404679,-1.83864413938822,5.25009753646239));
#3884=CARTESIAN_POINT('Ctrl Pts',(-1.55981367463781,-1.88995543609178,5.25431199483346));
#3885=CARTESIAN_POINT('Ctrl Pts',(-1.49730868428688,-1.94154191100047,5.25854905499332));
#3886=CARTESIAN_POINT('Ctrl Pts',(-1.43212632800358,-1.99011962445967,5.26278611515318));
#3887=CARTESIAN_POINT('Ctrl Pts',(-1.36458787377452,-2.03539926912327,5.26702317531304));
#3888=CARTESIAN_POINT('Ctrl Pts',(-1.29714621498398,-2.08061401945206,5.27125416296056));
#3889=CARTESIAN_POINT('Ctrl Pts',(-1.22735554698235,-2.12253983351051,5.27548515060809));
#3890=CARTESIAN_POINT('Ctrl Pts',(-1.15557029346231,-2.16092747376385,5.27971613825561));
#3891=CARTESIAN_POINT('Ctrl Pts',(-1.08363789016749,-2.19939380333486,5.28395579883872));
#3892=CARTESIAN_POINT('Ctrl Pts',(-1.00970308479543,-2.23430714871968,5.28819545942183));
#3893=CARTESIAN_POINT('Ctrl Pts',(-0.934151886214295,-2.26546032926694,
5.29243512000494));
#3894=CARTESIAN_POINT('Ctrl Pts',(-0.858891746631583,-2.29649349300841,
5.29665844740755));
#3895=CARTESIAN_POINT('Ctrl Pts',(-0.782028071175863,-2.32379522194956,
5.30088177481017));
#3896=CARTESIAN_POINT('Ctrl Pts',(-0.703965558134562,-2.34720743500874,
5.30510510221278));
#3897=CARTESIAN_POINT('Ctrl Pts',(-0.625929411642454,-2.37061174031241,
5.30932700313595));
#3898=CARTESIAN_POINT('Ctrl Pts',(-0.54669567529644,-2.39012900583903,5.31354890405913));
#3899=CARTESIAN_POINT('Ctrl Pts',(-0.46668533523853,-2.40565064959011,5.31777080498231));
#3900=CARTESIAN_POINT('Ctrl Pts',(-0.386677700793962,-2.42117176846444,
5.32199256313854));
#3901=CARTESIAN_POINT('Ctrl Pts',(-0.305893969996252,-2.43269744697983,
5.32621432129477));
#3902=CARTESIAN_POINT('Ctrl Pts',(-0.224765082065273,-2.44017026206865,
5.33043607945101));
#3903=CARTESIAN_POINT('Ctrl Pts',(-0.143042369608102,-2.44769777457774,
5.33468873885094));
#3904=CARTESIAN_POINT('Ctrl Pts',(-0.0609698994006798,-2.45111278889587,
5.33894139825088));
#3905=CARTESIAN_POINT('Ctrl Pts',(0.0210086863910375,-2.45040994225377,
5.34319405765081));
#3906=CARTESIAN_POINT('Ctrl Pts',(0.102506869309902,-2.44971121436467,5.34742179603297));
#3907=CARTESIAN_POINT('Ctrl Pts',(0.183911801552402,-2.44494284287907,5.35164953441514));
#3908=CARTESIAN_POINT('Ctrl Pts',(0.264791488201769,-2.43615182568244,5.3558772727973));
#3909=CARTESIAN_POINT('Ctrl Pts',(0.346386310436315,-2.42728307859481,5.36014239270612));
#3910=CARTESIAN_POINT('Ctrl Pts',(0.427446077354026,-2.41432027290381,5.36440751261494));
#3911=CARTESIAN_POINT('Ctrl Pts',(0.507538340512369,-2.39736419488361,5.36867263252375));
#3912=CARTESIAN_POINT('Ctrl Pts',(0.587630603670713,-2.38040811686342,5.37293775243257));
#3913=CARTESIAN_POINT('Ctrl Pts',(0.666754917165274,-2.35945894848903,5.37720287234138));
#3914=CARTESIAN_POINT('Ctrl Pts',(0.744496850786636,-2.33466800405728,5.3814679922502));
#3915=CARTESIAN_POINT('Ctrl Pts',(0.821746571718491,-2.31003402018549,5.38570610812086));
#3916=CARTESIAN_POINT('Ctrl Pts',(0.897911818200014,-2.28151738336742,5.38994422399153));
#3917=CARTESIAN_POINT('Ctrl Pts',(0.972575382730247,-2.2492326191186,5.39418233986219));
#3918=CARTESIAN_POINT('Ctrl Pts',(1.04713454354207,-2.21699299937175,5.39841452948143));
#3919=CARTESIAN_POINT('Ctrl Pts',(1.12019577159397,-2.18099590050983,5.40264671910067));
#3920=CARTESIAN_POINT('Ctrl Pts',(1.19135773665969,-2.14140537808727,5.4068789087199));
#3921=CARTESIAN_POINT('Ctrl Pts',(1.26264057670397,-2.10174760761241,5.41111828709269));
#3922=CARTESIAN_POINT('Ctrl Pts',(1.33201725536202,-2.05848435350727,5.41535766546549));
#3923=CARTESIAN_POINT('Ctrl Pts',(1.39910526965682,-2.01182869410358,5.41959704383828));
#3924=CARTESIAN_POINT('Ctrl Pts',(1.46596383919209,-1.9653325996634,5.42382192330003));
#3925=CARTESIAN_POINT('Ctrl Pts',(1.53054898433385,-1.91546752127288,5.42804680276178));
#3926=CARTESIAN_POINT('Ctrl Pts',(1.59250901370515,-1.86248900433475,5.43227168222353));
#3927=CARTESIAN_POINT('Ctrl Pts',(1.65445001563708,-1.80952675668392,5.43649526425791));
#3928=CARTESIAN_POINT('Ctrl Pts',(1.71376715112393,-1.75345327018786,5.44071884629229));
#3929=CARTESIAN_POINT('Ctrl Pts',(1.77014163171871,-1.69456450265437,5.44494242832668));
#3930=CARTESIAN_POINT('Ctrl Pts',(1.82651590672143,-1.63567594988227,5.44916599495808));
#3931=CARTESIAN_POINT('Ctrl Pts',(1.87994722879997,-1.5739724719131,5.45338956158949));
#3932=CARTESIAN_POINT('Ctrl Pts',(1.93015452266398,-1.50978600094179,5.45761312822089));
#3933=CARTESIAN_POINT('Ctrl Pts',(1.98068680052275,-1.44518406093918,5.46186403334139));
#3934=CARTESIAN_POINT('Ctrl Pts',(2.02795285798575,-1.37806723247651,5.4661149384619));
#3935=CARTESIAN_POINT('Ctrl Pts',(2.07170921576142,-1.30880524728823,5.4703658435824));
#3936=CARTESIAN_POINT('Ctrl Pts',(2.11524878101552,-1.23988642321256,5.47459568743348));
#3937=CARTESIAN_POINT('Ctrl Pts',(2.15531316372334,-1.16884408430403,5.47882553128456));
#3938=CARTESIAN_POINT('Ctrl Pts',(2.19170859473218,-1.09606737282755,5.48305537513565));
#3939=CARTESIAN_POINT('Ctrl Pts',(2.2283758563352,-1.02274710585042,5.48731681089086));
#3940=CARTESIAN_POINT('Ctrl Pts',(2.26131894199366,-0.947666889131624,5.49157824664608));
#3941=CARTESIAN_POINT('Ctrl Pts',(2.29038969987444,-0.871243520899339,5.49583968240129));
#3942=CARTESIAN_POINT('Ctrl Pts',(2.31946045775522,-0.794820152667054,5.50010111815651));
#3943=CARTESIAN_POINT('Ctrl Pts',(2.34465880176593,-0.717054103088672,5.50436255391172));
#3944=CARTESIAN_POINT('Ctrl Pts',(2.36588855649591,-0.638374175732132,5.50862398966694));
#3945=CARTESIAN_POINT('Ctrl Pts',(2.38693658795721,-0.560367735835114,5.51284894822095));
#3946=CARTESIAN_POINT('Ctrl Pts',(2.40416312148486,-0.481168656178992,5.51707390677496));
#3947=CARTESIAN_POINT('Ctrl Pts',(2.41743659529903,-0.401186437593617,5.52129886532898));
#3948=CARTESIAN_POINT('Ctrl Pts',(2.43069072165616,-0.321320801340671,5.52551766557016));
#3949=CARTESIAN_POINT('Ctrl Pts',(2.4400031551689,-0.240674749196244,5.52973646581135));
#3950=CARTESIAN_POINT('Ctrl Pts',(2.4452924611764,-0.159671629646227,5.53395526605254));
#3951=CARTESIAN_POINT('Ctrl Pts',(2.4506117272974,-0.0782096856960176,5.53819796276217));
#3952=CARTESIAN_POINT('Ctrl Pts',(2.45186201374226,0.00361292325704207,
5.54244065947179));
#3953=CARTESIAN_POINT('Ctrl Pts',(2.4490129663411,0.0853565503823599,5.54668335618143));
#3954=CARTESIAN_POINT('Ctrl Pts',(2.44618518850525,0.166489920403897,5.55089437903589));
#3955=CARTESIAN_POINT('Ctrl Pts',(2.4393190927792,0.247545010874237,5.55510540189036));
#3956=CARTESIAN_POINT('Ctrl Pts',(2.42843718689821,0.328090047532528,5.55931642474482));
#3957=CARTESIAN_POINT('Ctrl Pts',(2.41755900899864,0.408607490642109,5.56352600496459));
#3958=CARTESIAN_POINT('Ctrl Pts',(2.4026678150993,0.488614764977163,5.56773558518437));
#3959=CARTESIAN_POINT('Ctrl Pts',(2.38383792694924,0.567685641916697,5.57194516540414));
#3960=CARTESIAN_POINT('Ctrl Pts',(2.36500867370359,0.646753852751756,5.57615460368568));
#3961=CARTESIAN_POINT('Ctrl Pts',(2.34224109929169,0.724885275372057,5.58036404196721));
#3962=CARTESIAN_POINT('Ctrl Pts',(2.3156602336019,0.801665723674642,5.58457348024875));
#3963=CARTESIAN_POINT('Ctrl Pts',(2.28871457027766,0.879499912146572,5.58884068915166));
#3964=CARTESIAN_POINT('Ctrl Pts',(2.25785029518011,0.955945291480569,5.59310789805457));
#3965=CARTESIAN_POINT('Ctrl Pts',(2.22324864085516,1.03058999167257,5.59737510695748));
#3966=CARTESIAN_POINT('Ctrl Pts',(2.18906589337937,1.10433100165746,5.60159065465889));
#3967=CARTESIAN_POINT('Ctrl Pts',(2.15123604551934,1.17631430736382,5.60580620236031));
#3968=CARTESIAN_POINT('Ctrl Pts',(2.10997992000107,1.24616812155996,5.61002175006172));
#3969=CARTESIAN_POINT('Ctrl Pts',(2.06796540868183,1.31730601515435,5.61431478956538));
#3970=CARTESIAN_POINT('Ctrl Pts',(2.02239767096814,1.38623491878807,5.61860782906904));
#3971=CARTESIAN_POINT('Ctrl Pts',(1.97355452117658,1.4525951954841,5.6229008685727));
#3972=CARTESIAN_POINT('Ctrl Pts',(1.92471137138501,1.51895547218013,5.62719390807635));
#3973=CARTESIAN_POINT('Ctrl Pts',(1.87259318065766,1.5827467750005,5.63148694758001));
#3974=CARTESIAN_POINT('Ctrl Pts',(1.81751760834157,1.64364837887194,5.63577998708367));
#3975=CARTESIAN_POINT('Ctrl Pts',(1.7632259634663,1.7036831295005,5.64001192088601));
#3976=CARTESIAN_POINT('Ctrl Pts',(1.70585489581572,1.7611374720248,5.64424385468836));
#3977=CARTESIAN_POINT('Ctrl Pts',(1.64567929753346,1.8156789087473,5.64847578849071));
#3978=CARTESIAN_POINT('Ctrl Pts',(1.58559005334727,1.87014207659335,5.65270164931948));
#3979=CARTESIAN_POINT('Ctrl Pts',(1.52270461319807,1.92170033126185,5.65692751014826));
#3980=CARTESIAN_POINT('Ctrl Pts',(1.45733653481368,1.97005595714875,5.66115337097703));
#3981=CARTESIAN_POINT('Ctrl Pts',(1.39173516852258,2.01858415630105,5.66539431320717));
#3982=CARTESIAN_POINT('Ctrl Pts',(1.32363372862786,2.06388647329623,5.66963525543731));
#3983=CARTESIAN_POINT('Ctrl Pts',(1.25338478014428,2.10570103359966,5.67387619766745));
#3984=CARTESIAN_POINT('Ctrl Pts',(1.1835118772948,2.14729175876843,5.67809443795195));
#3985=CARTESIAN_POINT('Ctrl Pts',(1.11151480069387,2.18543173083046,5.68231267823645));
#3986=CARTESIAN_POINT('Ctrl Pts',(1.03777019224463,2.21990614172954,5.68653091852094));
#3987=CARTESIAN_POINT('Ctrl Pts',(0.964050048999357,2.25436911554173,5.69074775937962));
#3988=CARTESIAN_POINT('Ctrl Pts',(0.888583945905484,2.28516874649065,5.6949646002383));
#3989=CARTESIAN_POINT('Ctrl Pts',(0.811771830668873,2.31213683525273,5.69918144109697));
#3990=CARTESIAN_POINT('Ctrl Pts',(0.734961688191492,2.33910423139561,5.70339817365488));
#3991=CARTESIAN_POINT('Ctrl Pts',(0.656806041170815,2.36224012807259,5.70761490621278));
#3992=CARTESIAN_POINT('Ctrl Pts',(0.577722099748643,2.38142550281591,5.71183163877068));
#3993=CARTESIAN_POINT('Ctrl Pts',(0.497851152504282,2.40080180129611,5.71609033424816));
#3994=CARTESIAN_POINT('Ctrl Pts',(0.417033796931697,2.41614838032182,5.72034902972563));
#3995=CARTESIAN_POINT('Ctrl Pts',(0.335710752587426,2.42739542320512,5.72460772520311));
#3996=CARTESIAN_POINT('Ctrl Pts',(0.255072182046584,2.43854780280716,5.7288305764065));
#3997=CARTESIAN_POINT('Ctrl Pts',(0.173936876646031,2.44566941692095,5.7330534276099));
#3998=CARTESIAN_POINT('Ctrl Pts',(0.0927381853600384,2.44874455159703,5.73727627881329));
#3999=CARTESIAN_POINT('Ctrl Pts',(0.010505651769704,2.4518588396667,5.74155289642781));
#4000=CARTESIAN_POINT('Ctrl Pts',(-0.0717914012442349,2.45082288489509,
5.74582951404233));
#4001=CARTESIAN_POINT('Ctrl Pts',(-0.153706383479221,2.44567467126716,5.75010613165685));
#4002=CARTESIAN_POINT('Ctrl Pts',(-0.235621365714208,2.44052645763923,5.75438274927137));
#4003=CARTESIAN_POINT('Ctrl Pts',(-0.317153799599896,2.43126610463908,5.75865936688589));
#4004=CARTESIAN_POINT('Ctrl Pts',(-0.397867900035402,2.41798498426302,5.76293598450042));
#4005=CARTESIAN_POINT('Ctrl Pts',(-0.477732100735661,2.404843710836,5.7671675703775));
#4006=CARTESIAN_POINT('Ctrl Pts',(-0.557093977187023,2.38771681514626,5.77139915625458));
#4007=CARTESIAN_POINT('Ctrl Pts',(-0.635525202983672,2.36665543887837,5.77563074213167));
#4008=CARTESIAN_POINT('Ctrl Pts',(-0.713844126625363,2.34562421945065,5.7798562689907));
#4009=CARTESIAN_POINT('Ctrl Pts',(-0.791234601033947,2.32066982780576,5.78408179584973));
#4010=CARTESIAN_POINT('Ctrl Pts',(-0.867276616693171,2.29189474455902,5.78830732270876));
#4011=CARTESIAN_POINT('Ctrl Pts',(-0.943597579218515,2.26301410494025,5.79254835017578));
#4012=CARTESIAN_POINT('Ctrl Pts',(-1.01855970287114,2.23028476543546,5.7967893776428));
#4013=CARTESIAN_POINT('Ctrl Pts',(-1.09175188487455,2.19386145229658,5.80103040510981));
#4014=CARTESIAN_POINT('Ctrl Pts',(-1.16454567512727,2.15763639458732,5.80524834827587));
#4015=CARTESIAN_POINT('Ctrl Pts',(-1.23558832118943,2.11775768035901,5.80946629144192));
#4016=CARTESIAN_POINT('Ctrl Pts',(-1.30449538176471,2.07442571545827,5.81368423460798));
#4017=CARTESIAN_POINT('Ctrl Pts',(-1.37337981915064,2.0311079770713,5.817900792962));
#4018=CARTESIAN_POINT('Ctrl Pts',(-1.44012967023436,1.98433948674289,5.82211735131602));
#4019=CARTESIAN_POINT('Ctrl Pts',(-1.50438707258409,1.9343654736998,5.82633390967004));
#4020=CARTESIAN_POINT('Ctrl Pts',(-1.5686430541751,1.88439256560357,5.83055037479415));
#4021=CARTESIAN_POINT('Ctrl Pts',(-1.63040633035506,1.83121456195291,5.83476683991825));
#4022=CARTESIAN_POINT('Ctrl Pts',(-1.68935104864667,1.77511782269132,5.83898330504236));
#4023=CARTESIAN_POINT('Ctrl Pts',(-1.74889117827283,1.71845444005005,5.84324236144859));
#4024=CARTESIAN_POINT('Ctrl Pts',(-1.80555512371633,1.65881334288088,5.84750141785482));
#4025=CARTESIAN_POINT('Ctrl Pts',(-1.85904556160285,1.59652743474227,5.85176047426105));
#4026=CARTESIAN_POINT('Ctrl Pts',(-1.91207843569271,1.53477432793661,5.855983098174));
#4027=CARTESIAN_POINT('Ctrl Pts',(-1.96199164935102,1.47042189497707,5.86020572208694));
#4028=CARTESIAN_POINT('Ctrl Pts',(-2.00853749382785,1.40382598134089,5.86442834599988));
#4029=CARTESIAN_POINT('Ctrl Pts',(-2.05568572956717,1.33636819062541,5.86870561865276));
#4030=CARTESIAN_POINT('Ctrl Pts',(-2.09937854910837,1.26660885034991,5.87298289130563));
#4031=CARTESIAN_POINT('Ctrl Pts',(-2.13940611243684,1.19494423973166,5.87726016395851));
#4032=CARTESIAN_POINT('Ctrl Pts',(-2.17943367576532,1.12327962911341,5.88153743661139));
#4033=CARTESIAN_POINT('Ctrl Pts',(-2.21579582487487,1.04971021501664,5.88581470926427));
#4034=CARTESIAN_POINT('Ctrl Pts',(-2.24833350639357,0.974652088710637,5.89009198191714));
#4035=CARTESIAN_POINT('Ctrl Pts',(-2.28384508024982,0.892733769044993,5.89476019048722));
#4036=CARTESIAN_POINT('Ctrl Pts',(-2.31491649951914,0.808778738740961,5.8994283990573));
#4037=CARTESIAN_POINT('Ctrl Pts',(-2.3413338304259,0.72326077213077,5.90409660762737));
#4038=CARTESIAN_POINT('Ctrl Pts',(-2.36767363498142,0.637993773187956,5.90875111650998));
#4039=CARTESIAN_POINT('Ctrl Pts',(-2.38938646907818,0.551173257307184,5.91340562539258));
#4040=CARTESIAN_POINT('Ctrl Pts',(-2.40630646574033,0.463291962952379,5.91806013427519));
#4041=CARTESIAN_POINT('Ctrl Pts',(-2.42314171533485,0.37585083901515,5.92269133015207));
#4042=CARTESIAN_POINT('Ctrl Pts',(-2.43523189434834,0.287359813896116,5.92732252602895));
#4043=CARTESIAN_POINT('Ctrl Pts',(-2.44246149855737,0.198323165729345,5.93195372190583));
#4044=CARTESIAN_POINT('Ctrl Pts',(-2.44777886968742,0.132836745063649,5.93535996470161));
#4045=CARTESIAN_POINT('Ctrl Pts',(-2.45046784596014,0.0670555759183701,
5.93876620749739));
#4046=CARTESIAN_POINT('Ctrl Pts',(-2.45049971322697,0.00118552710434612,
5.94217245029317));
#4047=CARTESIAN_POINT('',(-2.45049908813342,-0.00211401449528276,6.74217252662557));
#4048=CARTESIAN_POINT('Ctrl Pts',(-2.44699185673277,0.00118279703466509,
5.94217250378798));
#4049=CARTESIAN_POINT('Ctrl Pts',(-2.44492517590112,-0.482063010132467,
5.96719766230328));
#4050=CARTESIAN_POINT('Ctrl Pts',(-2.07248530679735,-1.7867484728855,6.03460815329083));
#4051=CARTESIAN_POINT('Ctrl Pts',(0.0507853919948306,-2.89698604679681,
6.14440397675062));
#4052=CARTESIAN_POINT('Ctrl Pts',(2.46316813457006,-1.52579265015265,6.27155997416736));
#4053=CARTESIAN_POINT('Ctrl Pts',(2.61640506990387,1.24485975887081,6.39871597158408));
#4054=CARTESIAN_POINT('Ctrl Pts',(0.369930108240046,2.87373628563431,6.52587196900083));
#4055=CARTESIAN_POINT('Ctrl Pts',(-1.95817338645522,1.967226842049,6.64035747973544));
#4056=CARTESIAN_POINT('Ctrl Pts',(-2.44423549538377,0.570546928646848,6.71245765799784));
#4057=CARTESIAN_POINT('Ctrl Pts',(-2.44892931063419,-0.00211222014950052,
6.74217250378799));
#4058=CARTESIAN_POINT('',(-2.45089802721206,-0.000113383326009888,7.54217250378798));
#4059=CARTESIAN_POINT('Ctrl Pts',(-2.45049908813342,-0.00211401449528276,
6.74217252662557));
#4060=CARTESIAN_POINT('Ctrl Pts',(-2.45041450413157,-0.100161128108063,
6.74725689713589));
#4061=CARTESIAN_POINT('Ctrl Pts',(-2.44444165686557,-0.197950871715524,
6.7523412676462));
#4062=CARTESIAN_POINT('Ctrl Pts',(-2.43269561264666,-0.294859807721695,
6.75742563815651));
#4063=CARTESIAN_POINT('Ctrl Pts',(-2.42078374824785,-0.393136817685654,
6.76258178527664));
#4064=CARTESIAN_POINT('Ctrl Pts',(-2.402934606887,-0.490507979483392,6.76773793239676));
#4065=CARTESIAN_POINT('Ctrl Pts',(-2.37931704734039,-0.586345152819918,
6.77289407951689));
#4066=CARTESIAN_POINT('Ctrl Pts',(-2.36818669018654,-0.631510783322305,
6.77532404095602));
#4067=CARTESIAN_POINT('Ctrl Pts',(-2.35577585904011,-0.67633603002058,6.77775400239516));
#4068=CARTESIAN_POINT('Ctrl Pts',(-2.34210586547315,-0.720756800117959,
6.78018396383429));
#4069=CARTESIAN_POINT('Ctrl Pts',(-2.31830558549057,-0.798096029297579,
6.78441467267223));
#4070=CARTESIAN_POINT('Ctrl Pts',(-2.29062567513868,-0.87440055912202,6.78864538151017));
#4071=CARTESIAN_POINT('Ctrl Pts',(-2.25917440233834,-0.949253006220778,
6.7928760903481));
#4072=CARTESIAN_POINT('Ctrl Pts',(-2.22776831573623,-1.02399791244086,6.79710072090586));
#4073=CARTESIAN_POINT('Ctrl Pts',(-2.19260180642005,-1.09729445416125,6.80132535146361));
#4074=CARTESIAN_POINT('Ctrl Pts',(-2.15383289580862,-1.16874039330069,6.80554998202137));
#4075=CARTESIAN_POINT('Ctrl Pts',(-2.11491147857911,-1.24046738182692,6.80979123115594));
#4076=CARTESIAN_POINT('Ctrl Pts',(-2.07235939710418,-1.31032872344714,6.81403248029051));
#4077=CARTESIAN_POINT('Ctrl Pts',(-2.02638541890485,-1.37793772865461,6.81827372942508));
#4078=CARTESIAN_POINT('Ctrl Pts',(-1.98067422542635,-1.44516028452148,6.82249073581378));
#4079=CARTESIAN_POINT('Ctrl Pts',(-1.93158041197976,-1.51015579415148,6.82670774220249));
#4080=CARTESIAN_POINT('Ctrl Pts',(-1.87935425791776,-1.5725704509644,6.83092474859119));
#4081=CARTESIAN_POINT('Ctrl Pts',(-1.82714541753076,-1.63496441647614,6.83514035698536));
#4082=CARTESIAN_POINT('Ctrl Pts',(-1.77180659684868,-1.69477887183925,6.83935596537953));
#4083=CARTESIAN_POINT('Ctrl Pts',(-1.71362891028703,-1.75169238390435,6.8435715737737));
#4084=CARTESIAN_POINT('Ctrl Pts',(-1.65545267508404,-1.80860447614814,6.84778707700109));
#4085=CARTESIAN_POINT('Ctrl Pts',(-1.59443804800848,-1.86261544454416,6.85200258022848));
#4086=CARTESIAN_POINT('Ctrl Pts',(-1.53091258600426,-1.91344111589924,6.85621808345588));
#4087=CARTESIAN_POINT('Ctrl Pts',(-1.46671422244237,-1.96480516465994,6.86047823993881));
#4088=CARTESIAN_POINT('Ctrl Pts',(-1.39995188287686,-2.01291571814626,6.86473839642174));
#4089=CARTESIAN_POINT('Ctrl Pts',(-1.33099594387263,-2.0575227938943,6.86899855290467));
#4090=CARTESIAN_POINT('Ctrl Pts',(-1.26266340470618,-2.10172659699916,6.8732201952161));
#4091=CARTESIAN_POINT('Ctrl Pts',(-1.19217720728943,-2.14248983244165,6.87744183752754));
#4092=CARTESIAN_POINT('Ctrl Pts',(-1.11992323469428,-2.17961514914718,6.88166347983897));
#4093=CARTESIAN_POINT('Ctrl Pts',(-1.04668049930741,-2.21724850894669,6.88594289340765));
#4094=CARTESIAN_POINT('Ctrl Pts',(-0.971621690954015,-2.25114342631593,
6.89022230697633));
#4095=CARTESIAN_POINT('Ctrl Pts',(-0.895168574025098,-2.28114521108979,
6.89450172054501));
#4096=CARTESIAN_POINT('Ctrl Pts',(-0.818715457096181,-2.31114699586365,
6.89878113411369));
#4097=CARTESIAN_POINT('Ctrl Pts',(-0.740868517526701,-2.33725555414097,
6.90306054768236));
#4098=CARTESIAN_POINT('Ctrl Pts',(-0.66206232679372,-2.3593693490932,6.90733996125104));
#4099=CARTESIAN_POINT('Ctrl Pts',(-0.584153156659504,-2.38123143121165,
6.91157066389883));
#4100=CARTESIAN_POINT('Ctrl Pts',(-0.505013440057136,-2.39927149929305,
6.91580136654663));
#4101=CARTESIAN_POINT('Ctrl Pts',(-0.425052711369318,-2.41335460356691,
6.92003206919443));
#4102=CARTESIAN_POINT('Ctrl Pts',(-0.345206863613683,-2.42741747440651,
6.92425669352013));
#4103=CARTESIAN_POINT('Ctrl Pts',(-0.264542800572244,-2.43753459225192,
6.92848131784583));
#4104=CARTESIAN_POINT('Ctrl Pts',(-0.183484260366025,-2.443621037763,6.93270594217153));
#4105=CARTESIAN_POINT('Ctrl Pts',(-0.102106707509254,-2.4497314369884,6.93694719285887));
#4106=CARTESIAN_POINT('Ctrl Pts',(-0.02033202273886,-2.45177924153041,6.94118844354621));
#4107=CARTESIAN_POINT('Ctrl Pts',(0.0614016513397831,-2.44973061523359,
6.94542969423356));
#4108=CARTESIAN_POINT('Ctrl Pts',(0.142667989329953,-2.44769370255433,6.94964669433473));
#4109=CARTESIAN_POINT('Ctrl Pts',(0.223893314749414,-2.44160708876568,6.9538636944359));
#4110=CARTESIAN_POINT('Ctrl Pts',(0.304644658900765,-2.43148964254492,6.95808069453707));
#4111=CARTESIAN_POINT('Ctrl Pts',(0.385369232722055,-2.42137555041539,6.96229629663693));
#4112=CARTESIAN_POINT('Ctrl Pts',(0.46561967622631,-2.40723333725683,6.9665118987368));
#4113=CARTESIAN_POINT('Ctrl Pts',(0.544968130282486,-2.38913373149692,6.97072750083666));
#4114=CARTESIAN_POINT('Ctrl Pts',(0.624314604864237,-2.3710345772607,6.97494299777157));
#4115=CARTESIAN_POINT('Ctrl Pts',(0.702758681563797,-2.34897833119276,6.97915849470648));
#4116=CARTESIAN_POINT('Ctrl Pts',(0.779884097391443,-2.32308653403956,6.98337399164139));
#4117=CARTESIAN_POINT('Ctrl Pts',(0.857826726412317,-2.29692038999302,6.98763415556025));
#4118=CARTESIAN_POINT('Ctrl Pts',(0.934422118975503,-2.26683706758557,6.99189431947912));
#4119=CARTESIAN_POINT('Ctrl Pts',(1.00925957122563,-2.23301262152489,6.99615448339798));
#4120=CARTESIAN_POINT('Ctrl Pts',(1.08342021273652,-2.19949407508605,7.00037611948614));
#4121=CARTESIAN_POINT('Ctrl Pts',(1.1558541926515,-2.16230207004578,7.00459775557429));
#4122=CARTESIAN_POINT('Ctrl Pts',(1.22618666595462,-2.12165419195379,7.00881939166244));
#4123=CARTESIAN_POINT('Ctrl Pts',(1.29748194996728,-2.08044986801952,7.01309881949666));
#4124=CARTESIAN_POINT('Ctrl Pts',(1.3666173396932,-2.03569460567398,7.01737824733088));
#4125=CARTESIAN_POINT('Ctrl Pts',(1.43323442603924,-1.98765925903208,7.0216576751651));
#4126=CARTESIAN_POINT('Ctrl Pts',(1.49985151238528,-1.93962391239019,7.02593710299932));
#4127=CARTESIAN_POINT('Ctrl Pts',(1.56394995330399,-1.88830883917688,7.03021653083354));
#4128=CARTESIAN_POINT('Ctrl Pts',(1.62520909567545,-1.83402443967734,7.03449595866776));
#4129=CARTESIAN_POINT('Ctrl Pts',(1.68577070383461,-1.78035815568479,7.0387266583088));
#4130=CARTESIAN_POINT('Ctrl Pts',(1.74378516384833,-1.72358800008596,7.04295735794985));
#4131=CARTESIAN_POINT('Ctrl Pts',(1.79891728889183,-1.66398522761654,7.04718805759089));
#4132=CARTESIAN_POINT('Ctrl Pts',(1.85397020369154,-1.60446808852574,7.05141267883844));
#4133=CARTESIAN_POINT('Ctrl Pts',(1.90614869495937,-1.54212675375599,7.05563730008599));
#4134=CARTESIAN_POINT('Ctrl Pts',(1.95515194917686,-1.47727150707984,7.05986192133354));
#4135=CARTESIAN_POINT('Ctrl Pts',(2.0043481044594,-1.41216095804961,7.0641031727815));
#4136=CARTESIAN_POINT('Ctrl Pts',(2.05034361527978,-1.34451697738083,7.06834442422946));
#4137=CARTESIAN_POINT('Ctrl Pts',(2.0928728171472,-1.27468961761142,7.07258567567741));
#4138=CARTESIAN_POINT('Ctrl Pts',(2.13515880594148,-1.20526158174212,7.07680267254844));
#4139=CARTESIAN_POINT('Ctrl Pts',(2.17401777962351,-1.1336754725011,7.08101966941946));
#4140=CARTESIAN_POINT('Ctrl Pts',(2.20923118761774,-1.06030552656162,7.08523666629049));
#4141=CARTESIAN_POINT('Ctrl Pts',(2.2444329213901,-0.986959904795115,7.08945226511003));
#4142=CARTESIAN_POINT('Ctrl Pts',(2.27599128849376,-0.911832039673232,7.09366786392958));
#4143=CARTESIAN_POINT('Ctrl Pts',(2.30373410617456,-0.835319949509226,7.09788346274913));
#4144=CARTESIAN_POINT('Ctrl Pts',(2.33147623146361,-0.758809768896756,7.10209895635781));
#4145=CARTESIAN_POINT('Ctrl Pts',(2.35540283915505,-0.680915869507141,7.10631444996649));
#4146=CARTESIAN_POINT('Ctrl Pts',(2.37539074560114,-0.60205403055912,7.11052994357517));
#4147=CARTESIAN_POINT('Ctrl Pts',(2.39559047581516,-0.522356445660494,7.11479011128428));
#4148=CARTESIAN_POINT('Ctrl Pts',(2.41176739147823,-0.441670749031801,7.1190502789934));
#4149=CARTESIAN_POINT('Ctrl Pts',(2.42384715139712,-0.360437562781768,7.12331044670251));
#4150=CARTESIAN_POINT('Ctrl Pts',(2.43581764475536,-0.279939165213943,7.12753207938472));
#4151=CARTESIAN_POINT('Ctrl Pts',(2.44376482075147,-0.198903616741039,7.13175371206694));
#4152=CARTESIAN_POINT('Ctrl Pts',(2.44766867038456,-0.117763873993241,7.13597534474915));
#4153=CARTESIAN_POINT('Ctrl Pts',(2.45162597147657,-0.0355131669321832,
7.14025477997171));
#4154=CARTESIAN_POINT('Ctrl Pts',(2.45142838658748,0.0468441146066864,7.14453421519427));
#4155=CARTESIAN_POINT('Ctrl Pts',(2.44710959158739,0.128859988984182,7.14881365041683));
#4156=CARTESIAN_POINT('Ctrl Pts',(2.4427907965873,0.21087586336168,7.15309308563939));
#4157=CARTESIAN_POINT('Ctrl Pts',(2.43435090704917,0.292549849315418,7.15737252086195));
#4158=CARTESIAN_POINT('Ctrl Pts',(2.42187728965929,0.373444298165804,7.16165195608451));
#4159=CARTESIAN_POINT('Ctrl Pts',(2.40954571588641,0.453417559541066,7.1658826591359));
#4160=CARTESIAN_POINT('Ctrl Pts',(2.39322547574155,0.532929756284854,7.1701133621873));
#4161=CARTESIAN_POINT('Ctrl Pts',(2.37296315532827,0.611552216457846,7.17434406523869));
#4162=CARTESIAN_POINT('Ctrl Pts',(2.35272994622341,0.69006171806341,7.17856868994867));
#4163=CARTESIAN_POINT('Ctrl Pts',(2.32856602028905,0.767683575355329,7.18279331465865));
#4164=CARTESIAN_POINT('Ctrl Pts',(2.30056938768783,0.84399688532224,7.18701793936863));
#4165=CARTESIAN_POINT('Ctrl Pts',(2.27246257521156,0.920610523942117,7.19125918995749));
#4166=CARTESIAN_POINT('Ctrl Pts',(2.24049289669693,0.995904824643573,7.19550044054635));
#4167=CARTESIAN_POINT('Ctrl Pts',(2.20481082779162,1.06946690629155,7.19974169113521));
#4168=CARTESIAN_POINT('Ctrl Pts',(2.1693327778759,1.14260838280003,7.20395869157024));
#4169=CARTESIAN_POINT('Ctrl Pts',(2.13018487997237,1.2140369724477,7.20817569200528));
#4170=CARTESIAN_POINT('Ctrl Pts',(2.08756345116152,1.28336631067462,7.21239269244031));
#4171=CARTESIAN_POINT('Ctrl Pts',(2.04495615221826,1.35267266482063,7.21660829485422));
#4172=CARTESIAN_POINT('Ctrl Pts',(1.99887785250892,1.41988075370587,7.22082389726814));
#4173=CARTESIAN_POINT('Ctrl Pts',(1.94956996776746,1.48463032125145,7.22503949968205));
#4174=CARTESIAN_POINT('Ctrl Pts',(1.90026331332807,1.54937827320294,7.22925499691067));
#4175=CARTESIAN_POINT('Ctrl Pts',(1.84772751669397,1.61166745644557,7.23347049413928));
#4176=CARTESIAN_POINT('Ctrl Pts',(1.79224545488461,1.67116919533764,7.2376859913679));
#4177=CARTESIAN_POINT('Ctrl Pts',(1.73617551996997,1.73130139875953,7.24194615487901));
#4178=CARTESIAN_POINT('Ctrl Pts',(1.67709683107441,1.78858637078493,7.24620631839012));
#4179=CARTESIAN_POINT('Ctrl Pts',(1.61533959407928,1.84272305184469,7.25046648190124));
#4180=CARTESIAN_POINT('Ctrl Pts',(1.55414086436869,1.89637014282231,7.25468811822962));
#4181=CARTESIAN_POINT('Ctrl Pts',(1.49031224602932,1.94692541394981,7.25890975455801));
#4182=CARTESIAN_POINT('Ctrl Pts',(1.42420691800064,1.99413763434702,7.2631313908864));
#4183=CARTESIAN_POINT('Ctrl Pts',(1.35719666169748,2.0419961517132,7.26741081798887));
#4184=CARTESIAN_POINT('Ctrl Pts',(1.28784730768326,2.08641913126966,7.27169024509135));
#4185=CARTESIAN_POINT('Ctrl Pts',(1.2165537296308,2.12719234506929,7.27596967219382));
#4186=CARTESIAN_POINT('Ctrl Pts',(1.14526015157833,2.16796555886892,7.28024909929629));
#4187=CARTESIAN_POINT('Ctrl Pts',(1.07202281667777,2.20508884352166,7.28452852639877));
#4188=CARTESIAN_POINT('Ctrl Pts',(0.997256979740272,2.23839870585187,7.28880795350124));
#4189=CARTESIAN_POINT('Ctrl Pts',(0.92334241970013,2.2713293051735,7.29303865544293));
#4190=CARTESIAN_POINT('Ctrl Pts',(0.847655992314498,2.30065677971353,7.29726935738461));
#4191=CARTESIAN_POINT('Ctrl Pts',(0.770583328745483,2.32618820895033,7.3015000593263));
#4192=CARTESIAN_POINT('Ctrl Pts',(0.693621397328081,2.35168295656796,7.30572468291663));
#4193=CARTESIAN_POINT('Ctrl Pts',(0.615277622954306,2.37339234556574,7.30994930650696));
#4194=CARTESIAN_POINT('Ctrl Pts',(0.535958946618911,2.39117089676567,7.3141739300973));
#4195=CARTESIAN_POINT('Ctrl Pts',(0.456328087768331,2.40901942080285,7.31841518096483));
#4196=CARTESIAN_POINT('Ctrl Pts',(0.375715069936116,2.42290590556192,7.32265643183236));
#4197=CARTESIAN_POINT('Ctrl Pts',(0.294548495546354,2.43273332565889,7.32689768269988));
#4198=CARTESIAN_POINT('Ctrl Pts',(0.213846033457668,2.44250455234634,7.33111468199939));
#4199=CARTESIAN_POINT('Ctrl Pts',(0.132596794460656,2.44826295159285,7.33533168129891));
#4200=CARTESIAN_POINT('Ctrl Pts',(0.0512319056561366,2.44996439603575,7.33954868059842));
#4201=CARTESIAN_POINT('Ctrl Pts',(-0.0301060089648669,2.4516652764138,7.34376428187336));
#4202=CARTESIAN_POINT('Ctrl Pts',(-0.111559032665591,2.44931186314808,7.34797988314831));
#4203=CARTESIAN_POINT('Ctrl Pts',(-0.192693572290218,2.44291208134841,7.35219548442326));
#4204=CARTESIAN_POINT('Ctrl Pts',(-0.273826087455323,2.43651245923535,7.35641098051102));
#4205=CARTESIAN_POINT('Ctrl Pts',(-0.354639670809366,2.42606670698216,7.36062647659878));
#4206=CARTESIAN_POINT('Ctrl Pts',(-0.434704833047805,2.41163470660979,7.36484197268654));
#4207=CARTESIAN_POINT('Ctrl Pts',(-0.515618391733778,2.39704978007697,7.36910213753916));
#4208=CARTESIAN_POINT('Ctrl Pts',(-0.595767094195178,2.37839369334412,7.37336230239178));
#4209=CARTESIAN_POINT('Ctrl Pts',(-0.674719044389303,2.3557810724128,7.3776224672444));
#4210=CARTESIAN_POINT('Ctrl Pts',(-0.752956939670165,2.33337296388475,7.38184410243896));
#4211=CARTESIAN_POINT('Ctrl Pts',(-0.830019217768804,2.30707981069314,7.38606573763352));
#4212=CARTESIAN_POINT('Ctrl Pts',(-0.905503439360926,2.2770625312682,7.39028737282807));
#4213=CARTESIAN_POINT('Ctrl Pts',(-0.982021045333626,2.24663431314572,7.39456680250973));
#4214=CARTESIAN_POINT('Ctrl Pts',(-1.05691661040126,2.21237943536682,7.39884623219138));
#4215=CARTESIAN_POINT('Ctrl Pts',(-1.12979623071021,2.17451390592771,7.40312566187303));
#4216=CARTESIAN_POINT('Ctrl Pts',(-1.20267585101917,2.13664837648861,7.40740509155468));
#4217=CARTESIAN_POINT('Ctrl Pts',(-1.27353913625396,2.09517249972326,7.41168452123633));
#4218=CARTESIAN_POINT('Ctrl Pts',(-1.34202380373791,2.0503468877731,7.41596395091798));
#4219=CARTESIAN_POINT('Ctrl Pts',(-1.40963924107054,2.00609021738154,7.42018906465642));
#4220=CARTESIAN_POINT('Ctrl Pts',(-1.47519193951934,1.95840092729194,7.42441417839486));
#4221=CARTESIAN_POINT('Ctrl Pts',(-1.53831148277856,1.90749784585766,7.4286392921333));
#4222=CARTESIAN_POINT('Ctrl Pts',(-1.60134028251237,1.85666794500781,7.43285833165612));
#4223=CARTESIAN_POINT('Ctrl Pts',(-1.66194251383471,1.80263371861981,7.43707737117893));
#4224=CARTESIAN_POINT('Ctrl Pts',(-1.71977605476889,1.74565763294054,7.44129641070175));
#4225=CARTESIAN_POINT('Ctrl Pts',(-1.77754248223635,1.68874766568611,7.44551055420118));
#4226=CARTESIAN_POINT('Ctrl Pts',(-1.83254627380443,1.62890294915343,7.44972469770062));
#4227=CARTESIAN_POINT('Ctrl Pts',(-1.88447894381472,1.56642566383437,7.45393884120005));
#4228=CARTESIAN_POINT('Ctrl Pts',(-1.93637859007007,1.50398810754445,7.45815030494429));
#4229=CARTESIAN_POINT('Ctrl Pts',(-1.98521069369888,1.43892166294857,7.46236176868853));
#4230=CARTESIAN_POINT('Ctrl Pts',(-2.03070498785838,1.37156388924727,7.46657323243277));
#4231=CARTESIAN_POINT('Ctrl Pts',(-2.0761844000306,1.30422814946363,7.47078331853283));
#4232=CARTESIAN_POINT('Ctrl Pts',(-2.1183279099878,1.23460295519288,7.47499340463288));
#4233=CARTESIAN_POINT('Ctrl Pts',(-2.15690765425705,1.16305615556917,7.47920349073293));
#4234=CARTESIAN_POINT('Ctrl Pts',(-2.19548669081132,1.09151066841509,7.48341349960228));
#4235=CARTESIAN_POINT('Ctrl Pts',(-2.23050187135428,1.01804405714918,7.48762350847162));
#4236=CARTESIAN_POINT('Ctrl Pts',(-2.26177122547569,0.943048871273492,7.49183351734097));
#4237=CARTESIAN_POINT('Ctrl Pts',(-2.29307152277315,0.867979472504542,7.49604769230358));
#4238=CARTESIAN_POINT('Ctrl Pts',(-2.32061840874255,0.791378908907118,7.50026186726618));
#4239=CARTESIAN_POINT('Ctrl Pts',(-2.34427827871066,0.713659303845589,7.50447604222879));
#4240=CARTESIAN_POINT('Ctrl Pts',(-2.36794930503256,0.635903051608447,7.50869220430405));
#4241=CARTESIAN_POINT('Ctrl Pts',(-2.38772955056502,0.557027159822053,7.5129083663793));
#4242=CARTESIAN_POINT('Ctrl Pts',(-2.40353614316832,0.477456027801041,7.51712452845455));
#4243=CARTESIAN_POINT('Ctrl Pts',(-2.41937149876783,0.397740101501748,7.52134836261049));
#4244=CARTESIAN_POINT('Ctrl Pts',(-2.43121868418161,0.317326869613289,7.52557219676642));
#4245=CARTESIAN_POINT('Ctrl Pts',(-2.43904654598825,0.236647832237695,7.52979603092236));
#4246=CARTESIAN_POINT('Ctrl Pts',(-2.44669215229988,0.157847238587433,7.53392152187756));
#4247=CARTESIAN_POINT('Ctrl Pts',(-2.45050364776306,0.0787934941983163,
7.53804701283277));
#4248=CARTESIAN_POINT('Ctrl Pts',(-2.45049999737776,-0.000113364912372915,
7.54217250378798));
#4249=CARTESIAN_POINT('',(-2.45049903342988,0.00217650160213615,8.34217250378799));
#4250=CARTESIAN_POINT('Ctrl Pts',(-2.45453280350633,-0.000113551477855291,
7.54217250378798));
#4251=CARTESIAN_POINT('Ctrl Pts',(-2.45453687676125,-0.00616397550014873,
7.54248831863689));
#4252=CARTESIAN_POINT('Ctrl Pts',(-2.45451644395713,-0.0122143712099649,
7.5428041334858));
#4253=CARTESIAN_POINT('Ctrl Pts',(-2.44842908042641,-0.830260217324654,
7.58550528080696));
#4254=CARTESIAN_POINT('Ctrl Pts',(-1.55054422260318,-2.44765991029051,7.67027594575146));
#4255=CARTESIAN_POINT('Ctrl Pts',(1.21840547693069,-2.62882380370893,7.79743194316818));
#4256=CARTESIAN_POINT('Ctrl Pts',(2.86986254650355,-0.398892772318102,7.92458794058493));
#4257=CARTESIAN_POINT('Ctrl Pts',(1.8891496807097,2.19689325024607,8.05174393800165));
#4258=CARTESIAN_POINT('Ctrl Pts',(-0.824246511156764,2.77774083901823,8.1788999354184));
#4259=CARTESIAN_POINT('Ctrl Pts',(-2.31451209905297,1.28030821412869,8.2757092634905));
#4260=CARTESIAN_POINT('Ctrl Pts',(-2.45124442572433,0.23411249554893,8.33013325909037));
#4261=CARTESIAN_POINT('Ctrl Pts',(-2.44926690043473,0.00218661114913343,
8.342171922218));
#4262=CARTESIAN_POINT('',(-2.45028722013793,-0.000988674397566302,9.14217254507401));
#4263=CARTESIAN_POINT('Ctrl Pts',(-2.45049903342988,0.00217650160213615,
8.34217250378799));
#4264=CARTESIAN_POINT('Ctrl Pts',(-2.45057066460465,-0.0784722442460898,
8.34635669788586));
#4265=CARTESIAN_POINT('Ctrl Pts',(-2.44665665890771,-0.159202294317952,
8.35054089198374));
#4266=CARTESIAN_POINT('Ctrl Pts',(-2.43875966949261,-0.239586152471894,
8.35472508608161));
#4267=CARTESIAN_POINT('Ctrl Pts',(-2.43086623907028,-0.319933783456873,
8.35890739445876));
#4268=CARTESIAN_POINT('Ctrl Pts',(-2.41899343344881,-0.399935061913083,
8.36308970283592));
#4269=CARTESIAN_POINT('Ctrl Pts',(-2.40319591535469,-0.479165568903431,
8.36727201121308));
#4270=CARTESIAN_POINT('Ctrl Pts',(-2.38740048245362,-0.558385617864723,
8.37145376754653));
#4271=CARTESIAN_POINT('Ctrl Pts',(-2.36768145903396,-0.636834633535446,
8.37563552387998));
#4272=CARTESIAN_POINT('Ctrl Pts',(-2.3441447116268,-0.714097907119257,8.37981728021343));
#4273=CARTESIAN_POINT('Ctrl Pts',(-2.32060357007519,-0.791375605210379,
8.38399981725125));
#4274=CARTESIAN_POINT('Ctrl Pts',(-2.29324342983371,-0.867466669906543,
8.38818235428906));
#4275=CARTESIAN_POINT('Ctrl Pts',(-2.26221968959487,-0.941972571792464,
8.39236489132688));
#4276=CARTESIAN_POINT('Ctrl Pts',(-2.23116118125722,-1.01656197194577,8.39655211570606));
#4277=CARTESIAN_POINT('Ctrl Pts',(-2.19643106527865,-1.08956222842722,8.40073934008525));
#4278=CARTESIAN_POINT('Ctrl Pts',(-2.15823215230383,-1.16059649610102,8.40492656446443));
#4279=CARTESIAN_POINT('Ctrl Pts',(-2.1200075469554,-1.23167854102297,8.40911660514713));
#4280=CARTESIAN_POINT('Ctrl Pts',(-2.07830974907275,-1.30079156321441,8.41330664582984));
#4281=CARTESIAN_POINT('Ctrl Pts',(-2.03338528483849,-1.36758712095511,8.41749668651254));
#4282=CARTESIAN_POINT('Ctrl Pts',(-1.98838819436034,-1.43449066240915,8.4216935009414));
#4283=CARTESIAN_POINT('Ctrl Pts',(-1.94015431715338,-1.49906889049394,8.42589031537025));
#4284=CARTESIAN_POINT('Ctrl Pts',(-1.88897035835948,-1.56100648148535,8.4300871297991));
#4285=CARTESIAN_POINT('Ctrl Pts',(-1.87626709970743,-1.57637866560688,8.43112872995002));
#4286=CARTESIAN_POINT('Ctrl Pts',(-1.86338229759534,-1.59158837468582,8.43217033010094));
#4287=CARTESIAN_POINT('Ctrl Pts',(-1.85032066881286,-1.60663115635293,8.43321193025186));
#4288=CARTESIAN_POINT('Ctrl Pts',(-1.79726781722413,-1.66773092243547,8.43744263219124));
#4289=CARTESIAN_POINT('Ctrl Pts',(-1.74108556238777,-1.72631496655,8.44167333413062));
#4290=CARTESIAN_POINT('Ctrl Pts',(-1.68204176569164,-1.78204538339205,8.44590403607));
#4291=CARTESIAN_POINT('Ctrl Pts',(-1.62308279868508,-1.83769573095969,8.45012865965479));
#4292=CARTESIAN_POINT('Ctrl Pts',(-1.56127079031436,-1.89050027732404,8.45435328323959));
#4293=CARTESIAN_POINT('Ctrl Pts',(-1.49691297561597,-1.94015509520052,8.45857790682439));
#4294=CARTESIAN_POINT('Ctrl Pts',(-1.43230186127501,-1.99000534462916,8.4628191576929));
#4295=CARTESIAN_POINT('Ctrl Pts',(-1.36512516917711,-2.03668066064801,8.46706040856141));
#4296=CARTESIAN_POINT('Ctrl Pts',(-1.29573025478907,-2.07991186275387,8.47130165942991));
#4297=CARTESIAN_POINT('Ctrl Pts',(-1.22673214232091,-2.1228958677251,8.47551865871598));
#4298=CARTESIAN_POINT('Ctrl Pts',(-1.15554150512803,-2.16247479059064,8.47973565800205));
#4299=CARTESIAN_POINT('Ctrl Pts',(-1.08253035737817,-2.19842631792714,8.48395265728812));
#4300=CARTESIAN_POINT('Ctrl Pts',(-1.00954341442105,-2.23436592654582,8.48816825854667));
#4301=CARTESIAN_POINT('Ctrl Pts',(-0.93473757632392,-2.26668032243561,8.49238385980521));
#4302=CARTESIAN_POINT('Ctrl Pts',(-0.858509105248819,-2.29519331782856,
8.49659946106376));
#4303=CARTESIAN_POINT('Ctrl Pts',(-0.782282536270929,-2.32370560174864,
8.50081495713217));
#4304=CARTESIAN_POINT('Ctrl Pts',(-0.704633840860815,-2.34841651185334,
8.50503045320058));
#4305=CARTESIAN_POINT('Ctrl Pts',(-0.62597753528704,-2.36919867789005,8.509245949269));
#4306=CARTESIAN_POINT('Ctrl Pts',(-0.546487761341905,-2.39020105866928,
8.51350611413563));
#4307=CARTESIAN_POINT('Ctrl Pts',(-0.465969360420922,-2.40719079973591,
8.51776627900226));
#4308=CARTESIAN_POINT('Ctrl Pts',(-0.384862181302826,-2.42008912054966,
8.5220264438689));
#4309=CARTESIAN_POINT('Ctrl Pts',(-0.304488550124497,-2.43287078662628,
8.52624807903699));
#4310=CARTESIAN_POINT('Ctrl Pts',(-0.223537222083469,-2.44163475260477,
8.53046971420508));
#4311=CARTESIAN_POINT('Ctrl Pts',(-0.142440930413969,-2.44635664434743,
8.53469134937317));
#4312=CARTESIAN_POINT('Ctrl Pts',(-0.0602344235506632,-2.45114317919334,
8.53897077908907));
#4313=CARTESIAN_POINT('Ctrl Pts',(0.0221205514842775,-2.45177612534295,
8.54325020880498));
#4314=CARTESIAN_POINT('Ctrl Pts',(0.104175698326146,-2.44828463906431,8.54752963852088));
#4315=CARTESIAN_POINT('Ctrl Pts',(0.186230845168012,-2.44479315278567,8.55180906823679));
#4316=CARTESIAN_POINT('Ctrl Pts',(0.267985681418476,-2.4371773447912,8.55608849795269));
#4317=CARTESIAN_POINT('Ctrl Pts',(0.349001701606052,-2.42552016323841,8.5603679276686));
#4318=CARTESIAN_POINT('Ctrl Pts',(0.429095231937527,-2.41399571631895,8.56459862960827));
#4319=CARTESIAN_POINT('Ctrl Pts',(0.508767946089158,-2.39847815840017,8.56882933154794));
#4320=CARTESIAN_POINT('Ctrl Pts',(0.587590724305493,-2.37900975002419,8.57306003348762));
#4321=CARTESIAN_POINT('Ctrl Pts',(0.666300255877846,-2.35956931239426,8.57728465707269));
#4322=CARTESIAN_POINT('Ctrl Pts',(0.744161829072428,-2.33618940828937,8.58150928065777));
#4323=CARTESIAN_POINT('Ctrl Pts',(0.820753574049848,-2.30896379804544,8.58573390424285));
#4324=CARTESIAN_POINT('Ctrl Pts',(0.897646768995828,-2.28163103318119,8.58997515511128));
#4325=CARTESIAN_POINT('Ctrl Pts',(0.973259648983159,-2.25042229295733,8.59421640597972));
#4326=CARTESIAN_POINT('Ctrl Pts',(1.04717783611411,-2.21548388158239,8.59845765684816));
#4327=CARTESIAN_POINT('Ctrl Pts',(1.12067335714017,-2.1807452489469,8.60267465613449));
#4328=CARTESIAN_POINT('Ctrl Pts',(1.19249308862886,-2.14231968286406,8.60689165542082));
#4329=CARTESIAN_POINT('Ctrl Pts',(1.26224870601951,-2.10039959392304,8.61110865470715));
#4330=CARTESIAN_POINT('Ctrl Pts',(1.33198119789681,-2.05849340240867,8.61532425596595));
#4331=CARTESIAN_POINT('Ctrl Pts',(1.39965053627586,-2.01309522800395,8.61953985722476));
#4332=CARTESIAN_POINT('Ctrl Pts',(1.46489404893636,-1.96444284095792,8.62375545848356));
#4333=CARTESIAN_POINT('Ctrl Pts',(1.53013593360273,-1.9157916679146,8.62797095455223));
#4334=CARTESIAN_POINT('Ctrl Pts',(1.59295174073334,-1.86388672255779,8.63218645062089));
#4335=CARTESIAN_POINT('Ctrl Pts',(1.65300995881168,-1.80900755279502,8.63640194668956));
#4336=CARTESIAN_POINT('Ctrl Pts',(1.7137045737332,-1.75354686510662,8.64066211155587));
#4337=CARTESIAN_POINT('Ctrl Pts',(1.77158244245994,-1.69504886087427,8.64492227642219));
#4338=CARTESIAN_POINT('Ctrl Pts',(1.82633919032058,-1.63384069354977,8.64918244128851));
#4339=CARTESIAN_POINT('Ctrl Pts',(1.88060070829574,-1.5731861039098,8.65340407645682));
#4340=CARTESIAN_POINT('Ctrl Pts',(1.931797086613,-1.5098705808574,8.65762571162513));
#4341=CARTESIAN_POINT('Ctrl Pts',(1.97967354563323,-1.44424475166778,8.66184734679344));
#4342=CARTESIAN_POINT('Ctrl Pts',(2.02820543747774,-1.37772049925617,8.66612677650875));
#4343=CARTESIAN_POINT('Ctrl Pts',(2.07332555080613,-1.30882261898726,8.67040620622407));
#4344=CARTESIAN_POINT('Ctrl Pts',(2.11481568600756,-1.23794380495092,8.67468563593939));
#4345=CARTESIAN_POINT('Ctrl Pts',(2.15630582120899,-1.16706499091459,8.67896506565471));
#4346=CARTESIAN_POINT('Ctrl Pts',(2.19416581018959,-1.09420570863186,8.68324449537002));
#4347=CARTESIAN_POINT('Ctrl Pts',(2.22822798017978,-1.01977954399171,8.68752392508534));
#4348=CARTESIAN_POINT('Ctrl Pts',(2.26190230088903,-0.946200833710673,8.69175462702617));
#4349=CARTESIAN_POINT('Ctrl Pts',(2.29199154861773,-0.870814010199191,8.695985328967));
#4350=CARTESIAN_POINT('Ctrl Pts',(2.31829892371557,-0.794002739478404,8.70021603090783));
#4351=CARTESIAN_POINT('Ctrl Pts',(2.34456850235416,-0.717301825418201,8.70444065449409));
#4352=CARTESIAN_POINT('Ctrl Pts',(2.36706685020363,-0.639180964925148,8.70866527808035));
#4353=CARTESIAN_POINT('Ctrl Pts',(2.38564439164319,-0.560045611197326,8.71288990166661));
#4354=CARTESIAN_POINT('Ctrl Pts',(2.40429505060717,-0.480598796387484,8.71713115253475));
#4355=CARTESIAN_POINT('Ctrl Pts',(2.418993776443,-0.400129917035782,8.7213724034029));
#4356=CARTESIAN_POINT('Ctrl Pts',(2.42963922641219,-0.319066575308621,8.72561365427104));
#4357=CARTESIAN_POINT('Ctrl Pts',(2.44022380542706,-0.238466755836126,8.72983065355859));
#4358=CARTESIAN_POINT('Ctrl Pts',(2.44680127509918,-0.157279719579152,8.73404765284614));
#4359=CARTESIAN_POINT('Ctrl Pts',(2.44932316256163,-0.0759361267060359,
8.7382646521337));
#4360=CARTESIAN_POINT('Ctrl Pts',(2.45184421396321,0.00538049898668423,
8.74248025339374));
#4361=CARTESIAN_POINT('Ctrl Pts',(2.45031233873225,0.0868531137583524,8.74669585465378));
#4362=CARTESIAN_POINT('Ctrl Pts',(2.44473108895808,0.168048066581625,8.75091145591382));
#4363=CARTESIAN_POINT('Ctrl Pts',(2.43914997845053,0.249240993380991,8.75512695198372));
#4364=CARTESIAN_POINT('Ctrl Pts',(2.42951972727187,0.330155808116043,8.75934244805361));
#4365=CARTESIAN_POINT('Ctrl Pts',(2.4158958831663,0.410362439436317,8.76355794412351));
#4366=CARTESIAN_POINT('Ctrl Pts',(2.40212767628843,0.491418966833192,8.76781810898839));
#4367=CARTESIAN_POINT('Ctrl Pts',(2.38428080292132,0.571751732834513,8.77207827385327));
#4368=CARTESIAN_POINT('Ctrl Pts',(2.36246552773785,0.650927707391768,8.77633843871815));
#4369=CARTESIAN_POINT('Ctrl Pts',(2.34084755381676,0.729387600231115,8.78056007388773));
#4370=CARTESIAN_POINT('Ctrl Pts',(2.31533287718715,0.806711114715091,8.7847817090573));
#4371=CARTESIAN_POINT('Ctrl Pts',(2.28607834965371,0.882494209184735,8.78900334422688));
#4372=CARTESIAN_POINT('Ctrl Pts',(2.25642332516109,0.959314780634891,8.79328277393941));
#4373=CARTESIAN_POINT('Ctrl Pts',(2.22292547788995,1.03455198387359,8.79756220365194));
#4374=CARTESIAN_POINT('Ctrl Pts',(2.18579683249587,1.10780975670511,8.80184163336447));
#4375=CARTESIAN_POINT('Ctrl Pts',(2.14866818710179,1.18106752953663,8.806121063077));
#4376=CARTESIAN_POINT('Ctrl Pts',(2.10790904396707,1.25234547859619,8.81040049278953));
#4377=CARTESIAN_POINT('Ctrl Pts',(2.06377634851482,1.32127871144238,8.81467992250206));
#4378=CARTESIAN_POINT('Ctrl Pts',(2.02014617047389,1.38942703529153,8.81891062444216));
#4379=CARTESIAN_POINT('Ctrl Pts',(1.97305480665095,1.45554011598564,8.82314132638225));
#4380=CARTESIAN_POINT('Ctrl Pts',(1.92271827747735,1.51924477140931,8.82737202832234));
#4381=CARTESIAN_POINT('Ctrl Pts',(1.87245406804581,1.58285790077181,8.83159665190785));
#4382=CARTESIAN_POINT('Ctrl Pts',(1.8189542389445,1.6440691152987,8.83582127549335));
#4383=CARTESIAN_POINT('Ctrl Pts',(1.76247869598671,1.70253314099696,8.84004589907886));
#4384=CARTESIAN_POINT('Ctrl Pts',(1.70578087646237,1.76122726953653,8.84428714994719));
#4385=CARTESIAN_POINT('Ctrl Pts',(1.64608412507283,1.81715213841906,8.84852840081552));
#4386=CARTESIAN_POINT('Ctrl Pts',(1.5836930833972,1.86999103409611,8.85276965168385));
#4387=CARTESIAN_POINT('Ctrl Pts',(1.52165879530245,1.92252779560878,8.85698665097064));
#4388=CARTESIAN_POINT('Ctrl Pts',(1.4569613038109,1.97201347592082,8.86120365025743));
#4389=CARTESIAN_POINT('Ctrl Pts',(1.3899364459144,2.01817415658779,8.86542064954422));
#4390=CARTESIAN_POINT('Ctrl Pts',(1.32293380822476,2.06431953397915,8.86963625080348));
#4391=CARTESIAN_POINT('Ctrl Pts',(1.25360571905227,2.10714183715056,8.87385185206275));
#4392=CARTESIAN_POINT('Ctrl Pts',(1.18231869690365,2.14640926874444,8.87806745332201));
#4393=CARTESIAN_POINT('Ctrl Pts',(1.11103345355034,2.18567572051449,8.88228294939113));
#4394=CARTESIAN_POINT('Ctrl Pts',(1.03778978228036,2.22138725363865,8.88649844546026));
#4395=CARTESIAN_POINT('Ctrl Pts',(0.962979343023657,2.25335772457675,8.89071394152938));
#4396=CARTESIAN_POINT('Ctrl Pts',(0.887376187501839,2.28566696524496,8.89497410639517));
#4397=CARTESIAN_POINT('Ctrl Pts',(0.810173301462104,2.31415518338324,8.89923427126095));
#4398=CARTESIAN_POINT('Ctrl Pts',(0.731794456775938,2.33868063724657,8.90349443612674));
#4399=CARTESIAN_POINT('Ctrl Pts',(0.654124484452999,2.36298427849567,8.90771607129554));
#4400=CARTESIAN_POINT('Ctrl Pts',(0.575300209773041,2.3833964889253,8.91193770646433));
#4401=CARTESIAN_POINT('Ctrl Pts',(0.495746255225524,2.39983038992964,8.91615934163313));
#4402=CARTESIAN_POINT('Ctrl Pts',(0.415103200255845,2.41648927244023,8.92043877134741));
#4403=CARTESIAN_POINT('Ctrl Pts',(0.333710824244754,2.42906001847969,8.92471820106169));
#4404=CARTESIAN_POINT('Ctrl Pts',(0.252016912123801,2.43750645660757,8.92899763077597));
#4405=CARTESIAN_POINT('Ctrl Pts',(0.17032300000285,2.44595289473544,8.93327706049026));
#4406=CARTESIAN_POINT('Ctrl Pts',(0.0883280451269847,2.45027506452807,8.93755649020454));
#4407=CARTESIAN_POINT('Ctrl Pts',(0.00647794685802633,2.45049143769255,
8.94183591991882));
#4408=CARTESIAN_POINT('Ctrl Pts',(-0.0744401643555323,2.45070534712159,
8.94606662185901));
#4409=CARTESIAN_POINT('Ctrl Pts',(-0.155521056560432,2.44690733381109,8.95029732379919));
#4410=CARTESIAN_POINT('Ctrl Pts',(-0.236334018065072,2.4390769733457,8.95452802573937));
#4411=CARTESIAN_POINT('Ctrl Pts',(-0.317030873580234,2.43125786295372,8.95875264932497));
#4412=CARTESIAN_POINT('Ctrl Pts',(-0.397460103947487,2.4194179558364,8.96297727291058));
#4413=CARTESIAN_POINT('Ctrl Pts',(-0.477190701373381,2.40358883433144,8.96720189649618));
#4414=CARTESIAN_POINT('Ctrl Pts',(-0.557235102658202,2.38769741253561,8.97144314736449));
#4415=CARTESIAN_POINT('Ctrl Pts',(-0.636574885291669,2.36778530622891,8.9756843982328));
#4416=CARTESIAN_POINT('Ctrl Pts',(-0.714778833415444,2.34393717264377,8.9799256491011));
#4417=CARTESIAN_POINT('Ctrl Pts',(-0.792535609354803,2.32022540329912,8.98414264838799));
#4418=CARTESIAN_POINT('Ctrl Pts',(-0.869169055689855,2.2926226341566,8.98835964767487));
#4419=CARTESIAN_POINT('Ctrl Pts',(-0.944267047301864,2.26126292000285,8.99257664696175));
#4420=CARTESIAN_POINT('Ctrl Pts',(-1.01934014228681,2.22991360228036,8.99679224822112));
#4421=CARTESIAN_POINT('Ctrl Pts',(-1.09287836460284,2.19480999197975,9.0010078494805));
#4422=CARTESIAN_POINT('Ctrl Pts',(-1.16448839141626,2.15613474445749,9.00522345073987));
#4423=CARTESIAN_POINT('Ctrl Pts',(-1.23609663137471,2.11746046198247,9.00943894680911));
#4424=CARTESIAN_POINT('Ctrl Pts',(-1.30577636281228,2.07521494143496,9.01365444287835));
#4425=CARTESIAN_POINT('Ctrl Pts',(-1.37315903482134,2.02962669352975,9.01786993894759));
#4426=CARTESIAN_POINT('Ctrl Pts',(-1.44125571600252,1.98355537740873,9.02213010381325));
#4427=CARTESIAN_POINT('Ctrl Pts',(-1.50700595679968,1.9340703289569,9.02639026867891));
#4428=CARTESIAN_POINT('Ctrl Pts',(-1.57006115166297,1.88145109690333,9.03065043354457));
#4429=CARTESIAN_POINT('Ctrl Pts',(-1.6325460640103,1.8293077626423,9.03487206871347));
#4430=CARTESIAN_POINT('Ctrl Pts',(-1.69238417959119,1.77408707324531,9.03909370388235));
#4431=CARTESIAN_POINT('Ctrl Pts',(-1.74927255891815,1.71609899615843,9.04331533905125));
#4432=CARTESIAN_POINT('Ctrl Pts',(-1.80693974500516,1.65731705735545,9.0475947687653));
#4433=CARTESIAN_POINT('Ctrl Pts',(-1.86157549088788,1.59569175573465,9.05187419847934));
#4434=CARTESIAN_POINT('Ctrl Pts',(-1.91290694908905,1.53157998619949,9.05615362819339));
#4435=CARTESIAN_POINT('Ctrl Pts',(-1.96423840729021,1.46746821666433,9.06043305790744));
#4436=CARTESIAN_POINT('Ctrl Pts',(-2.01226534397572,1.40087041543378,9.06471248762149));
#4437=CARTESIAN_POINT('Ctrl Pts',(-2.05676187417548,1.33217147655179,9.06899191733554));
#4438=CARTESIAN_POINT('Ctrl Pts',(-2.10171929270989,1.26276096444394,9.07331567273578));
#4439=CARTESIAN_POINT('Ctrl Pts',(-2.14323638783505,1.19095353206654,9.07763942813602));
#4440=CARTESIAN_POINT('Ctrl Pts',(-2.18105535464625,1.11711583551973,9.08196318353626));
#4441=CARTESIAN_POINT('Ctrl Pts',(-2.21881263121907,1.04339858290581,9.08627988603359));
#4442=CARTESIAN_POINT('Ctrl Pts',(-2.25288357200913,0.967658035312121,9.09059658853091));
#4443=CARTESIAN_POINT('Ctrl Pts',(-2.28305401222146,0.890289069504666,9.09491329102823));
#4444=CARTESIAN_POINT('Ctrl Pts',(-2.31317310560235,0.813051777322742,9.09922264696402));
#4445=CARTESIAN_POINT('Ctrl Pts',(-2.33940475210908,0.734191988265807,9.10353200289981));
#4446=CARTESIAN_POINT('Ctrl Pts',(-2.3615816991856,0.654126996898643,9.1078413588356));
#4447=CARTESIAN_POINT('Ctrl Pts',(-2.38373640869621,0.574142289373843,9.11214639363619));
#4448=CARTESIAN_POINT('Ctrl Pts',(-2.40184438315027,0.492955201522529,9.11645142843678));
#4449=CARTESIAN_POINT('Ctrl Pts',(-2.41578745660378,0.411000260968077,9.12075646323736));
#4450=CARTESIAN_POINT('Ctrl Pts',(-2.42971883039754,0.329114088961891,9.12505788567497));
#4451=CARTESIAN_POINT('Ctrl Pts',(-2.43949218192697,0.246461776577874,9.12935930811257));
#4452=CARTESIAN_POINT('Ctrl Pts',(-2.44504020385111,0.163488995200726,9.13366073055018));
#4453=CARTESIAN_POINT('Ctrl Pts',(-2.44869973006766,0.108759386547032,9.13649798829612));
#4454=CARTESIAN_POINT('Ctrl Pts',(-2.45052192610961,0.0538905871464149,
9.13933524604205));
#4455=CARTESIAN_POINT('Ctrl Pts',(-2.4504998008426,-0.000987962737744003,
9.14217250378799));
#4456=CARTESIAN_POINT('',(-2.45288802918575,-0.00174278630456637,9.94217250378798));
#4457=CARTESIAN_POINT('Ctrl Pts',(-2.44683804691476,-0.0010002212498868,
9.14217321494963));
#4458=CARTESIAN_POINT('Ctrl Pts',(-2.44809247353642,-0.348475610399284,
9.16016478155052));
#4459=CARTESIAN_POINT('Ctrl Pts',(-2.2164011699741,-1.51294856493534,9.22054168062364));
#4460=CARTESIAN_POINT('Ctrl Pts',(-0.427813805281666,-2.86569395165591,
9.32330391216903));
#4461=CARTESIAN_POINT('Ctrl Pts',(2.17773028627945,-1.91120832897776,9.45045990958575));
#4462=CARTESIAN_POINT('Ctrl Pts',(2.78591175602507,0.796192290953494,9.57761590700248));
#4463=CARTESIAN_POINT('Ctrl Pts',(0.838920969493999,2.77334420573432,9.70477190441923));
#4464=CARTESIAN_POINT('Ctrl Pts',(-1.757082399502,2.23196455382522,9.82629077001439));
#4465=CARTESIAN_POINT('Ctrl Pts',(-2.44721011341078,0.703532295850273,9.90542430313731));
#4466=CARTESIAN_POINT('Ctrl Pts',(-2.45288802918575,-0.00174278630456637,
9.94217250378798));
#4467=CARTESIAN_POINT('',(-2.45231825334198,0.00195314577384671,10.742172503788));
#4468=CARTESIAN_POINT('Ctrl Pts',(-2.45288802918575,-0.00174278630456637,
9.94217250378798));
#4469=CARTESIAN_POINT('Ctrl Pts',(-2.45375901495182,-0.109931174801997,
9.94780963560955));
#4470=CARTESIAN_POINT('Ctrl Pts',(-2.39807267662402,-1.03068064077238,9.99583209990337));
#4471=CARTESIAN_POINT('Ctrl Pts',(-1.23228710005795,-2.62234532042679,10.0862398966695));
#4472=CARTESIAN_POINT('Ctrl Pts',(1.53758172190995,-2.4558234718693,10.2133958940861));
#4473=CARTESIAN_POINT('Ctrl Pts',(2.89721701832281,-0.0368785205104102,
10.340551891503));
#4474=CARTESIAN_POINT('Ctrl Pts',(1.5995935090241,2.4158905361011,10.4677078889196));
#4475=CARTESIAN_POINT('Ctrl Pts',(-1.16513926773105,2.65286203247095,10.5948638863363));
#4476=CARTESIAN_POINT('Ctrl Pts',(-2.38547222680609,1.0727264530832,10.6863520912925));
#4477=CARTESIAN_POINT('Ctrl Pts',(-2.45344104862174,0.130954817715624,10.7354549637764));
#4478=CARTESIAN_POINT('Ctrl Pts',(-2.45231825334198,0.00195314577384671,
10.742172503788));
#4479=CARTESIAN_POINT('',(-2.44662748352118,0.00066590285712469,11.542172503788));
#4480=CARTESIAN_POINT('Ctrl Pts',(-2.45231825334198,0.00195314577384671,
10.742172503788));
#4481=CARTESIAN_POINT('Ctrl Pts',(-2.44635660235887,-0.683000699522043,
10.7778402962486));
#4482=CARTESIAN_POINT('Ctrl Pts',(-1.79037428776405,-2.19191629563671,10.8558934211814));
#4483=CARTESIAN_POINT('Ctrl Pts',(0.768057096932581,-2.79379934361555,10.9763318785866));
#4484=CARTESIAN_POINT('Ctrl Pts',(2.76474302699328,-0.866846278890543,11.1034878760034));
#4485=CARTESIAN_POINT('Ctrl Pts',(2.22567215749589,1.85515765472443,11.23064387342));
#4486=CARTESIAN_POINT('Ctrl Pts',(-0.354732482212946,2.8756549415042,11.3577998708367));
#4487=CARTESIAN_POINT('Ctrl Pts',(-2.19633755390064,1.55513205657248,11.4616427476261));
#4488=CARTESIAN_POINT('Ctrl Pts',(-2.44752205661339,0.369091202994485,11.5231002919432));
#4489=CARTESIAN_POINT('Ctrl Pts',(-2.44662748352118,0.00066590285712469,
11.542172503788));
#4490=CARTESIAN_POINT('',(-2.45049897433078,-0.00224205347296723,12.3421725236924));
#4491=CARTESIAN_POINT('Ctrl Pts',(-2.44662748352118,0.00066590285712469,
11.542172503788));
#4492=CARTESIAN_POINT('Ctrl Pts',(-2.44553399260474,-0.449682674129272,
11.5654856244154));
#4493=CARTESIAN_POINT('Ctrl Pts',(-2.11046030797052,-1.72031872164123,11.631184077515));
#4494=CARTESIAN_POINT('Ctrl Pts',(-0.066093817566476,-2.89669778952078,
11.7392678630871));
#4495=CARTESIAN_POINT('Ctrl Pts',(2.39963648265557,-1.62387537318686,11.8664238605037));
#4496=CARTESIAN_POINT('Ctrl Pts',(2.66447705535063,1.13832706110551,11.9935798579205));
#4497=CARTESIAN_POINT('Ctrl Pts',(0.485522402085563,2.85648288522925,12.1207358553373));
#4498=CARTESIAN_POINT('Ctrl Pts',(-1.91257980658966,2.03245349049535,12.2369334039597));
#4499=CARTESIAN_POINT('Ctrl Pts',(-2.44444428856106,0.602821897078908,12.31074562011));
#4500=CARTESIAN_POINT('Ctrl Pts',(-2.44987021777706,-0.00224109498362596,
12.342172503788));
#4501=CARTESIAN_POINT('',(-2.45083983812899,0.00049556074693392,13.1421725532727));
#4502=CARTESIAN_POINT('Ctrl Pts',(-2.45049897433078,-0.00224205347296723,
12.3421725236924));
#4503=CARTESIAN_POINT('Ctrl Pts',(-2.45040243216092,-0.107759825940935,
12.3476517447721));
#4504=CARTESIAN_POINT('Ctrl Pts',(-2.44348655931372,-0.212972878406652,
12.3531309658518));
#4505=CARTESIAN_POINT('Ctrl Pts',(-2.42989259424978,-0.317131251077622,
12.3586101869315));
#4506=CARTESIAN_POINT('Ctrl Pts',(-2.41629862918585,-0.421289623748593,
12.3640894080113));
#4507=CARTESIAN_POINT('Ctrl Pts',(-2.39602674807031,-0.524393675044689,
12.369568629091));
#4508=CARTESIAN_POINT('Ctrl Pts',(-2.36926728014896,-0.625717831946268,
12.3750478501708));
#4509=CARTESIAN_POINT('Ctrl Pts',(-2.34860534094121,-0.70395382588797,12.379278552111));
#4510=CARTESIAN_POINT('Ctrl Pts',(-2.32402521275318,-0.781312427764938,
12.3835092540513));
#4511=CARTESIAN_POINT('Ctrl Pts',(-2.29561824173242,-0.857372228513002,
12.3877399559916));
#4512=CARTESIAN_POINT('Ctrl Pts',(-2.26725208371266,-0.933322752255728,
12.3919645795773));
#4513=CARTESIAN_POINT('Ctrl Pts',(-2.23507016376243,-1.00797774891747,12.3961892031629));
#4514=CARTESIAN_POINT('Ctrl Pts',(-2.19921415187082,-1.08092893578214,12.4004138267486));
#4515=CARTESIAN_POINT('Ctrl Pts',(-2.1632170178103,-1.15416724408536,12.4046550776169));
#4516=CARTESIAN_POINT('Ctrl Pts',(-2.12351692995344,-1.22568784328583,12.4088963284852));
#4517=CARTESIAN_POINT('Ctrl Pts',(-2.08030689143503,-1.2950959375459,12.4131375793535));
#4518=CARTESIAN_POINT('Ctrl Pts',(-2.03734392902606,-1.36410715454132,12.4173545786404));
#4519=CARTESIAN_POINT('Ctrl Pts',(-1.99091129526494,-1.4310295609814,12.4215715779274));
#4520=CARTESIAN_POINT('Ctrl Pts',(-1.94124479636664,-1.49549954549624,12.4257885772143));
#4521=CARTESIAN_POINT('Ctrl Pts',(-1.89159476299925,-1.55994815680082,12.4300041784738));
#4522=CARTESIAN_POINT('Ctrl Pts',(-1.83871327709118,-1.62194559260165,12.4342197797332));
#4523=CARTESIAN_POINT('Ctrl Pts',(-1.78287825230524,-1.68115894175923,12.4384353809926));
#4524=CARTESIAN_POINT('Ctrl Pts',(-1.7270446207474,-1.74037081339079,12.4426508770619));
#4525=CARTESIAN_POINT('Ctrl Pts',(-1.66825791668527,-1.79679839888931,12.4468663731312));
#4526=CARTESIAN_POINT('Ctrl Pts',(-1.60683396932452,-1.85014454706242,12.4510818692005));
#4527=CARTESIAN_POINT('Ctrl Pts',(-1.54475915341902,-1.9040559687375,12.4553420340661));
#4528=CARTESIAN_POINT('Ctrl Pts',(-1.47999122643177,-1.95481993054753,12.4596021989316));
#4529=CARTESIAN_POINT('Ctrl Pts',(-1.41289018521115,-2.00217171454748,12.4638623637972));
#4530=CARTESIAN_POINT('Ctrl Pts',(-1.34639601786583,-2.04909524050351,12.4680839989661));
#4531=CARTESIAN_POINT('Ctrl Pts',(-1.27761119900921,-2.09266786159513,12.4723056341351));
#4532=CARTESIAN_POINT('Ctrl Pts',(-1.20691333802504,-2.13267682607967,12.476527269304));
#4533=CARTESIAN_POINT('Ctrl Pts',(-1.13524761730405,-2.17323351669478,12.4808066990179));
#4534=CARTESIAN_POINT('Ctrl Pts',(-1.06161652068031,-2.21012801679272,12.4850861287318));
#4535=CARTESIAN_POINT('Ctrl Pts',(-0.986435236874027,-2.24318875118731,
12.4893655584457));
#4536=CARTESIAN_POINT('Ctrl Pts',(-0.911253953067751,-2.2762494855819,12.4936449881596));
#4537=CARTESIAN_POINT('Ctrl Pts',(-0.834522963846906,-2.30547634084911,
12.4979244178735));
#4538=CARTESIAN_POINT('Ctrl Pts',(-0.756672398389139,-2.33075033659035,
12.5022038475874));
#4539=CARTESIAN_POINT('Ctrl Pts',(-0.679708279253695,-2.35573654970029,
12.5064345495276));
#4540=CARTESIAN_POINT('Ctrl Pts',(-0.601360480166753,-2.37695348549062,
12.5106652514679));
#4541=CARTESIAN_POINT('Ctrl Pts',(-0.52203275985569,-2.39424978806253,12.5148959534081));
#4542=CARTESIAN_POINT('Ctrl Pts',(-0.442819011651081,-2.41152124060684,
12.5191205769938));
#4543=CARTESIAN_POINT('Ctrl Pts',(-0.362628588873684,-2.424883148893,12.5233452005795));
#4544=CARTESIAN_POINT('Ctrl Pts',(-0.281881460098961,-2.43423357393092,
12.5275698241652));
#4545=CARTESIAN_POINT('Ctrl Pts',(-0.200816526600817,-2.44362080039184,
12.5318110750334));
#4546=CARTESIAN_POINT('Ctrl Pts',(-0.119190946900967,-2.4489647525341,12.5360523259017));
#4547=CARTESIAN_POINT('Ctrl Pts',(-0.0374411427535529,-2.4502139520518,
12.54029357677));
#4548=CARTESIAN_POINT('Ctrl Pts',(0.0438412139152897,-2.45145600861459,
12.544510576057));
#4549=CARTESIAN_POINT('Ctrl Pts',(0.125245908568908,-2.448650006106,12.5487275753439));
#4550=CARTESIAN_POINT('Ctrl Pts',(0.20633956393436,-2.44179733687204,12.5529445746309));
#4551=CARTESIAN_POINT('Ctrl Pts',(0.287406334978989,-2.43494693944784,12.5571601758903));
#4552=CARTESIAN_POINT('Ctrl Pts',(0.368161808465367,-2.42405257853431,12.5613757771498));
#4553=CARTESIAN_POINT('Ctrl Pts',(0.448175621099132,-2.40916767009945,12.5655913784092));
#4554=CARTESIAN_POINT('Ctrl Pts',(0.528187437181607,-2.3942831330815,12.5698068744785));
#4555=CARTESIAN_POINT('Ctrl Pts',(0.607457172188748,-2.3754083326432,12.5740223705478));
#4556=CARTESIAN_POINT('Ctrl Pts',(0.685564000346674,-2.35264792338944,12.5782378666171));
#4557=CARTESIAN_POINT('Ctrl Pts',(0.764498474394502,-2.32964633728066,12.5824980314827));
#4558=CARTESIAN_POINT('Ctrl Pts',(0.842244780125857,-2.3026764257124,12.5867581963483));
#4559=CARTESIAN_POINT('Ctrl Pts',(0.918385447378562,-2.27189753731177,12.5910183612139));
#4560=CARTESIAN_POINT('Ctrl Pts',(0.993837484753712,-2.24139701870898,12.5952399963829));
#4561=CARTESIAN_POINT('Ctrl Pts',(1.0677124095195,-2.20715639802551,12.5994616315518));
#4562=CARTESIAN_POINT('Ctrl Pts',(1.13962690685403,-2.16937796687768,12.6036832667208));
#4563=CARTESIAN_POINT('Ctrl Pts',(1.21252591978051,-2.13108234579064,12.6079626964347));
#4564=CARTESIAN_POINT('Ctrl Pts',(1.28340999627542,-2.08915156679782,12.6122421261486));
#4565=CARTESIAN_POINT('Ctrl Pts',(1.35191009511859,-2.04384181010088,12.6165215558625));
#4566=CARTESIAN_POINT('Ctrl Pts',(1.42041019396175,-1.99853205340395,12.6208009855764));
#4567=CARTESIAN_POINT('Ctrl Pts',(1.48652595895617,-1.94984366264381,12.6250804152903));
#4568=CARTESIAN_POINT('Ctrl Pts',(1.54992447940436,-1.89807385476517,12.6293598450042));
#4569=CARTESIAN_POINT('Ctrl Pts',(1.61260111190023,-1.84689352437492,12.6335905469444));
#4570=CARTESIAN_POINT('Ctrl Pts',(1.6728578368507,-1.79250912326258,12.6378212488847));
#4571=CARTESIAN_POINT('Ctrl Pts',(1.7303488008871,-1.73517816873904,12.642051950825));
#4572=CARTESIAN_POINT('Ctrl Pts',(1.78775716622726,-1.67792958302209,12.6462765744106));
#4573=CARTESIAN_POINT('Ctrl Pts',(1.84240733600462,-1.61774317723492,12.6505011979963));
#4574=CARTESIAN_POINT('Ctrl Pts',(1.89398622828447,-1.55491685213994,12.654725821582));
#4575=CARTESIAN_POINT('Ctrl Pts',(1.94576812487967,-1.49184325505931,12.6589670724503));
#4576=CARTESIAN_POINT('Ctrl Pts',(1.99445414866907,-1.42610921385226,12.6632083233186));
#4577=CARTESIAN_POINT('Ctrl Pts',(2.03976473497199,-1.35805378242714,12.6674495741869));
#4578=CARTESIAN_POINT('Ctrl Pts',(2.08481623417936,-1.29038749370581,12.6716665734738));
#4579=CARTESIAN_POINT('Ctrl Pts',(2.12653053250305,-1.22042668126703,12.6758835727608));
#4580=CARTESIAN_POINT('Ctrl Pts',(2.16467416497889,-1.14853646414597,12.6801005720478));
#4581=CARTESIAN_POINT('Ctrl Pts',(2.20280515200609,-1.07667008020465,12.6843161733072));
#4582=CARTESIAN_POINT('Ctrl Pts',(2.23736760612099,-1.00287597228756,12.6885317745666));
#4583=CARTESIAN_POINT('Ctrl Pts',(2.26817343341471,-0.927544891609961,12.6927473758261));
#4584=CARTESIAN_POINT('Ctrl Pts',(2.29897849202349,-0.852215690637342,12.6969628718954));
#4585=CARTESIAN_POINT('Ctrl Pts',(2.32602693515753,-0.775350024025249,12.7011783679647));
#4586=CARTESIAN_POINT('Ctrl Pts',(2.34917891190397,-0.697358365451837,12.705393864034));
#4587=CARTESIAN_POINT('Ctrl Pts',(2.37257621468461,-0.618540281363785,12.7096540288995));
#4588=CARTESIAN_POINT('Ctrl Pts',(2.39199382957925,-0.538572660312077,12.7139141937651));
#4589=CARTESIAN_POINT('Ctrl Pts',(2.40733970685362,-0.457892766710644,12.7181743586307));
#4590=CARTESIAN_POINT('Ctrl Pts',(2.42254679325618,-0.377942556565532,12.7223959937997));
#4591=CARTESIAN_POINT('Ctrl Pts',(2.43375549324763,-0.297293380137965,12.7266176289686));
#4592=CARTESIAN_POINT('Ctrl Pts',(2.44092835384074,-0.216377035325659,12.7308392641376));
#4593=CARTESIAN_POINT('Ctrl Pts',(2.44819941150613,-0.134352938863017,12.7351186938515));
#4594=CARTESIAN_POINT('Ctrl Pts',(2.45132327236096,-0.0520547978097172,
12.7393981235654));
#4595=CARTESIAN_POINT('Ctrl Pts',(2.45031551854859,0.030068414656077,12.7436775532793));
#4596=CARTESIAN_POINT('Ctrl Pts',(2.44930776473623,0.112191627121871,12.7479569829932));
#4597=CARTESIAN_POINT('Ctrl Pts',(2.44416849232609,0.194139425473585,12.752236412707));
#4598=CARTESIAN_POINT('Ctrl Pts',(2.43496734690495,0.275470995762991,12.7565158424209));
#4599=CARTESIAN_POINT('Ctrl Pts',(2.42587097042763,0.355876483230287,12.7607465443612));
#4600=CARTESIAN_POINT('Ctrl Pts',(2.41277058077403,0.435982137069594,12.7649772463014));
#4601=CARTESIAN_POINT('Ctrl Pts',(2.39569543844962,0.515357755536542,12.7692079482417));
#4602=CARTESIAN_POINT('Ctrl Pts',(2.37864482840639,0.594619333080539,12.7734325718274));
#4603=CARTESIAN_POINT('Ctrl Pts',(2.35763090428529,0.673152507543908,12.777657195413));
#4604=CARTESIAN_POINT('Ctrl Pts',(2.3327346221251,0.750532765932898,12.7818818189987));
#4605=CARTESIAN_POINT('Ctrl Pts',(2.30774035312392,0.828217577709613,12.786123069867));
#4606=CARTESIAN_POINT('Ctrl Pts',(2.2788331534967,0.904739907101411,12.7903643207353));
#4607=CARTESIAN_POINT('Ctrl Pts',(2.24614672573761,0.979681140197254,12.7946055716036));
#4608=CARTESIAN_POINT('Ctrl Pts',(2.2136471998115,1.05419385739856,12.7988225708905));
#4609=CARTESIAN_POINT('Ctrl Pts',(2.17741173571577,1.12714308017367,12.8030395701775));
#4610=CARTESIAN_POINT('Ctrl Pts',(2.13762090932871,1.19813484132659,12.8072565694644));
#4611=CARTESIAN_POINT('Ctrl Pts',(2.0978432744711,1.2691030671576,12.8114721707239));
#4612=CARTESIAN_POINT('Ctrl Pts',(2.05451284518539,1.3381147146936,12.8156877719833));
#4613=CARTESIAN_POINT('Ctrl Pts',(2.0078563122249,1.40480008522873,12.8199033732427));
#4614=CARTESIAN_POINT('Ctrl Pts',(1.96120094346539,1.47148379179165,12.824118869312));
#4615=CARTESIAN_POINT('Ctrl Pts',(1.91121990354004,1.53584095633197,12.8283343653813));
#4616=CARTESIAN_POINT('Ctrl Pts',(1.85818258434079,1.59753176283058,12.8325498614506));
#4617=CARTESIAN_POINT('Ctrl Pts',(1.80458326409398,1.65987626560194,12.8368100263162));
#4618=CARTESIAN_POINT('Ctrl Pts',(1.74786281183033,1.71949718877392,12.8410701911818));
#4619=CARTESIAN_POINT('Ctrl Pts',(1.68833902407878,1.7760804007062,12.8453303560474));
#4620=CARTESIAN_POINT('Ctrl Pts',(1.62935358016044,1.83215186390142,12.8495519912163));
#4621=CARTESIAN_POINT('Ctrl Pts',(1.56761570131212,1.88524008226713,12.8537736263853));
#4622=CARTESIAN_POINT('Ctrl Pts',(1.50346814737377,1.93507978642548,12.8579952615543));
#4623=CARTESIAN_POINT('Ctrl Pts',(1.43844240795988,1.98560180037758,12.8622746912682));
#4624=CARTESIAN_POINT('Ctrl Pts',(1.37094092201193,2.03278539839958,12.8665541209821));
#4625=CARTESIAN_POINT('Ctrl Pts',(1.30134960346411,2.07640060189834,12.870833550696));
#4626=CARTESIAN_POINT('Ctrl Pts',(1.2317582849163,2.1200158053971,12.8751129804098));
#4627=CARTESIAN_POINT('Ctrl Pts',(1.16007759399185,2.16006243227386,12.8793924101237));
#4628=CARTESIAN_POINT('Ctrl Pts',(1.08671585527975,2.19636037568601,12.8836718398376));
#4629=CARTESIAN_POINT('Ctrl Pts',(1.01418945081465,2.23224501216514,12.8879025417779));
#4630=CARTESIAN_POINT('Ctrl Pts',(0.939747313560946,2.26460091096586,12.8921332437181));
#4631=CARTESIAN_POINT('Ctrl Pts',(0.863766980855926,2.29321975675752,12.8963639456584));
#4632=CARTESIAN_POINT('Ctrl Pts',(0.787895810982456,2.32179748514247,12.9005885692441));
#4633=CARTESIAN_POINT('Ctrl Pts',(0.710491266285847,2.34664866134351,12.9048131928298));
#4634=CARTESIAN_POINT('Ctrl Pts',(0.63195408981764,2.36761151339546,12.9090378164154));
#4635=CARTESIAN_POINT('Ctrl Pts',(0.553107806561057,2.3886568710857,12.9132790672837));
#4636=CARTESIAN_POINT('Ctrl Pts',(0.473120382119683,2.40578302118053,12.917520318152));
#4637=CARTESIAN_POINT('Ctrl Pts',(0.392416157402715,2.41887573252726,12.9217615690203));
#4638=CARTESIAN_POINT('Ctrl Pts',(0.312173401514297,2.43189357941443,12.9259785683072));
#4639=CARTESIAN_POINT('Ctrl Pts',(0.231222484144265,2.44092391377575,12.9301955675942));
#4640=CARTESIAN_POINT('Ctrl Pts',(0.149992402096151,2.44590525763232,12.9344125668812));
#4641=CARTESIAN_POINT('Ctrl Pts',(0.0687892495973066,2.45088495006443,12.9386281681406));
#4642=CARTESIAN_POINT('Ctrl Pts',(-0.0126924199720212,2.45181828918592,
12.9428437694));
#4643=CARTESIAN_POINT('Ctrl Pts',(-0.0940190465842783,2.44869570769407,
12.9470593706595));
#4644=CARTESIAN_POINT('Ctrl Pts',(-0.175343643887187,2.4455732041187,12.9512748667288));
#4645=CARTESIAN_POINT('Ctrl Pts',(-0.256512741248561,2.43839500007924,12.9554903627981));
#4646=CARTESIAN_POINT('Ctrl Pts',(-0.337094783832249,2.42720360841712,12.9597058588674));
#4647=CARTESIAN_POINT('Ctrl Pts',(-0.418530700499861,2.41589362905237,12.9639660237329));
#4648=CARTESIAN_POINT('Ctrl Pts',(-0.499366564978021,2.40048495620425,12.9682261885985));
#4649=CARTESIAN_POINT('Ctrl Pts',(-0.579166209921358,2.38107470510384,12.9724863534641));
#4650=CARTESIAN_POINT('Ctrl Pts',(-0.658244132535397,2.36184000380251,12.9767079886331));
#4651=CARTESIAN_POINT('Ctrl Pts',(-0.736304070493699,2.33867600803559,12.980929623802));
#4652=CARTESIAN_POINT('Ctrl Pts',(-0.812937422333354,2.31172727573345,12.985151258971));
#4653=CARTESIAN_POINT('Ctrl Pts',(-0.890619891284911,2.28440961299145,12.9894306886849));
#4654=CARTESIAN_POINT('Ctrl Pts',(-0.966835960430611,2.2532029897929,12.9937101183988));
#4655=CARTESIAN_POINT('Ctrl Pts',(-1.04118333516246,2.21830735304646,12.9979895481127));
#4656=CARTESIAN_POINT('Ctrl Pts',(-1.1155307098943,2.18341171630001,13.0022689778266));
#4657=CARTESIAN_POINT('Ctrl Pts',(-1.18800898794108,2.1448273543514,13.0065484075405));
#4658=CARTESIAN_POINT('Ctrl Pts',(-1.25824567135025,2.1028000571924,13.0108278372544));
#4659=CARTESIAN_POINT('Ctrl Pts',(-1.32768260398911,2.06125130431604,13.0150585391946));
#4660=CARTESIAN_POINT('Ctrl Pts',(-1.39518992430448,2.01618138430343,13.0192892411349));
#4661=CARTESIAN_POINT('Ctrl Pts',(-1.46038808642804,1.96779493012332,13.0235199430751));
#4662=CARTESIAN_POINT('Ctrl Pts',(-1.52549257673233,1.91947799396403,13.0277445666608));
#4663=CARTESIAN_POINT('Ctrl Pts',(-1.58829412754736,1.86785426188777,13.0319691902465));
#4664=CARTESIAN_POINT('Ctrl Pts',(-1.64843976084091,1.81317307637158,13.0361938138322));
#4665=CARTESIAN_POINT('Ctrl Pts',(-1.70882211544763,1.75827667652755,13.0404350647005));
#4666=CARTESIAN_POINT('Ctrl Pts',(-1.76652719414015,1.70029894822673,13.0446763155687));
#4667=CARTESIAN_POINT('Ctrl Pts',(-1.8212292130223,1.63953481318152,13.048917566437));
#4668=CARTESIAN_POINT('Ctrl Pts',(-1.87561844435633,1.57911812902027,13.053134565724));
#4669=CARTESIAN_POINT('Ctrl Pts',(-1.92703855155145,1.51594716624645,13.0573515650109));
#4670=CARTESIAN_POINT('Ctrl Pts',(-1.97520558258288,1.45034932224393,13.0615685642979));
#4671=CARTESIAN_POINT('Ctrl Pts',(-2.02335664518979,1.38477322536175,13.0657841655573));
#4672=CARTESIAN_POINT('Ctrl Pts',(-2.06825649825139,1.31677221953997,13.0699997668168));
#4673=CARTESIAN_POINT('Ctrl Pts',(-2.10966236345087,1.2467056437824,13.0742153680762));
#4674=CARTESIAN_POINT('Ctrl Pts',(-2.15106719546708,1.17664081636685,13.0784308641455));
#4675=CARTESIAN_POINT('Ctrl Pts',(-2.1889779772965,1.10451092242006,13.0826463602148));
#4676=CARTESIAN_POINT('Ctrl Pts',(-2.22319680302972,1.03070181187308,13.0868618562841));
#4677=CARTESIAN_POINT('Ctrl Pts',(-2.25777822280421,0.956110595479309,13.0911220211497));
#4678=CARTESIAN_POINT('Ctrl Pts',(-2.28858875983413,0.87980479627115,13.0953821860153));
#4679=CARTESIAN_POINT('Ctrl Pts',(-2.3154739183128,0.802203704562095,13.0996423508809));
#4680=CARTESIAN_POINT('Ctrl Pts',(-2.34211592258677,0.725304451071835,13.1038639860498));
#4681=CARTESIAN_POINT('Ctrl Pts',(-2.3649031940265,0.647133709267337,13.1080856212188));
#4682=CARTESIAN_POINT('Ctrl Pts',(-2.38373604912697,0.568113279278458,13.1123072563877));
#4683=CARTESIAN_POINT('Ctrl Pts',(-2.40282672761737,0.488011052874501,13.1165866861016));
#4684=CARTESIAN_POINT('Ctrl Pts',(-2.41785380712066,0.407036183877513,13.1208661158155));
#4685=CARTESIAN_POINT('Ctrl Pts',(-2.42876758743796,0.325635158130646,13.1251455455294));
#4686=CARTESIAN_POINT('Ctrl Pts',(-2.43968136775527,0.244234132383773,13.1294249752433));
#4687=CARTESIAN_POINT('Ctrl Pts',(-2.44648187352101,0.162407444213362,13.1337044049572));
#4688=CARTESIAN_POINT('Ctrl Pts',(-2.4491740797156,0.0806013476886166,13.1379838346711));
#4689=CARTESIAN_POINT('Ctrl Pts',(-2.45005244916337,0.0539109790339228,
13.13938005771));
#4690=CARTESIAN_POINT('Ctrl Pts',(-2.4504945386623,0.0272061736954524,13.140776280749));
#4691=CARTESIAN_POINT('Ctrl Pts',(-2.45049994971379,0.00049644004570383,
13.142172503788));
#4692=CARTESIAN_POINT('',(-2.45049921122159,0.00196616437485418,13.942172503788));
#4693=CARTESIAN_POINT('Ctrl Pts',(-2.45441644957311,0.000486307974839832,
13.1421730739958));
#4694=CARTESIAN_POINT('Ctrl Pts',(-2.4522381490858,-0.784885048141428,13.1831619933598));
#4695=CARTESIAN_POINT('Ctrl Pts',(-1.61768875870369,-2.38635259292605,13.2665362451961));
#4696=CARTESIAN_POINT('Ctrl Pts',(1.11139908544534,-2.67582109816901,13.3922958295045));
#4697=CARTESIAN_POINT('Ctrl Pts',(2.8514413495468,-0.514304099370272,13.5194518269214));
#4698=CARTESIAN_POINT('Ctrl Pts',(1.97620916677945,2.11892043401155,13.646607824338));
#4699=CARTESIAN_POINT('Ctrl Pts',(-0.711555241617889,2.80872134870322,13.7737638217548));
#4700=CARTESIAN_POINT('Ctrl Pts',(-2.2883966915673,1.34721062141272,13.8722850888502));
#4701=CARTESIAN_POINT('Ctrl Pts',(-2.45037336834511,0.267128840959013,13.9284210234732));
#4702=CARTESIAN_POINT('Ctrl Pts',(-2.44838630074066,0.00198140226147181,
13.9421716256242));
#4703=CARTESIAN_POINT('',(-2.45049957242558,-0.00144759872526646,14.742172503788));
#4704=CARTESIAN_POINT('Ctrl Pts',(-2.45049921122159,0.00196616437485418,
13.942172503788));
#4705=CARTESIAN_POINT('Ctrl Pts',(-2.45056435292043,-0.079222206062589,
13.9463793468358));
#4706=CARTESIAN_POINT('Ctrl Pts',(-2.44659036857388,-0.160464817053646,
13.9505861898836));
#4707=CARTESIAN_POINT('Ctrl Pts',(-2.43858777176843,-0.241329503752571,
13.9547930329314));
#4708=CARTESIAN_POINT('Ctrl Pts',(-2.43058695487124,-0.322176204824231,
13.9589989403086));
#4709=CARTESIAN_POINT('Ctrl Pts',(-2.41855935099307,-0.402644684116547,
13.9632048476858));
#4710=CARTESIAN_POINT('Ctrl Pts',(-2.40256742063332,-0.482306996954589,
13.9674107550629));
#4711=CARTESIAN_POINT('Ctrl Pts',(-2.38657409952595,-0.561976237672478,
13.9716170282093));
#4712=CARTESIAN_POINT('Ctrl Pts',(-2.36661586067399,-0.640838715262248,
13.9758233013557));
#4713=CARTESIAN_POINT('Ctrl Pts',(-2.34280616296429,-0.718477231912426,
13.9800295745021));
#4714=CARTESIAN_POINT('Ctrl Pts',(-2.3189701885327,-0.796201431536588,13.9842404897515));
#4715=CARTESIAN_POINT('Ctrl Pts',(-2.2912744051616,-0.872698525713307,13.9884514050009));
#4716=CARTESIAN_POINT('Ctrl Pts',(-2.25988184464756,-0.947567569217272,
13.9926623202503));
#4717=CARTESIAN_POINT('Ctrl Pts',(-2.2284715477322,-1.02247891278789,13.9968756146138));
#4718=CARTESIAN_POINT('Ctrl Pts',(-2.19336051763534,-1.09575995335298,14.0010889089773));
#4719=CARTESIAN_POINT('Ctrl Pts',(-2.15475843919274,-1.16703312666252,14.0053022033408));
#4720=CARTESIAN_POINT('Ctrl Pts',(-2.11608554479169,-1.2384370514311,14.0095232270414));
#4721=CARTESIAN_POINT('Ctrl Pts',(-2.07390905318627,-1.30782535253099,14.0137442507421));
#4722=CARTESIAN_POINT('Ctrl Pts',(-2.02848263731509,-1.37484851533222,14.0179652744427));
#4723=CARTESIAN_POINT('Ctrl Pts',(-1.99221294503478,-1.42836164076451,14.0213354551579));
#4724=CARTESIAN_POINT('Ctrl Pts',(-1.95387236655151,-1.4803675466113,14.0247056358731));
#4725=CARTESIAN_POINT('Ctrl Pts',(-1.91360765035879,-1.53070441643327,14.0280758165883));
#4726=CARTESIAN_POINT('Ctrl Pts',(-1.8630619890676,-1.59389399314112,14.0323065185285));
#4727=CARTESIAN_POINT('Ctrl Pts',(-1.80928801626886,-1.6546960970155,14.0365372204688));
#4728=CARTESIAN_POINT('Ctrl Pts',(-1.75253974839791,-1.71276229532454,14.040767922409));
#4729=CARTESIAN_POINT('Ctrl Pts',(-1.69587301217313,-1.77074506848401,14.0449925459947));
#4730=CARTESIAN_POINT('Ctrl Pts',(-1.6362407900663,-1.82599941297279,14.0492171695804));
#4731=CARTESIAN_POINT('Ctrl Pts',(-1.57393781039641,-1.87820925857705,14.0534417931661));
#4732=CARTESIAN_POINT('Ctrl Pts',(-1.51138961852498,-1.93062459180406,14.0576830440344));
#4733=CARTESIAN_POINT('Ctrl Pts',(-1.44614989728259,-1.97997103907282,14.0619242949027));
#4734=CARTESIAN_POINT('Ctrl Pts',(-1.37855486404845,-2.02596563070758,14.0661655457709));
#4735=CARTESIAN_POINT('Ctrl Pts',(-1.31134634094944,-2.07169722408673,14.0703825450579));
#4736=CARTESIAN_POINT('Ctrl Pts',(-1.24180975659261,-2.11411492555338,14.0745995443449));
#4737=CARTESIAN_POINT('Ctrl Pts',(-1.17030785705411,-2.15298159994864,14.0788165436318));
#4738=CARTESIAN_POINT('Ctrl Pts',(-1.09882966195957,-2.19183538919105,14.0830321448912));
#4739=CARTESIAN_POINT('Ctrl Pts',(-1.02538785381415,-2.22714026723997,14.0872477461507));
#4740=CARTESIAN_POINT('Ctrl Pts',(-0.950371267117993,-2.25870420919529,
14.0914633474101));
#4741=CARTESIAN_POINT('Ctrl Pts',(-0.875356552279458,-2.29026736354873,
14.0956788434794));
#4742=CARTESIAN_POINT('Ctrl Pts',(-0.798767566099872,-2.31808958804037,
14.0998943395487));
#4743=CARTESIAN_POINT('Ctrl Pts',(-0.721013351049024,-2.34202689942047,
14.104109835618));
#4744=CARTESIAN_POINT('Ctrl Pts',(-0.642435226513823,-2.36621785850138,
14.1083700004835));
#4745=CARTESIAN_POINT('Ctrl Pts',(-0.562667490049711,-2.38644092464532,
14.1126301653491));
#4746=CARTESIAN_POINT('Ctrl Pts',(-0.482146455553999,-2.40259964317751,
14.1168903302147));
#4747=CARTESIAN_POINT('Ctrl Pts',(-0.402353667764279,-2.4186122193555,14.1211119653837));
#4748=CARTESIAN_POINT('Ctrl Pts',(-0.321821627248609,-2.43063366121305,
14.1253336005526));
#4749=CARTESIAN_POINT('Ctrl Pts',(-0.240981732250492,-2.43862216317361,
14.1295552357216));
#4750=CARTESIAN_POINT('Ctrl Pts',(-0.159035132206545,-2.44672002840622,
14.1338346654355));
#4751=CARTESIAN_POINT('Ctrl Pts',(-0.0767726788328666,-2.45067367133576,
14.1381140951494));
#4752=CARTESIAN_POINT('Ctrl Pts',(0.00535652038376576,-2.45049414561418,
14.1423935248633));
#4753=CARTESIAN_POINT('Ctrl Pts',(0.0874857196003865,-2.45031461989261,
14.1466729545772));
#4754=CARTESIAN_POINT('Ctrl Pts',(0.169481178189257,-2.44600201668813,14.1509523842911));
#4755=CARTESIAN_POINT('Ctrl Pts',(0.250901402272344,-2.43762153262925,14.1552318140049));
#4756=CARTESIAN_POINT('Ctrl Pts',(0.331394534075985,-2.42933647304453,14.1594625159452));
#4757=CARTESIAN_POINT('Ctrl Pts',(0.411628226228095,-2.41704458019804,14.1636932178855));
#4758=CARTESIAN_POINT('Ctrl Pts',(0.491172003780826,-2.40077077471006,14.1679239198257));
#4759=CARTESIAN_POINT('Ctrl Pts',(0.570601498812235,-2.38452035020271,14.1721485434114));
#4760=CARTESIAN_POINT('Ctrl Pts',(0.649342596099766,-2.36429946752609,14.1763731669971));
#4761=CARTESIAN_POINT('Ctrl Pts',(0.726969987829958,-2.34018479757358,14.1805977905828));
#4762=CARTESIAN_POINT('Ctrl Pts',(0.804902905615784,-2.31597521705111,14.1848390414511));
#4763=CARTESIAN_POINT('Ctrl Pts',(0.881712860331415,-2.28784118174837,14.1890802923193));
#4764=CARTESIAN_POINT('Ctrl Pts',(0.956979911021107,-2.25591216582163,14.1933215431876));
#4765=CARTESIAN_POINT('Ctrl Pts',(1.03181658278293,-2.22416572082754,14.1975385424746));
#4766=CARTESIAN_POINT('Ctrl Pts',(1.10512751493307,-2.1886677604776,14.2017555417616));
#4767=CARTESIAN_POINT('Ctrl Pts',(1.17651693927987,-2.14959487848002,14.2059725410485));
#4768=CARTESIAN_POINT('Ctrl Pts',(1.24788269647073,-2.11053494999761,14.210188142308));
#4769=CARTESIAN_POINT('Ctrl Pts',(1.31732780324473,-2.06790267650819,14.2144037435674));
#4770=CARTESIAN_POINT('Ctrl Pts',(1.38448029361778,-2.02192100898725,14.2186193448268));
#4771=CARTESIAN_POINT('Ctrl Pts',(1.45163110836261,-1.97594048882778,14.2228348408961));
#4772=CARTESIAN_POINT('Ctrl Pts',(1.5164890373366,-1.92661100445113,14.2270503369654));
#4773=CARTESIAN_POINT('Ctrl Pts',(1.57871156510052,-1.87419850715389,14.2312658330347));
#4774=CARTESIAN_POINT('Ctrl Pts',(1.64159342343243,-1.82123062962935,14.2355259979003));
#4775=CARTESIAN_POINT('Ctrl Pts',(1.70178331591802,-1.76511431268457,14.2397861627659));
#4776=CARTESIAN_POINT('Ctrl Pts',(1.75896392205107,-1.70616416880753,14.2440463276315));
#4777=CARTESIAN_POINT('Ctrl Pts',(1.81562737650659,-1.64774718062538,14.2482679628004));
#4778=CARTESIAN_POINT('Ctrl Pts',(1.86933549494015,-1.58654781275061,14.2524895979694));
#4779=CARTESIAN_POINT('Ctrl Pts',(1.91981956487922,-1.52290613246745,14.2567112331384));
#4780=CARTESIAN_POINT('Ctrl Pts',(1.97099476603439,-1.45839319216223,14.2609906628523));
#4781=CARTESIAN_POINT('Ctrl Pts',(2.01885668784563,-1.39137096474464,14.2652700925662));
#4782=CARTESIAN_POINT('Ctrl Pts',(2.06317147164031,-1.32222302529095,14.2695495222801));
#4783=CARTESIAN_POINT('Ctrl Pts',(2.10748625543499,-1.25307508583727,14.273828951994));
#4784=CARTESIAN_POINT('Ctrl Pts',(2.14825371448245,-1.18180189271094,14.2781083817079));
#4785=CARTESIAN_POINT('Ctrl Pts',(2.1852896333229,-1.10880993343831,14.2823878114218));
#4786=CARTESIAN_POINT('Ctrl Pts',(2.22190384226498,-1.03664909791501,14.286618513362));
#4787=CARTESIAN_POINT('Ctrl Pts',(2.25500881229795,-0.962537041235813,14.2908492153023));
#4788=CARTESIAN_POINT('Ctrl Pts',(2.28439243138442,-0.886849180770644,14.2950799172425));
#4789=CARTESIAN_POINT('Ctrl Pts',(2.31373383429534,-0.811270062934999,14.2993045408282));
#4790=CARTESIAN_POINT('Ctrl Pts',(2.33936433793701,-0.734120067592675,14.3035291644139));
#4791=CARTESIAN_POINT('Ctrl Pts',(2.36111813725122,-0.65579828601737,14.3077537879995));
#4792=CARTESIAN_POINT('Ctrl Pts',(2.38295755521568,-0.57716824540526,14.3119950388678));
#4793=CARTESIAN_POINT('Ctrl Pts',(2.40088947279053,-0.497357598133571,14.3162362897361));
#4794=CARTESIAN_POINT('Ctrl Pts',(2.41479538533844,-0.416789511562107,14.3204775406044));
#4795=CARTESIAN_POINT('Ctrl Pts',(2.42862178352145,-0.336682115377783,14.3246945398914));
#4796=CARTESIAN_POINT('Ctrl Pts',(2.43846801344591,-0.255826381394331,14.3289115391783));
#4797=CARTESIAN_POINT('Ctrl Pts',(2.44426827401313,-0.174650664621922,14.3331285384653));
#4798=CARTESIAN_POINT('Ctrl Pts',(2.45006661166708,-0.0935018593754865,
14.3373441397247));
#4799=CARTESIAN_POINT('Ctrl Pts',(2.45182161049296,-0.0120337455097168,
14.3415597409841));
#4800=CARTESIAN_POINT('Ctrl Pts',(2.44951933141044,0.0693202354766672,14.3457753422436));
#4801=CARTESIAN_POINT('Ctrl Pts',(2.44721710977573,0.150672186471123,14.3499908383129));
#4802=CARTESIAN_POINT('Ctrl Pts',(2.44085782576217,0.231909545404855,14.3542063343822));
#4803=CARTESIAN_POINT('Ctrl Pts',(2.43047963800674,0.312600350663004,14.3584218304514));
#4804=CARTESIAN_POINT('Ctrl Pts',(2.41999147952733,0.394146182490494,14.362681995317));
#4805=CARTESIAN_POINT('Ctrl Pts',(2.40539878472013,0.475133326180942,14.3669421601826));
#4806=CARTESIAN_POINT('Ctrl Pts',(2.38679426532006,0.555124657203479,14.3712023250482));
#4807=CARTESIAN_POINT('Ctrl Pts',(2.36835800853678,0.634392532253334,14.3754239602172));
#4808=CARTESIAN_POINT('Ctrl Pts',(2.34598239116248,0.712682099636594,14.3796455953861));
#4809=CARTESIAN_POINT('Ctrl Pts',(2.31980784320882,0.789583320864148,14.3838672305551));
#4810=CARTESIAN_POINT('Ctrl Pts',(2.29327496346493,0.867537326358365,14.388146660269));
#4811=CARTESIAN_POINT('Ctrl Pts',(2.26283853301648,0.944064225087086,14.3924260899829));
#4812=CARTESIAN_POINT('Ctrl Pts',(2.22869443163873,1.01875972652167,14.3967055196968));
#4813=CARTESIAN_POINT('Ctrl Pts',(2.19455033026098,1.09345522795625,14.4009849494106));
#4814=CARTESIAN_POINT('Ctrl Pts',(2.15669884222827,1.1663189269381,14.4052643791245));
#4815=CARTESIAN_POINT('Ctrl Pts',(2.11538198855414,1.23697586577132,14.4095438088384));
#4816=CARTESIAN_POINT('Ctrl Pts',(2.07453558969008,1.30682826859122,14.4137745107787));
#4817=CARTESIAN_POINT('Ctrl Pts',(2.03014874344269,1.37478666664704,14.4180052127189));
#4818=CARTESIAN_POINT('Ctrl Pts',(1.98242224482019,1.4404694697362,14.4222359146592));
#4819=CARTESIAN_POINT('Ctrl Pts',(1.93476431604388,1.50605790471047,14.4264605382449));
#4820=CARTESIAN_POINT('Ctrl Pts',(1.88377653536069,1.56937686489836,14.4306851618305));
#4821=CARTESIAN_POINT('Ctrl Pts',(1.82970467293867,1.63007087570645,14.4349097854162));
#4822=CARTESIAN_POINT('Ctrl Pts',(1.77541999436405,1.69100376613302,14.4391510362845));
#4823=CARTESIAN_POINT('Ctrl Pts',(1.7180271448577,1.7492905906423,14.4433922871528));
#4824=CARTESIAN_POINT('Ctrl Pts',(1.65781774574636,1.80460260774732,14.4476335380211));
#4825=CARTESIAN_POINT('Ctrl Pts',(1.59795262552468,1.85959834931873,14.451850537308));
#4826=CARTESIAN_POINT('Ctrl Pts',(1.53530342442256,1.91165289343346,14.456067536595));
#4827=CARTESIAN_POINT('Ctrl Pts',(1.47019465964299,1.96047900084577,14.460284535882));
#4828=CARTESIAN_POINT('Ctrl Pts',(1.40510747984326,2.00928892133536,14.4645001371414));
#4829=CARTESIAN_POINT('Ctrl Pts',(1.33756272737892,2.05487225175629,14.4687157384008));
#4830=CARTESIAN_POINT('Ctrl Pts',(1.26791727466758,2.09698260235977,14.4729313396603));
#4831=CARTESIAN_POINT('Ctrl Pts',(1.19827355979026,2.13909190220117,14.4771468357296));
#4832=CARTESIAN_POINT('Ctrl Pts',(1.12652964741637,2.177728154827,14.4813623317989));
#4833=CARTESIAN_POINT('Ctrl Pts',(1.05306937206137,2.21268957326288,14.4855778278682));
#4834=CARTESIAN_POINT('Ctrl Pts',(0.978830687233028,2.24802145449896,14.4898379927337));
#4835=CARTESIAN_POINT('Ctrl Pts',(0.902839479066865,2.27959993556306,14.4940981575993));
#4836=CARTESIAN_POINT('Ctrl Pts',(0.825513458532294,2.3072663001444,14.4983583224649));
#4837=CARTESIAN_POINT('Ctrl Pts',(0.748886788423378,2.33468244515266,14.5025799576339));
#4838=CARTESIAN_POINT('Ctrl Pts',(0.670949821353555,2.35825687574795,14.5068015928028));
#4839=CARTESIAN_POINT('Ctrl Pts',(0.592123330739176,2.37788565982352,14.5110232279718));
#4840=CARTESIAN_POINT('Ctrl Pts',(0.512217698756271,2.39778316362446,14.5153026576857));
#4841=CARTESIAN_POINT('Ctrl Pts',(0.431398488927928,2.41362607529504,14.5195820873996));
#4842=CARTESIAN_POINT('Ctrl Pts',(0.350111663188402,2.42536019454832,14.5238615171135));
#4843=CARTESIAN_POINT('Ctrl Pts',(0.268824837448876,2.43709431380159,14.5281409468274));
#4844=CARTESIAN_POINT('Ctrl Pts',(0.187070890347798,2.44471966028567,14.5324203765413));
#4845=CARTESIAN_POINT('Ctrl Pts',(0.105296103432629,2.44823670844996,14.5366998062552));
#4846=CARTESIAN_POINT('Ctrl Pts',(0.0244524460306887,2.45171370970653,14.5409305081954));
#4847=CARTESIAN_POINT('Ctrl Pts',(-0.0567156527722998,2.45118861657421,
14.5451612101357));
#4848=CARTESIAN_POINT('Ctrl Pts',(-0.137778655346634,2.44662365151056,14.5493919120759));
#4849=CARTESIAN_POINT('Ctrl Pts',(-0.21872519269157,2.44206524504561,14.5536165356616));
#4850=CARTESIAN_POINT('Ctrl Pts',(-0.299566473305872,2.43347852000482,14.5578411592473));
#4851=CARTESIAN_POINT('Ctrl Pts',(-0.379870566370386,2.42087765134991,14.562065782833));
#4852=CARTESIAN_POINT('Ctrl Pts',(-0.460490720457274,2.40822718816901,14.5663070337013));
#4853=CARTESIAN_POINT('Ctrl Pts',(-0.540568975281024,2.39153089546031,14.5705482845696));
#4854=CARTESIAN_POINT('Ctrl Pts',(-0.61967105172237,2.37085597151267,14.5747895354379));
#4855=CARTESIAN_POINT('Ctrl Pts',(-0.698320820460222,2.35029926731085,14.5790065347248));
#4856=CARTESIAN_POINT('Ctrl Pts',(-0.776005089679829,2.3258094270183,14.5832235340118));
#4857=CARTESIAN_POINT('Ctrl Pts',(-0.85230666336635,2.29750377618434,14.5874405332987));
#4858=CARTESIAN_POINT('Ctrl Pts',(-0.928582941411809,2.26920750929294,14.5916561345582));
#4859=CARTESIAN_POINT('Ctrl Pts',(-1.00347699853749,2.23709810560857,14.5958717358176));
#4860=CARTESIAN_POINT('Ctrl Pts',(-1.07658846575391,2.20134220997228,14.600087337077));
#4861=CARTESIAN_POINT('Ctrl Pts',(-1.14969810865047,2.16558720653789,14.6043028331463));
#4862=CARTESIAN_POINT('Ctrl Pts',(-1.22102483277727,2.12618609735261,14.6085183292156));
#4863=CARTESIAN_POINT('Ctrl Pts',(-1.29019117166378,2.08335234431453,14.6127338252849));
#4864=CARTESIAN_POINT('Ctrl Pts',(-1.36009042004676,2.04006471060448,14.6169939901505));
#4865=CARTESIAN_POINT('Ctrl Pts',(-1.42778280589453,1.99327149439629,14.6212541550161));
#4866=CARTESIAN_POINT('Ctrl Pts',(-1.49290873360751,1.94323795843906,14.6255143198817));
#4867=CARTESIAN_POINT('Ctrl Pts',(-1.55744565072687,1.89365693477226,14.6297359550507));
#4868=CARTESIAN_POINT('Ctrl Pts',(-1.61946202784922,1.8408943193843,14.6339575902196));
#4869=CARTESIAN_POINT('Ctrl Pts',(-1.67864267156163,1.78524761061664,14.6381792253886));
#4870=CARTESIAN_POINT('Ctrl Pts',(-1.73863350332548,1.72883909366784,14.6424586551025));
#4871=CARTESIAN_POINT('Ctrl Pts',(-1.79571002812112,1.66946727506073,14.6467380848164));
#4872=CARTESIAN_POINT('Ctrl Pts',(-1.84958522757528,1.60747775596906,14.6510175145303));
#4873=CARTESIAN_POINT('Ctrl Pts',(-1.90346042702943,1.54548823687739,14.6552969442442));
#4874=CARTESIAN_POINT('Ctrl Pts',(-1.95413404990639,1.4808814437352,14.659576373958));
#4875=CARTESIAN_POINT('Ctrl Pts',(-2.00136487298638,1.41403284798345,14.6638558036719));
#4876=CARTESIAN_POINT('Ctrl Pts',(-2.04854588977583,1.34725474603989,14.6681307206015));
#4877=CARTESIAN_POINT('Ctrl Pts',(-2.09246741364618,1.27799073561833,14.672405637531));
#4878=CARTESIAN_POINT('Ctrl Pts',(-2.13286079451428,1.20658819869245,14.6766805544605));
#4879=CARTESIAN_POINT('Ctrl Pts',(-2.17319329701726,1.13529327518295,14.6809490285039));
#4880=CARTESIAN_POINT('Ctrl Pts',(-2.21000799855832,1.06186661759444,14.6852175025473));
#4881=CARTESIAN_POINT('Ctrl Pts',(-2.24307855145289,0.986685797005316,14.6894859765907));
#4882=CARTESIAN_POINT('Ctrl Pts',(-2.27709485655393,0.909354954093206,14.6938765205238));
#4883=CARTESIAN_POINT('Ctrl Pts',(-2.30714929978574,0.830168471242125,14.6982670644569));
#4884=CARTESIAN_POINT('Ctrl Pts',(-2.33304538151732,0.749566206402557,14.70265760839));
#4885=CARTESIAN_POINT('Ctrl Pts',(-2.35816409428244,0.671383523797928,14.7069163535191));
#4886=CARTESIAN_POINT('Ctrl Pts',(-2.37937041262091,0.591869318872894,14.7111750986483));
#4887=CARTESIAN_POINT('Ctrl Pts',(-2.39653373568161,0.511445308649865,14.7154338437774));
#4888=CARTESIAN_POINT('Ctrl Pts',(-2.41449380944567,0.427287878827075,14.7198902871125));
#4889=CARTESIAN_POINT('Ctrl Pts',(-2.4280262260801,0.342134607466912,14.7243467304476));
#4890=CARTESIAN_POINT('Ctrl Pts',(-2.4370404068577,0.256484512871338,14.7288031737827));
#4891=CARTESIAN_POINT('Ctrl Pts',(-2.4460545876353,0.170834418275776,14.7332596171178));
#4892=CARTESIAN_POINT('Ctrl Pts',(-2.45055045587725,0.0846880646948334,
14.7377160604529));
#4893=CARTESIAN_POINT('Ctrl Pts',(-2.45049957242558,-0.00144759872526646,
14.742172503788));
#4894=CARTESIAN_POINT('',(-2.45049965096235,-0.00130791185444283,15.542172503788));
#4895=CARTESIAN_POINT('Ctrl Pts',(-2.44733426487298,-0.00146391714831885,
14.7421734460211));
#4896=CARTESIAN_POINT('Ctrl Pts',(-2.44901793535173,-0.315713367656626,
14.7584528977103));
#4897=CARTESIAN_POINT('Ctrl Pts',(-2.24674592747447,-1.44605616538801,14.8171176818718));
#4898=CARTESIAN_POINT('Ctrl Pts',(-0.543033491398334,-2.8461098193418,14.9181677985054));
#4899=CARTESIAN_POINT('Ctrl Pts',(2.09888347669716,-1.99747706564621,15.0453237959221));
#4900=CARTESIAN_POINT('Ctrl Pts',(2.81575424861743,0.683194326621678,15.1724797933388));
#4901=CARTESIAN_POINT('Ctrl Pts',(0.950081937109875,2.7372560693716,15.2996357907557));
#4902=CARTESIAN_POINT('Ctrl Pts',(-1.70248634147458,2.29486366106898,15.4228663208472));
#4903=CARTESIAN_POINT('Ctrl Pts',(-2.44889900543195,0.736220053860236,15.5037115184667));
#4904=CARTESIAN_POINT('Ctrl Pts',(-2.45367050467139,-0.00128812380637844,
15.5421713836139));
#4905=CARTESIAN_POINT('',(-2.45049903536358,0.00217432338375172,16.3421725038319));
#4906=CARTESIAN_POINT('Ctrl Pts',(-2.45049965096235,-0.00130791185444283,
15.542172503788));
#4907=CARTESIAN_POINT('Ctrl Pts',(-2.45045953015348,-0.0764781366577363,
15.5460975977217));
#4908=CARTESIAN_POINT('Ctrl Pts',(-2.44696089914346,-0.151553924908697,
15.5500226916554));
#4909=CARTESIAN_POINT('Ctrl Pts',(-2.44002780973267,-0.226306291850654,
15.5539477855891));
#4910=CARTESIAN_POINT('Ctrl Pts',(-2.43255490963965,-0.306878881756149,
15.5581784875294));
#4911=CARTESIAN_POINT('Ctrl Pts',(-2.42107276369846,-0.387232452371849,
15.5624091894696));
#4912=CARTESIAN_POINT('Ctrl Pts',(-2.4056019501097,-0.466936299326177,15.5666398914099));
#4913=CARTESIAN_POINT('Ctrl Pts',(-2.39015336382314,-0.546525633783576,
15.5708645149956));
#4914=CARTESIAN_POINT('Ctrl Pts',(-2.3707275790756,-0.625466645844599,15.5750891385813));
#4915=CARTESIAN_POINT('Ctrl Pts',(-2.34739697381755,-0.703333276130331,
15.5793137621669));
#4916=CARTESIAN_POINT('Ctrl Pts',(-2.32397454391307,-0.781506374067252,
15.5835550130352));
#4917=CARTESIAN_POINT('Ctrl Pts',(-2.29661653419516,-0.858596142455209,
15.5877962639035));
#4918=CARTESIAN_POINT('Ctrl Pts',(-2.26544817731458,-0.934181356002161,
15.5920375147718));
#4919=CARTESIAN_POINT('Ctrl Pts',(-2.23445804189869,-1.00933437135788,15.5962545140588));
#4920=CARTESIAN_POINT('Ctrl Pts',(-2.19970119547367,-1.08299955708573,15.6004715133457));
#4921=CARTESIAN_POINT('Ctrl Pts',(-2.16135023161793,-1.1547793842484,15.6046885126327));
#4922=CARTESIAN_POINT('Ctrl Pts',(-2.12301198194574,-1.226535414828,15.6089041138921));
#4923=CARTESIAN_POINT('Ctrl Pts',(-2.08108219999881,-1.29640691820099,15.6131197151515));
#4924=CARTESIAN_POINT('Ctrl Pts',(-2.03578007430045,-1.36401969893446,15.617335316411));
#4925=CARTESIAN_POINT('Ctrl Pts',(-1.99047907900709,-1.43163079255447,15.6215508124803));
#4926=CARTESIAN_POINT('Ctrl Pts',(-1.94180616703827,-1.49698288984425,15.6257663085496));
#4927=CARTESIAN_POINT('Ctrl Pts',(-1.89002382204775,-1.55973081077858,15.6299818046189));
#4928=CARTESIAN_POINT('Ctrl Pts',(-1.83769277413322,-1.6231436295212,15.6342419694845));
#4929=CARTESIAN_POINT('Ctrl Pts',(-1.78218629959459,-1.68389636994626,15.63850213435));
#4930=CARTESIAN_POINT('Ctrl Pts',(-1.72381579488247,-1.74166855495347,15.6427622992156));
#4931=CARTESIAN_POINT('Ctrl Pts',(-1.66597320350443,-1.79891823793754,15.6469839343846));
#4932=CARTESIAN_POINT('Ctrl Pts',(-1.605318570642,-1.85324079426793,15.6512055695535));
#4933=CARTESIAN_POINT('Ctrl Pts',(-1.54218923643854,-1.90436409570573,15.6554272047225));
#4934=CARTESIAN_POINT('Ctrl Pts',(-1.47819565627453,-1.95618727949325,15.6597066344364));
#4935=CARTESIAN_POINT('Ctrl Pts',(-1.41165950361692,-2.00472265748693,15.6639860641503));
#4936=CARTESIAN_POINT('Ctrl Pts',(-1.34296197567411,-2.04973251471832,15.6682654938642));
#4937=CARTESIAN_POINT('Ctrl Pts',(-1.27426444773129,-2.09474237194971,15.6725449235781));
#4938=CARTESIAN_POINT('Ctrl Pts',(-1.20340600096031,-2.13622651707527,15.6768243532919));
#4939=CARTESIAN_POINT('Ctrl Pts',(-1.13079124448469,-2.17399664475288,15.6811037830058));
#4940=CARTESIAN_POINT('Ctrl Pts',(-1.05900331673451,-2.21133670245514,15.6853344849461));
#4941=CARTESIAN_POINT('Ctrl Pts',(-0.985228877902366,-2.24518737691081,
15.6895651868863));
#4942=CARTESIAN_POINT('Ctrl Pts',(-0.909841187210448,-2.27533278094776,
15.6937958888266));
#4943=CARTESIAN_POINT('Ctrl Pts',(-0.834561807886533,-2.30543487433386,
15.6980205124123));
#4944=CARTESIAN_POINT('Ctrl Pts',(-0.757674208132242,-2.33184209876761,
15.7022451359979));
#4945=CARTESIAN_POINT('Ctrl Pts',(-0.679575786855455,-2.35438463296034,
15.7064697595836));
#4946=CARTESIAN_POINT('Ctrl Pts',(-0.601169985643965,-2.3770158901077,15.7107110104519));
#4947=CARTESIAN_POINT('Ctrl Pts',(-0.521544232367028,-2.39575175146806,
15.7149522613202));
#4948=CARTESIAN_POINT('Ctrl Pts',(-0.441120477798487,-2.4104694509715,15.7191935121885));
#4949=CARTESIAN_POINT('Ctrl Pts',(-0.361156588322953,-2.42510299429139,
15.7234105114754));
#4950=CARTESIAN_POINT('Ctrl Pts',(-0.280404260837503,-2.43576411840727,
15.7276275107624));
#4951=CARTESIAN_POINT('Ctrl Pts',(-0.199291164994801,-2.44238270579265,
15.7318445100494));
#4952=CARTESIAN_POINT('Ctrl Pts',(-0.1182049599179,-2.44899909897151,15.7360601113088));
#4953=CARTESIAN_POINT('Ctrl Pts',(-0.0367586871468292,-2.45157557901659,
15.7402757125682));
#4954=CARTESIAN_POINT('Ctrl Pts',(0.0446143744299721,-2.45009383648754,
15.7444913138277));
#4955=CARTESIAN_POINT('Ctrl Pts',(0.125985405538724,-2.44861213093179,15.748706809897));
#4956=CARTESIAN_POINT('Ctrl Pts',(0.207282764121698,-2.44307241368985,15.7529223059663));
#4957=CARTESIAN_POINT('Ctrl Pts',(0.28807412571626,-2.4335084853135,15.7571378020355));
#4958=CARTESIAN_POINT('Ctrl Pts',(0.36972157940851,-2.42384321437596,15.7613979669011));
#4959=CARTESIAN_POINT('Ctrl Pts',(0.450851765835281,-2.41006798170178,15.7656581317667));
#4960=CARTESIAN_POINT('Ctrl Pts',(0.531026647736233,-2.39227108610082,15.7699182966323));
#4961=CARTESIAN_POINT('Ctrl Pts',(0.610476413597396,-2.37463514882189,15.7741399318013));
#4962=CARTESIAN_POINT('Ctrl Pts',(0.688987648276002,-2.35305018546353,15.7783615669702));
#4963=CARTESIAN_POINT('Ctrl Pts',(0.766148917958076,-2.32765248383681,15.7825832021392));
#4964=CARTESIAN_POINT('Ctrl Pts',(0.844366531992265,-2.30190708551224,15.7868626318531));
#4965=CARTESIAN_POINT('Ctrl Pts',(0.921196477439546,-2.27224394323022,15.791142061567));
#4966=CARTESIAN_POINT('Ctrl Pts',(0.996232508967404,-2.23885484971146,15.7954214912809));
#4967=CARTESIAN_POINT('Ctrl Pts',(1.07126854049527,-2.20546575619269,15.7997009209948));
#4968=CARTESIAN_POINT('Ctrl Pts',(1.14451025009894,-2.1683509916112,15.8039803507086));
#4969=CARTESIAN_POINT('Ctrl Pts',(1.21558025847274,-2.12774878338853,15.8082597804225));
#4970=CARTESIAN_POINT('Ctrl Pts',(1.28584102741231,-2.08760889265761,15.8124904823628));
#4971=CARTESIAN_POINT('Ctrl Pts',(1.35424359176949,-2.04390963436344,15.816721184303));
#4972=CARTESIAN_POINT('Ctrl Pts',(1.42040435581549,-1.99684794513263,15.8209518862433));
#4973=CARTESIAN_POINT('Ctrl Pts',(1.48647006504817,-1.94985387059987,15.825176509829));
#4974=CARTESIAN_POINT('Ctrl Pts',(1.5502999950053,-1.89950722681971,15.8294011334147));
#4975=CARTESIAN_POINT('Ctrl Pts',(1.61153621068436,-1.84605018665612,15.8336257570003));
#4976=CARTESIAN_POINT('Ctrl Pts',(1.67301343999307,-1.79238275015864,15.8378670078686));
#4977=CARTESIAN_POINT('Ctrl Pts',(1.73187608248903,-1.73558061635869,15.8421082587369));
#4978=CARTESIAN_POINT('Ctrl Pts',(1.78779247252783,-1.67593207653915,15.8463495096052));
#4979=CARTESIAN_POINT('Ctrl Pts',(1.84338913121305,-1.61662460860143,15.8505665088921));
#4980=CARTESIAN_POINT('Ctrl Pts',(1.89607281824666,-1.55450354065931,15.8547835081791));
#4981=CARTESIAN_POINT('Ctrl Pts',(1.94555303637445,-1.48989047673115,15.859000507466));
#4982=CARTESIAN_POINT('Ctrl Pts',(1.99501685072745,-1.42529883344721,15.8632161087255));
#4983=CARTESIAN_POINT('Ctrl Pts',(2.04127902263602,-1.35821720371133,15.8674317099849));
#4984=CARTESIAN_POINT('Ctrl Pts',(2.08408957597741,-1.28899995706062,15.8716473112444));
#4985=CARTESIAN_POINT('Ctrl Pts',(2.12689906108494,-1.21978443755897,15.8758628073137));
#4986=CARTESIAN_POINT('Ctrl Pts',(2.16625685516059,-1.14843380318765,15.8800783033829));
#4987=CARTESIAN_POINT('Ctrl Pts',(2.20195731068694,-1.07532983401017,15.8842937994522));
#4988=CARTESIAN_POINT('Ctrl Pts',(2.23803606009593,-1.00145123089796,15.8885539643178));
#4989=CARTESIAN_POINT('Ctrl Pts',(2.27037927363017,-0.925782342157913,15.8928141291834));
#4990=CARTESIAN_POINT('Ctrl Pts',(2.29882403061643,-0.848739256933737,15.897074294049));
#4991=CARTESIAN_POINT('Ctrl Pts',(2.3270115281088,-0.772392963217447,15.901295929218));
#4992=CARTESIAN_POINT('Ctrl Pts',(2.35137072031579,-0.694697697152131,15.9055175643869));
#4993=CARTESIAN_POINT('Ctrl Pts',(2.37179343709891,-0.616073162647547,15.9097391995559));
#4994=CARTESIAN_POINT('Ctrl Pts',(2.39249574261377,-0.536372251570763,15.9140186292698));
#4995=CARTESIAN_POINT('Ctrl Pts',(2.40915287521122,-0.455716920307952,15.9182980589837));
#4996=CARTESIAN_POINT('Ctrl Pts',(2.42170614002846,-0.374552561529669,15.9225774886976));
#4997=CARTESIAN_POINT('Ctrl Pts',(2.43425940484571,-0.293388202751386,15.9268569184115));
#4998=CARTESIAN_POINT('Ctrl Pts',(2.44270881654254,-0.211715311180257,15.9311363481254));
#4999=CARTESIAN_POINT('Ctrl Pts',(2.44705034898912,-0.129980150454718,15.9354157778393));
#5000=CARTESIAN_POINT('Ctrl Pts',(2.45134244652861,-0.0491756680383044,
15.9396464797795));
#5001=CARTESIAN_POINT('Ctrl Pts',(2.45163592503804,0.0319935986607728,15.9438771817198));
#5002=CARTESIAN_POINT('Ctrl Pts',(2.44788867719599,0.113098514825096,15.94810788366));
#5003=CARTESIAN_POINT('Ctrl Pts',(2.44414681311801,0.194086905541516,15.9523325072457));
#5004=CARTESIAN_POINT('Ctrl Pts',(2.43637577383797,0.275010668718802,15.9565571308314));
#5005=CARTESIAN_POINT('Ctrl Pts',(2.42458537776252,0.355437752553385,15.9607817544171));
#5006=CARTESIAN_POINT('Ctrl Pts',(2.41274857702078,0.436181381477818,15.9650230052854));
#5007=CARTESIAN_POINT('Ctrl Pts',(2.39686068766559,0.516423939124441,15.9692642561537));
#5008=CARTESIAN_POINT('Ctrl Pts',(2.3769845250529,0.595730490791806,15.9735055070219));
#5009=CARTESIAN_POINT('Ctrl Pts',(2.35722201484823,0.674583565561007,15.9777225063089));
#5010=CARTESIAN_POINT('Ctrl Pts',(2.33351683191251,0.752510853873331,15.9819395055959));
#5011=CARTESIAN_POINT('Ctrl Pts',(2.30598208858882,0.829093997751474,15.9861565048828));
#5012=CARTESIAN_POINT('Ctrl Pts',(2.27845647363493,0.905651752642007,15.9903721061423));
#5013=CARTESIAN_POINT('Ctrl Pts',(2.24710397669182,0.980865810723941,15.9945877074017));
#5014=CARTESIAN_POINT('Ctrl Pts',(2.21208719657955,1.05433414282609,15.9988033086611));
#5015=CARTESIAN_POINT('Ctrl Pts',(2.17707129022638,1.12780064170363,16.0030188047304));
#5016=CARTESIAN_POINT('Ctrl Pts',(2.13839148356906,1.19952108186293,16.0072343007997));
#5017=CARTESIAN_POINT('Ctrl Pts',(2.096257421066,1.26911586335753,16.011449796869));
#5018=CARTESIAN_POINT('Ctrl Pts',(2.05367689204424,1.33944809426877,16.0157099617346));
#5019=CARTESIAN_POINT('Ctrl Pts',(2.00756870353708,1.40760892713825,16.0199701266002));
#5020=CARTESIAN_POINT('Ctrl Pts',(1.95819447843981,1.4732361095927,16.0242302914658));
#5021=CARTESIAN_POINT('Ctrl Pts',(1.90926680270716,1.53826974801543,16.0284519266347));
#5022=CARTESIAN_POINT('Ctrl Pts',(1.85713227849037,1.60081505957935,16.0326735618037));
#5023=CARTESIAN_POINT('Ctrl Pts',(1.8020852104146,1.66055386675801,16.0368951969727));
#5024=CARTESIAN_POINT('Ctrl Pts',(1.74628454328966,1.72111050329365,16.0411746266866));
#5025=CARTESIAN_POINT('Ctrl Pts',(1.68749133567476,1.77878286466226,16.0454540564005));
#5026=CARTESIAN_POINT('Ctrl Pts',(1.62604827671431,1.83328046184822,16.0497334861144));
#5027=CARTESIAN_POINT('Ctrl Pts',(1.56460521775387,1.88777805903417,16.0540129158283));
#5028=CARTESIAN_POINT('Ctrl Pts',(1.50051273132664,1.93910063651412,16.0582923455422));
#5029=CARTESIAN_POINT('Ctrl Pts',(1.4341438371495,1.98700319686862,16.062571775256));
#5030=CARTESIAN_POINT('Ctrl Pts',(1.36853065311792,2.0343603141913,16.0668024771963));
#5031=CARTESIAN_POINT('Ctrl Pts',(1.30044587424408,2.07855306101479,16.0710331791366));
#5032=CARTESIAN_POINT('Ctrl Pts',(1.23022750145147,2.11931369661796,16.0752638810768));
#5033=CARTESIAN_POINT('Ctrl Pts',(1.16011001313948,2.16001577040334,16.0794885046625));
#5034=CARTESIAN_POINT('Ctrl Pts',(1.08786541773138,2.19729529471072,16.0837131282482));
#5035=CARTESIAN_POINT('Ctrl Pts',(1.01386228183302,2.23092660647462,16.0879377518338));
#5036=CARTESIAN_POINT('Ctrl Pts',(0.939567884232938,2.26469028442781,16.0921790027021));
#5037=CARTESIAN_POINT('Ctrl Pts',(0.863501458712895,2.29477669322709,16.0964202535704));
#5038=CARTESIAN_POINT('Ctrl Pts',(0.786062688873,2.32100316655574,16.1006615044387));
#5039=CARTESIAN_POINT('Ctrl Pts',(0.709066715906823,2.34707967623668,16.1048785037257));
#5040=CARTESIAN_POINT('Ctrl Pts',(0.630714495145698,2.36934012240313,16.1090955030126));
#5041=CARTESIAN_POINT('Ctrl Pts',(0.551419004568888,2.38765310114352,16.1133125022996));
#5042=CARTESIAN_POINT('Ctrl Pts',(0.472149802181945,2.40596000873082,16.117528103559));
#5043=CARTESIAN_POINT('Ctrl Pts',(0.391938403751546,2.42032194312575,16.1217437048184));
#5044=CARTESIAN_POINT('Ctrl Pts',(0.311210851255252,2.43065794715361,16.1259593060779));
#5045=CARTESIAN_POINT('Ctrl Pts',(0.230485313119831,2.44099369327148,16.1301748021472));
#5046=CARTESIAN_POINT('Ctrl Pts',(0.14924410795852,2.44730365077037,16.1343902982165));
#5047=CARTESIAN_POINT('Ctrl Pts',(0.067919891275365,2.44955855989791,16.1386057942858));
#5048=CARTESIAN_POINT('Ctrl Pts',(-0.01426606381486,2.45183736279141,16.1428659591514));
#5049=CARTESIAN_POINT('Ctrl Pts',(-0.0965363163016381,2.44997463881073,
16.1471261240169));
#5050=CARTESIAN_POINT('Ctrl Pts',(-0.178444654042102,2.44399422164697,16.1513862888825));
#5051=CARTESIAN_POINT('Ctrl Pts',(-0.259612198056688,2.43806789245076,16.1556079240515));
#5052=CARTESIAN_POINT('Ctrl Pts',(-0.340423888304079,2.42809817162709,16.1598295592204));
#5053=CARTESIAN_POINT('Ctrl Pts',(-0.420452874624735,2.41416023292154,16.1640511943894));
#5054=CARTESIAN_POINT('Ctrl Pts',(-0.501577464582437,2.40003148264833,16.1683306241033));
#5055=CARTESIAN_POINT('Ctrl Pts',(-0.581897275367252,2.38182515070137,16.1726100538172));
#5056=CARTESIAN_POINT('Ctrl Pts',(-0.660982540191496,2.35967208136258,16.1768894835311));
#5057=CARTESIAN_POINT('Ctrl Pts',(-0.740067805015739,2.33751901202378,16.181168913245));
#5058=CARTESIAN_POINT('Ctrl Pts',(-0.817918079553251,2.31141942332903,16.1854483429589));
#5059=CARTESIAN_POINT('Ctrl Pts',(-0.894125423086832,2.28155428990629,16.1897277726728));
#5060=CARTESIAN_POINT('Ctrl Pts',(-0.969465030862757,2.25202921615465,16.193958474613));
#5061=CARTESIAN_POINT('Ctrl Pts',(-1.04348232106309,2.2187129027707,16.1981891765533));
#5062=CARTESIAN_POINT('Ctrl Pts',(-1.11576919095822,2.18174456857544,16.2024198784935));
#5063=CARTESIAN_POINT('Ctrl Pts',(-1.18795220451158,2.14482934770431,16.2066445020792));
#5064=CARTESIAN_POINT('Ctrl Pts',(-1.2584093248239,2.10427273670739,16.2108691256649));
#5065=CARTESIAN_POINT('Ctrl Pts',(-1.32675127764859,2.06026243407432,16.2150937492506));
#5066=CARTESIAN_POINT('Ctrl Pts',(-1.39536221087849,2.0160789155973,16.2193350001188));
#5067=CARTESIAN_POINT('Ctrl Pts',(-1.46184084931117,1.96841463423303,16.2235762509871));
#5068=CARTESIAN_POINT('Ctrl Pts',(-1.52581722143071,1.91750672926732,16.2278175018554));
#5069=CARTESIAN_POINT('Ctrl Pts',(-1.58942777501225,1.86688991700897,16.2320345011424));
#5070=CARTESIAN_POINT('Ctrl Pts',(-1.65056423310857,1.81306676722036,16.2362515004293));
#5071=CARTESIAN_POINT('Ctrl Pts',(-1.70889252572214,1.75631335061002,16.2404684997163));
#5072=CARTESIAN_POINT('Ctrl Pts',(-1.76720148123065,1.6995787489989,16.2446841009757));
#5073=CARTESIAN_POINT('Ctrl Pts',(-1.82270378694915,1.63991613375578,16.2488997022352));
#5074=CARTESIAN_POINT('Ctrl Pts',(-1.87510071335025,1.577639871705,16.2531153034946));
#5075=CARTESIAN_POINT('Ctrl Pts',(-1.92749633231272,1.51536516360779,16.2573307995639));
#5076=CARTESIAN_POINT('Ctrl Pts',(-1.97678642744433,1.45047729492956,16.2615462956332));
#5077=CARTESIAN_POINT('Ctrl Pts',(-2.02271215357283,1.38332418246366,16.2657617917025));
#5078=CARTESIAN_POINT('Ctrl Pts',(-2.06912452394702,1.31545949331697,16.2700219565681));
#5079=CARTESIAN_POINT('Ctrl Pts',(-2.11210051405406,1.24528165878786,16.2742821214337));
#5080=CARTESIAN_POINT('Ctrl Pts',(-2.15141857770886,1.17317873893502,16.2785422862993));
#5081=CARTESIAN_POINT('Ctrl Pts',(-2.19038104173026,1.1017279308467,16.2827639214682));
#5082=CARTESIAN_POINT('Ctrl Pts',(-2.22575133037719,1.02838716936328,16.2869855566372));
#5083=CARTESIAN_POINT('Ctrl Pts',(-2.25736154480874,0.95355603192402,16.2912071918062));
#5084=CARTESIAN_POINT('Ctrl Pts',(-2.28940450576747,0.877700449841354,16.29548662152));
#5085=CARTESIAN_POINT('Ctrl Pts',(-2.31758349228026,0.800313840879615,16.2997660512339));
#5086=CARTESIAN_POINT('Ctrl Pts',(-2.34177583183142,0.721828375342958,16.3040454809478));
#5087=CARTESIAN_POINT('Ctrl Pts',(-2.36596817138258,0.643342909806301,16.3083249106617));
#5088=CARTESIAN_POINT('Ctrl Pts',(-2.38617380672396,0.563759079312502,16.3126043403756));
#5089=CARTESIAN_POINT('Ctrl Pts',(-2.40232402969856,0.483517844895977,16.3168837700895));
#5090=CARTESIAN_POINT('Ctrl Pts',(-2.42528233781664,0.36945112356297,16.3229671824421));
#5091=CARTESIAN_POINT('Ctrl Pts',(-2.44012249745587,0.253699812650627,16.3290505947948));
#5092=CARTESIAN_POINT('Ctrl Pts',(-2.44665526989177,0.137216035181218,16.3351340071474));
#5093=CARTESIAN_POINT('Ctrl Pts',(-2.44917473836213,0.0922921980931879,
16.3374801726943));
#5094=CARTESIAN_POINT('Ctrl Pts',(-2.45045903119538,0.0472596765101275,
16.3398263382411));
#5095=CARTESIAN_POINT('Ctrl Pts',(-2.45049903536283,0.00217432422689355,
16.342172503788));
#5096=CARTESIAN_POINT('',(-2.45049999653667,0.000130283472662122,17.1421725037616));
#5097=CARTESIAN_POINT('Ctrl Pts',(-2.45049903536358,0.00217432338375008,
16.3421725038319));
#5098=CARTESIAN_POINT('Ctrl Pts',(-2.45057140723682,-0.079389995380578,
16.3464169731516));
#5099=CARTESIAN_POINT('Ctrl Pts',(-2.4465669366815,-0.161087169591855,16.3506614424714));
#5100=CARTESIAN_POINT('Ctrl Pts',(-2.43847466509943,-0.242469704640073,
16.3549059117912));
#5101=CARTESIAN_POINT('Ctrl Pts',(-2.43054759010119,-0.322190887046028,
16.359063734015));
#5102=CARTESIAN_POINT('Ctrl Pts',(-2.41869807736869,-0.40160965200395,16.3632215562389));
#5103=CARTESIAN_POINT('Ctrl Pts',(-2.40296835781613,-0.480305445872146,
16.3673793784627));
#5104=CARTESIAN_POINT('Ctrl Pts',(-2.38724644125933,-0.558962201349099,
16.3715351381279));
#5105=CARTESIAN_POINT('Ctrl Pts',(-2.36764823010998,-0.636896227556718,
16.3756908977931));
#5106=CARTESIAN_POINT('Ctrl Pts',(-2.3442674440548,-0.713694893315605,16.3798466574583));
#5107=CARTESIAN_POINT('Ctrl Pts',(-2.32089060445962,-0.790480596171468,
16.3840017156698));
#5108=CARTESIAN_POINT('Ctrl Pts',(-2.29373259783578,-0.866130860355851,
16.3881567738813));
#5109=CARTESIAN_POINT('Ctrl Pts',(-2.26293718669726,-0.940247594552993,
16.3923118320928));
#5110=CARTESIAN_POINT('Ctrl Pts',(-2.23098851599837,-1.01713993164474,16.3966224933773));
#5111=CARTESIAN_POINT('Ctrl Pts',(-2.19512480414509,-1.09238108773953,16.4009331546617));
#5112=CARTESIAN_POINT('Ctrl Pts',(-2.15556071890026,-1.16555061543211,16.4052438159462));
#5113=CARTESIAN_POINT('Ctrl Pts',(-2.11737709415858,-1.23616712964319,16.4094040706786));
#5114=CARTESIAN_POINT('Ctrl Pts',(-2.07574736520893,-1.3048538028626,16.413564325411));
#5115=CARTESIAN_POINT('Ctrl Pts',(-2.03090962191084,-1.37126086417937,16.4177245801435));
#5116=CARTESIAN_POINT('Ctrl Pts',(-1.98604163029081,-1.4377127248554,16.4218876414561));
#5117=CARTESIAN_POINT('Ctrl Pts',(-1.93796161023166,-1.50188153438697,16.4260507027688));
#5118=CARTESIAN_POINT('Ctrl Pts',(-1.88694812386883,-1.56345035988607,16.4302137640815));
#5119=CARTESIAN_POINT('Ctrl Pts',(-1.83585604644397,-1.6251140379375,16.4343832389807));
#5120=CARTESIAN_POINT('Ctrl Pts',(-1.78182181869666,-1.68416939772259,16.4385527138799));
#5121=CARTESIAN_POINT('Ctrl Pts',(-1.72516030602611,-1.7403367974366,16.4427221887792));
#5122=CARTESIAN_POINT('Ctrl Pts',(-1.71919184832307,-1.7462532076008,16.4431613816882));
#5123=CARTESIAN_POINT('Ctrl Pts',(-1.7131942684475,-1.75213761220032,16.4436005745972));
#5124=CARTESIAN_POINT('Ctrl Pts',(-1.70716795431106,-1.75798971150954,16.4440397675063));
#5125=CARTESIAN_POINT('Ctrl Pts',(-1.64911706508823,-1.8143624064984,16.4482704694465));
#5126=CARTESIAN_POINT('Ctrl Pts',(-1.58816176517468,-1.86796266208124,16.4525011713868));
#5127=CARTESIAN_POINT('Ctrl Pts',(-1.52459764933984,-1.91847654601963,16.456731873327));
#5128=CARTESIAN_POINT('Ctrl Pts',(-1.46112485764922,-1.96891785540615,16.4609564969127));
#5129=CARTESIAN_POINT('Ctrl Pts',(-1.3950510550735,-2.01628131296009,16.4651811204984));
#5130=CARTESIAN_POINT('Ctrl Pts',(-1.32670818167509,-2.06029018603603,16.4694057440841));
#5131=CARTESIAN_POINT('Ctrl Pts',(-1.25809632424838,-2.10447226932939,16.4736469949524));
#5132=CARTESIAN_POINT('Ctrl Pts',(-1.18719783690718,-2.14527297494293,16.4778882458206));
#5133=CARTESIAN_POINT('Ctrl Pts',(-1.11438168379159,-2.18245359923867,16.4821294966889));
#5134=CARTESIAN_POINT('Ctrl Pts',(-1.0419818953087,-2.21942162377026,16.4863464959759));
#5135=CARTESIAN_POINT('Ctrl Pts',(-0.967686730419196,-2.25281064046376,
16.4905634952628));
#5136=CARTESIAN_POINT('Ctrl Pts',(-0.891885742000532,-2.28243073787928,
16.4947804945498));
#5137=CARTESIAN_POINT('Ctrl Pts',(-0.816109883267823,-2.31204101558451,
16.4989960958092));
#5138=CARTESIAN_POINT('Ctrl Pts',(-0.7388296251798,-2.33788468613573,16.5032116970686));
#5139=CARTESIAN_POINT('Ctrl Pts',(-0.660454763104563,-2.3598198566612,16.5074272983281));
#5140=CARTESIAN_POINT('Ctrl Pts',(-0.582081856684622,-2.3817544798475,16.5116427943974));
#5141=CARTESIAN_POINT('Ctrl Pts',(-0.502614848726326,-2.39978067261866,
16.5158582904666));
#5142=CARTESIAN_POINT('Ctrl Pts',(-0.422477576217387,-2.41380673368716,
16.5200737865359));
#5143=CARTESIAN_POINT('Ctrl Pts',(-0.341491142555745,-2.42798141955673,
16.5243339514015));
#5144=CARTESIAN_POINT('Ctrl Pts',(-0.259820629509927,-2.43807059611939,
16.5285941162671));
#5145=CARTESIAN_POINT('Ctrl Pts',(-0.177910987859338,-2.44403312792583,
16.5328542811327));
#5146=CARTESIAN_POINT('Ctrl Pts',(-0.0967421517275273,-2.44994173352311,
16.5370759163016));
#5147=CARTESIAN_POINT('Ctrl Pts',(-0.0153389665501788,-2.45179808934016,
16.5412975514706));
#5148=CARTESIAN_POINT('Ctrl Pts',(0.065865327957158,-2.44961466532455,16.5455191866396));
#5149=CARTESIAN_POINT('Ctrl Pts',(0.148181316170854,-2.44740135004825,16.5497986163535));
#5150=CARTESIAN_POINT('Ctrl Pts',(0.230292433647624,-2.4410368458092,16.5540780460674));
#5151=CARTESIAN_POINT('Ctrl Pts',(0.311754480613395,-2.43058828142848,16.5583574757813));
#5152=CARTESIAN_POINT('Ctrl Pts',(0.393216527579153,-2.42013971704777,16.5626369054952));
#5153=CARTESIAN_POINT('Ctrl Pts',(0.474029032782728,-2.40560724381223,16.5669163352091));
#5154=CARTESIAN_POINT('Ctrl Pts',(0.553762120998581,-2.38711075640557,16.571195764923));
#5155=CARTESIAN_POINT('Ctrl Pts',(0.63258732752593,-2.36882487945679,16.5754264668632));
#5156=CARTESIAN_POINT('Ctrl Pts',(0.710654067120473,-2.34659606583185,16.5796571688035));
#5157=CARTESIAN_POINT('Ctrl Pts',(0.787538360381103,-2.32050287242404,16.5838878707437));
#5158=CARTESIAN_POINT('Ctrl Pts',(0.864312192067739,-2.29444716775538,16.5881124943294));
#5159=CARTESIAN_POINT('Ctrl Pts',(0.939906514777329,-2.26453825817382,16.5923371179151));
#5160=CARTESIAN_POINT('Ctrl Pts',(1.01390894717427,-2.23090539845148,16.5965617415008));
#5161=CARTESIAN_POINT('Ctrl Pts',(1.08820263850401,-2.19714016644742,16.6008029923691));
#5162=CARTESIAN_POINT('Ctrl Pts',(1.16089141963541,-2.15962171520719,16.6050442432373));
#5163=CARTESIAN_POINT('Ctrl Pts',(1.2315748371327,-2.11853101712992,16.6092854941056));
#5164=CARTESIAN_POINT('Ctrl Pts',(1.30185408503437,-2.07767527671902,16.6135024933926));
#5165=CARTESIAN_POINT('Ctrl Pts',(1.37015043441123,-2.0332882670932,16.6177194926796));
#5166=CARTESIAN_POINT('Ctrl Pts',(1.4360933072488,-1.98559468746147,16.6219364919665));
#5167=CARTESIAN_POINT('Ctrl Pts',(1.50201431858144,-1.93791691929474,16.626152093226));
#5168=CARTESIAN_POINT('Ctrl Pts',(1.56558302624584,-1.88693503031828,16.6303676944854));
#5169=CARTESIAN_POINT('Ctrl Pts',(1.62645826467569,-1.83291673658902,16.6345832957448));
#5170=CARTESIAN_POINT('Ctrl Pts',(1.6873319841111,-1.77889979075573,16.6387987918141));
#5171=CARTESIAN_POINT('Ctrl Pts',(1.74551202080585,-1.72184690029531,16.6430142878834));
#5172=CARTESIAN_POINT('Ctrl Pts',(1.80069180584647,-1.66206476118032,16.6472297839527));
#5173=CARTESIAN_POINT('Ctrl Pts',(1.85645629421417,-1.60164915066606,16.6514899488183));
#5174=CARTESIAN_POINT('Ctrl Pts',(1.90915622857922,-1.53844645212566,16.6557501136839));
#5175=CARTESIAN_POINT('Ctrl Pts',(1.95851612238009,-1.47280849005471,16.6600102785495));
#5176=CARTESIAN_POINT('Ctrl Pts',(2.00742959643125,-1.40776416950815,16.6642319137185));
#5177=CARTESIAN_POINT('Ctrl Pts',(2.05306299034396,-1.34032888220273,16.6684535488874));
#5178=CARTESIAN_POINT('Ctrl Pts',(2.0951922272061,-1.2708736290659,16.6726751840564));
#5179=CARTESIAN_POINT('Ctrl Pts',(2.13789821690804,-1.20046752759977,16.6769546137703));
#5180=CARTESIAN_POINT('Ctrl Pts',(2.17700314381611,-1.12798616986567,16.6812340434842));
#5181=CARTESIAN_POINT('Ctrl Pts',(2.21232295197177,-1.05383936450435,16.6855134731981));
#5182=CARTESIAN_POINT('Ctrl Pts',(2.24764276012743,-0.979692559143013,16.689792902912));
#5183=CARTESIAN_POINT('Ctrl Pts',(2.27917732158527,-0.903880784270916,16.6940723326259));
#5184=CARTESIAN_POINT('Ctrl Pts',(2.30679469916295,-0.82683037311997,16.6983517623398));
#5185=CARTESIAN_POINT('Ctrl Pts',(2.33409761116627,-0.750657297325339,16.70258246428));
#5186=CARTESIAN_POINT('Ctrl Pts',(2.35767482651374,-0.672987155684143,16.7068131662203));
#5187=CARTESIAN_POINT('Ctrl Pts',(2.37736284503395,-0.594218943700109,16.7110438681605));
#5188=CARTESIAN_POINT('Ctrl Pts',(2.39702257728888,-0.515563899962941,16.7152684917462));
#5189=CARTESIAN_POINT('Ctrl Pts',(2.41280409839237,-0.435814366485038,16.7194931153319));
#5190=CARTESIAN_POINT('Ctrl Pts',(2.42459281212612,-0.355387036041509,16.7237177389176));
#5191=CARTESIAN_POINT('Ctrl Pts',(2.43642792390476,-0.274643159537652,16.7279589897859));
#5192=CARTESIAN_POINT('Ctrl Pts',(2.44423857098117,-0.193216586000028,16.7322002406541));
#5193=CARTESIAN_POINT('Ctrl Pts',(2.44796009702729,-0.11154198026814,16.7364414915224));
#5194=CARTESIAN_POINT('Ctrl Pts',(2.45166034329195,-0.0303343920283068,
16.7406584908094));
#5195=CARTESIAN_POINT('Ctrl Pts',(2.45131808364671,0.0511179303453776,16.7448754900963));
#5196=CARTESIAN_POINT('Ctrl Pts',(2.44692160031486,0.13238176578573,16.7490924893833));
#5197=CARTESIAN_POINT('Ctrl Pts',(2.44252657451343,0.213618660486784,16.7533080906427));
#5198=CARTESIAN_POINT('Ctrl Pts',(2.4340800192118,0.294666728330832,16.7575236919022));
#5199=CARTESIAN_POINT('Ctrl Pts',(2.42162230761968,0.375094187156699,16.7617392931616));
#5200=CARTESIAN_POINT('Ctrl Pts',(2.40916490687963,0.455519639109805,16.7659547892309));
#5201=CARTESIAN_POINT('Ctrl Pts',(2.39269662110847,0.535324053420373,16.7701702853002));
#5202=CARTESIAN_POINT('Ctrl Pts',(2.37230932721088,0.614083631135268,16.7743857813695));
#5203=CARTESIAN_POINT('Ctrl Pts',(2.35170600277669,0.693677771491064,16.7786459462351));
#5204=CARTESIAN_POINT('Ctrl Pts',(2.32710022727606,0.772204327488877,16.7829061111006));
#5205=CARTESIAN_POINT('Ctrl Pts',(2.29863864811251,0.849241199779836,16.7871662759662));
#5206=CARTESIAN_POINT('Ctrl Pts',(2.27043448058559,0.925581336753914,16.7913879111352));
#5207=CARTESIAN_POINT('Ctrl Pts',(2.23844421552458,1.0004582194032,16.7956095463041));
#5208=CARTESIAN_POINT('Ctrl Pts',(2.20285845685558,1.07348258908092,16.7998311814731));
#5209=CARTESIAN_POINT('Ctrl Pts',(2.16678552612036,1.14750666859735,16.804110611187));
#5210=CARTESIAN_POINT('Ctrl Pts',(2.12701815000923,1.21962669580686,16.8083900409009));
#5211=CARTESIAN_POINT('Ctrl Pts',(2.08380122814352,1.28946604902478,16.8126694706148));
#5212=CARTESIAN_POINT('Ctrl Pts',(2.04058430627781,1.35930540224269,16.8169489003287));
#5213=CARTESIAN_POINT('Ctrl Pts',(1.99391817136637,1.42686371504001,16.8212283300425));
#5214=CARTESIAN_POINT('Ctrl Pts',(1.94408983392776,1.49179923837584,16.8255077597564));
#5215=CARTESIAN_POINT('Ctrl Pts',(1.89482886740289,1.55599537265911,16.8297384616967));
#5216=CARTESIAN_POINT('Ctrl Pts',(1.84229209519928,1.61786962863473,16.8339691636369));
#5217=CARTESIAN_POINT('Ctrl Pts',(1.78672645485866,1.67706852141116,16.8381998655772));
#5218=CARTESIAN_POINT('Ctrl Pts',(1.73124064705382,1.73618236166778,16.8424244891629));
#5219=CARTESIAN_POINT('Ctrl Pts',(1.67273492930515,1.7926281364344,16.8466491127486));
#5220=CARTESIAN_POINT('Ctrl Pts',(1.61149759544796,1.84608389567361,16.8508737363343));
#5221=CARTESIAN_POINT('Ctrl Pts',(1.55001924356036,1.89975004620509,16.8551149872025));
#5222=CARTESIAN_POINT('Ctrl Pts',(1.48578801614026,1.95040221802365,16.8593562380708));
#5223=CARTESIAN_POINT('Ctrl Pts',(1.4191343552195,1.99775071814172,16.8635974889391));
#5224=CARTESIAN_POINT('Ctrl Pts',(1.35286182164279,2.04482847832074,16.8678144882261));
#5225=CARTESIAN_POINT('Ctrl Pts',(1.28419486541293,2.08863997320343,16.872031487513));
#5226=CARTESIAN_POINT('Ctrl Pts',(1.21349137625816,2.128940799963,16.8762484868));
#5227=CARTESIAN_POINT('Ctrl Pts',(1.14281132685682,2.16922826611683,16.8804640880594));
#5228=CARTESIAN_POINT('Ctrl Pts',(1.0700964889884,2.20600714526631,16.8846796893189));
#5229=CARTESIAN_POINT('Ctrl Pts',(0.995731745287223,2.23907760951407,16.8888952905783));
#5230=CARTESIAN_POINT('Ctrl Pts',(0.921368857178305,2.27214724856842,16.8931107866476));
#5231=CARTESIAN_POINT('Ctrl Pts',(0.845356570468824,2.30150846872209,16.8973262827169));
#5232=CARTESIAN_POINT('Ctrl Pts',(0.768100940561478,2.32700906640017,16.9015417787862));
#5233=CARTESIAN_POINT('Ctrl Pts',(0.690026684343838,2.35277987687972,16.9058019436518));
#5234=CARTESIAN_POINT('Ctrl Pts',(0.610683033284415,2.37460759369614,16.9100621085174));
#5235=CARTESIAN_POINT('Ctrl Pts',(0.530504267227748,2.3923869821693,16.9143222733829));
#5236=CARTESIAN_POINT('Ctrl Pts',(0.451050652339837,2.41000557065806,16.9185439085519));
#5237=CARTESIAN_POINT('Ctrl Pts',(0.37077744147681,2.42364874593634,16.9227655437209));
#5238=CARTESIAN_POINT('Ctrl Pts',(0.290115101997907,2.4332660104462,16.9269871788898));
#5239=CARTESIAN_POINT('Ctrl Pts',(0.208348488223305,2.44301493612609,16.9312666086037));
#5240=CARTESIAN_POINT('Ctrl Pts',(0.126182504257374,2.44862685258754,16.9355460383176));
#5241=CARTESIAN_POINT('Ctrl Pts',(0.0440663891710255,2.45010375358788,16.9398254680315));
#5242=CARTESIAN_POINT('Ctrl Pts',(-0.0380497259153342,2.45158065458822,
16.9441048977454));
#5243=CARTESIAN_POINT('Ctrl Pts',(-0.120115483911665,2.44892262146591,16.9483843274593));
#5244=CARTESIAN_POINT('Ctrl Pts',(-0.201688165846049,2.44218593349435,16.9526637571732));
#5245=CARTESIAN_POINT('Ctrl Pts',(-0.2823320195379,2.43552595289467,16.9568944591134));
#5246=CARTESIAN_POINT('Ctrl Pts',(-0.362797296576188,2.42485472160487,16.9611251610537));
#5247=CARTESIAN_POINT('Ctrl Pts',(-0.442653106968677,2.41018847331303,16.9653558629939));
#5248=CARTESIAN_POINT('Ctrl Pts',(-0.522394186534465,2.39554329638447,16.9695804865796));
#5249=CARTESIAN_POINT('Ctrl Pts',(-0.601527084986443,2.37691458518842,16.9738051101653));
#5250=CARTESIAN_POINT('Ctrl Pts',(-0.679625034710922,2.35437041737153,16.9780297337509));
#5251=CARTESIAN_POINT('Ctrl Pts',(-0.758030362514393,2.33173752017031,16.9822709846192));
#5252=CARTESIAN_POINT('Ctrl Pts',(-0.835392104465863,2.30515831837505,16.9865122354875));
#5253=CARTESIAN_POINT('Ctrl Pts',(-0.911287793776045,2.27475379039464,16.9907534863558));
#5254=CARTESIAN_POINT('Ctrl Pts',(-0.98674950958664,2.24452311628566,16.9949704856428));
#5255=CARTESIAN_POINT('Ctrl Pts',(-1.06076145706699,2.21051091859264,16.9991874849297));
#5256=CARTESIAN_POINT('Ctrl Pts',(-1.13292438696323,2.17288577321128,17.0034044842167));
#5257=CARTESIAN_POINT('Ctrl Pts',(-1.20506339326942,2.13527310138878,17.0076200854761));
#5258=CARTESIAN_POINT('Ctrl Pts',(-1.27535418723763,2.09405007528635,17.0118356867356));
#5259=CARTESIAN_POINT('Ctrl Pts',(-1.34342038204212,2.04943209868339,17.016051287995));
#5260=CARTESIAN_POINT('Ctrl Pts',(-1.41148487841935,2.00481523541412,17.0202667840643));
#5261=CARTESIAN_POINT('Ctrl Pts',(-1.4773244976492,1.95680384593853,17.0244822801336));
#5262=CARTESIAN_POINT('Ctrl Pts',(-1.54059143022568,1.90565691957267,17.0286977762029));
#5263=CARTESIAN_POINT('Ctrl Pts',(-1.60452876023013,1.85396802338958,17.0329579410685));
#5264=CARTESIAN_POINT('Ctrl Pts',(-1.66583816997849,1.79907703632268,17.0372181059341));
#5265=CARTESIAN_POINT('Ctrl Pts',(-1.72419605836923,1.74129210711586,17.0414782707997));
#5266=CARTESIAN_POINT('Ctrl Pts',(-1.78202614753013,1.68402979519308,17.0456999059687));
#5267=CARTESIAN_POINT('Ctrl Pts',(-1.8369576170974,1.62392606598167,17.0499215411376));
#5268=CARTESIAN_POINT('Ctrl Pts',(-1.88871495074155,1.56131549817625,17.0541431763066));
#5269=CARTESIAN_POINT('Ctrl Pts',(-1.94118084669036,1.49784778636636,17.0584226060205));
#5270=CARTESIAN_POINT('Ctrl Pts',(-1.99038474476865,1.43180447526388,17.0627020357344));
#5271=CARTESIAN_POINT('Ctrl Pts',(-2.03608509788801,1.36356434544116,17.0669814654483));
#5272=CARTESIAN_POINT('Ctrl Pts',(-2.08178545100736,1.29532421561844,17.0712608951622));
#5273=CARTESIAN_POINT('Ctrl Pts',(-2.12398206323079,1.22488772157969,17.075540324876));
#5274=CARTESIAN_POINT('Ctrl Pts',(-2.16248255848475,1.15265755289646,17.0798197545899));
#5275=CARTESIAN_POINT('Ctrl Pts',(-2.20267916262549,1.07724534122418,17.0842877111973));
#5276=CARTESIAN_POINT('Ctrl Pts',(-2.23898476198777,0.999620428064312,17.0887556678047));
#5277=CARTESIAN_POINT('Ctrl Pts',(-2.27116419083351,0.920197515903829,17.0932236244121));
#5278=CARTESIAN_POINT('Ctrl Pts',(-2.30324859241758,0.841009143078799,17.0976783869481));
#5279=CARTESIAN_POINT('Ctrl Pts',(-2.33123095314881,0.760033706883336,17.1021331494841));
#5280=CARTESIAN_POINT('Ctrl Pts',(-2.35492280758174,0.677708506904951,17.10658791202));
#5281=CARTESIAN_POINT('Ctrl Pts',(-2.37857232061478,0.595530436152888,17.1110347131327));
#5282=CARTESIAN_POINT('Ctrl Pts',(-2.39794647646274,0.5120077714379,17.1154815142454));
#5283=CARTESIAN_POINT('Ctrl Pts',(-2.41290518136713,0.427596580589296,17.1199283153581));
#5284=CARTESIAN_POINT('Ctrl Pts',(-2.42782859230949,0.343384551725846,17.1243646245712));
#5285=CARTESIAN_POINT('Ctrl Pts',(-2.4383572374737,0.258288553179804,17.1288009337843));
#5286=CARTESIAN_POINT('Ctrl Pts',(-2.44440142582966,0.172777080082745,17.1332372429974));
#5287=CARTESIAN_POINT('Ctrl Pts',(-2.44845933346365,0.115366946738365,17.1362156632521));
#5288=CARTESIAN_POINT('Ctrl Pts',(-2.45049693206647,0.0577698600948637,
17.1391940835069));
#5289=CARTESIAN_POINT('Ctrl Pts',(-2.45049999653667,0.000130283472656437,
17.1421725037616));
#5290=CARTESIAN_POINT('',(-2.45049898498602,-0.00223037720147216,17.942172503788));
#5291=CARTESIAN_POINT('Ctrl Pts',(-2.4504999965367,0.000130282960863897,
17.142172503788));
#5292=CARTESIAN_POINT('Ctrl Pts',(-2.45050452194911,-0.0849884696040502,
17.1465708604649));
#5293=CARTESIAN_POINT('Ctrl Pts',(-2.44606980392813,-0.170029198439797,
17.1509692171419));
#5294=CARTESIAN_POINT('Ctrl Pts',(-2.43724598391095,-0.254523601872133,
17.1553675738189));
#5295=CARTESIAN_POINT('Ctrl Pts',(-2.42839970581627,-0.339233057499113,
17.1597771250391));
#5296=CARTESIAN_POINT('Ctrl Pts',(-2.41514204232485,-0.423393005931581,
17.1641866762593));
#5297=CARTESIAN_POINT('Ctrl Pts',(-2.39757477354347,-0.506542649011867,
17.1685962274796));
#5298=CARTESIAN_POINT('Ctrl Pts',(-2.37998497661235,-0.58979892264665,17.1730114334792));
#5299=CARTESIAN_POINT('Ctrl Pts',(-2.35807465958441,-0.672041917858444,
17.1774266394789));
#5300=CARTESIAN_POINT('Ctrl Pts',(-2.33199555060948,-0.752826010401865,
17.1818418454786));
#5301=CARTESIAN_POINT('Ctrl Pts',(-2.305845995393,-0.833828321125292,17.1862689780617));
#5302=CARTESIAN_POINT('Ctrl Pts',(-2.27550527631956,-0.913363471002124,
17.1906961106448));
#5303=CARTESIAN_POINT('Ctrl Pts',(-2.24117371120437,-0.991004866893403,
17.1951232432279));
#5304=CARTESIAN_POINT('Ctrl Pts',(-2.2105357328379,-1.06029315595564,17.1990740794875));
#5305=CARTESIAN_POINT('Ctrl Pts',(-2.17672019184866,-1.12807340583658,17.2030249157471));
#5306=CARTESIAN_POINT('Ctrl Pts',(-2.13989918397987,-1.19406102540963,17.2069757520067));
#5307=CARTESIAN_POINT('Ctrl Pts',(-2.10046988365032,-1.26472301487633,17.2112064539469));
#5308=CARTESIAN_POINT('Ctrl Pts',(-2.05746265756894,-1.33356278892363,17.2154371558872));
#5309=CARTESIAN_POINT('Ctrl Pts',(-2.01107056395207,-1.40019478530863,17.2196678578274));
#5310=CARTESIAN_POINT('Ctrl Pts',(-1.96474512300856,-1.46673104984919,17.2238924814131));
#5311=CARTESIAN_POINT('Ctrl Pts',(-1.91504473643684,-1.53106545800606,17.2281171049988));
#5312=CARTESIAN_POINT('Ctrl Pts',(-1.86220795516761,-1.59283765077,17.2323417285845));
#5313=CARTESIAN_POINT('Ctrl Pts',(-1.80916321878083,-1.65485296666328,17.2365829794528));
#5314=CARTESIAN_POINT('Ctrl Pts',(-1.7529575775228,-1.71428544075453,17.2408242303211));
#5315=CARTESIAN_POINT('Ctrl Pts',(-1.69387596331298,-1.77080051697262,17.2450654811893));
#5316=CARTESIAN_POINT('Ctrl Pts',(-1.63513217928983,-1.82699243853417,17.2492824804763));
#5317=CARTESIAN_POINT('Ctrl Pts',(-1.57354556228432,-1.88029991050138,17.2534994797632));
#5318=CARTESIAN_POINT('Ctrl Pts',(-1.50943477042274,-1.93042920715546,17.2577164790502));
#5319=CARTESIAN_POINT('Ctrl Pts',(-1.44534523269119,-1.98054188485104,17.2619320803096));
#5320=CARTESIAN_POINT('Ctrl Pts',(-1.37873354795455,-2.02747819333673,17.266147681569));
#5321=CARTESIAN_POINT('Ctrl Pts',(-1.30995154682968,-2.07098459553868,17.2703632828285));
#5322=CARTESIAN_POINT('Ctrl Pts',(-1.24117126199333,-2.11448991214358,17.2745787788978));
#5323=CARTESIAN_POINT('Ctrl Pts',(-1.17022116205761,-2.15456524494081,17.2787942749671));
#5324=CARTESIAN_POINT('Ctrl Pts',(-1.09748093380663,-2.19100110678451,17.2830097710364));
#5325=CARTESIAN_POINT('Ctrl Pts',(-1.02396992594062,-2.22782305512038,17.2872699359019));
#5326=CARTESIAN_POINT('Ctrl Pts',(-0.948631052230668,-2.2609277117866,17.2915301007675));
#5327=CARTESIAN_POINT('Ctrl Pts',(-0.871878737678063,-2.29014796831666,
17.2957902656331));
#5328=CARTESIAN_POINT('Ctrl Pts',(-0.795820584851126,-2.3191039515956,17.3000119008021));
#5329=CARTESIAN_POINT('Ctrl Pts',(-0.718374921478922,-2.34424542805932,
17.304233535971));
#5330=CARTESIAN_POINT('Ctrl Pts',(-0.639960339280295,-2.36546000053864,
17.30845517114));
#5331=CARTESIAN_POINT('Ctrl Pts',(-0.560472254774414,-2.38696500232161,
17.3127346008539));
#5332=CARTESIAN_POINT('Ctrl Pts',(-0.479989004807428,-2.40443466179837,
17.3170140305678));
#5333=CARTESIAN_POINT('Ctrl Pts',(-0.398955367489305,-2.4178057954996,17.3212934602817));
#5334=CARTESIAN_POINT('Ctrl Pts',(-0.317921730171183,-2.43117692920084,
17.3255728899955));
#5335=CARTESIAN_POINT('Ctrl Pts',(-0.236338200347234,-2.44044954679654,
17.3298523197094));
#5336=CARTESIAN_POINT('Ctrl Pts',(-0.154650978361386,-2.44561512198708,
17.3341317494233));
#5337=CARTESIAN_POINT('Ctrl Pts',(-0.0738938888296647,-2.45072187929873,
17.3383624513636));
#5338=CARTESIAN_POINT('Ctrl Pts',(0.00726829076739741,-2.45183389960285,
17.3425931533038));
#5339=CARTESIAN_POINT('Ctrl Pts',(0.0884068720681205,-2.44890475008138,
17.3468238552441));
#5340=CARTESIAN_POINT('Ctrl Pts',(0.169428879553403,-2.44597980894179,17.3510484788298));
#5341=CARTESIAN_POINT('Ctrl Pts',(0.250426895263739,-2.43902524574518,17.3552731024155));
#5342=CARTESIAN_POINT('Ctrl Pts',(0.330968790351253,-2.42804652134456,17.3594977260012));
#5343=CARTESIAN_POINT('Ctrl Pts',(0.411827682402982,-2.4170245868568,17.3637389768694));
#5344=CARTESIAN_POINT('Ctrl Pts',(0.492226382121687,-2.40194671666983,17.3679802277377));
#5345=CARTESIAN_POINT('Ctrl Pts',(0.571729343457058,-2.38287133681829,17.372221478606));
#5346=CARTESIAN_POINT('Ctrl Pts',(0.650777704818788,-2.36390503047837,17.376438477893));
#5347=CARTESIAN_POINT('Ctrl Pts',(0.728940086938435,-2.34098691574096,17.3806554771799));
#5348=CARTESIAN_POINT('Ctrl Pts',(0.805797012423679,-2.31422588023924,17.3848724764669));
#5349=CARTESIAN_POINT('Ctrl Pts',(0.882628458156655,-2.28747371660626,17.3890880777263));
#5350=CARTESIAN_POINT('Ctrl Pts',(0.958154867847561,-2.25688131498564,17.3933036789858));
#5351=CARTESIAN_POINT('Ctrl Pts',(1.03197259303029,-2.22260721164004,17.3975192802452));
#5352=CARTESIAN_POINT('Ctrl Pts',(1.10578847627005,-2.18833396352188,17.4017347763145));
#5353=CARTESIAN_POINT('Ctrl Pts',(1.17789533841908,-2.15037939316877,17.4059502723838));
#5354=CARTESIAN_POINT('Ctrl Pts',(1.24791148466067,-2.10894930627837,17.4101657684531));
#5355=CARTESIAN_POINT('Ctrl Pts',(1.31866954523984,-2.06708021242856,17.4144259333187));
#5356=CARTESIAN_POINT('Ctrl Pts',(1.38729189310412,-2.02166174087271,17.4186860981843));
#5357=CARTESIAN_POINT('Ctrl Pts',(1.45341365594795,-1.97295184804495,17.4229462630499));
#5358=CARTESIAN_POINT('Ctrl Pts',(1.51893740168615,-1.9246824962414,17.4271678982188));
#5359=CARTESIAN_POINT('Ctrl Pts',(1.58200528676912,-1.87318136533049,17.4313895333878));
#5360=CARTESIAN_POINT('Ctrl Pts',(1.64229618191589,-1.81873953629003,17.4356111685568));
#5361=CARTESIAN_POINT('Ctrl Pts',(1.70341246455095,-1.76355239397432,17.4398905982707));
#5362=CARTESIAN_POINT('Ctrl Pts',(1.76167479715392,-1.70534377668145,17.4441700279846));
#5363=CARTESIAN_POINT('Ctrl Pts',(1.81678924960985,-1.64445342667467,17.4484494576985));
#5364=CARTESIAN_POINT('Ctrl Pts',(1.87190370206578,-1.5835630766679,17.4527288874124));
#5365=CARTESIAN_POINT('Ctrl Pts',(1.92387001458967,-1.51999141522758,17.4570083171263));
#5366=CARTESIAN_POINT('Ctrl Pts',(1.97243944047889,-1.45410897241002,17.4612877468402));
#5367=CARTESIAN_POINT('Ctrl Pts',(2.02045583006451,-1.38897670075427,17.4655184487804));
#5368=CARTESIAN_POINT('Ctrl Pts',(2.06533293501881,-1.32134104863923,17.4697491507207));
#5369=CARTESIAN_POINT('Ctrl Pts',(2.10679961964322,-1.25153729975226,17.4739798526609));
#5370=CARTESIAN_POINT('Ctrl Pts',(2.14820672805185,-1.18183383964516,17.4782044762466));
#5371=CARTESIAN_POINT('Ctrl Pts',(2.1862129119699,-1.10996886568492,17.4824290998323));
#5372=CARTESIAN_POINT('Ctrl Pts',(2.2205888029732,-1.03630865002182,17.486653723418));
#5373=CARTESIAN_POINT('Ctrl Pts',(2.25509999068222,-0.962358522323541,17.4908949742863));
#5374=CARTESIAN_POINT('Ctrl Pts',(2.28595196635849,-0.886599373155283,17.4951362251546));
#5375=CARTESIAN_POINT('Ctrl Pts',(2.31295804233885,-0.809429023682766,17.4993774760229));
#5376=CARTESIAN_POINT('Ctrl Pts',(2.33980969688355,-0.732699936249384,17.5035944753098));
#5377=CARTESIAN_POINT('Ctrl Pts',(2.36285915913114,-0.654576186647708,17.5078114745968));
#5378=CARTESIAN_POINT('Ctrl Pts',(2.38197086714886,-0.575469406705611,17.5120284738837));
#5379=CARTESIAN_POINT('Ctrl Pts',(2.40107623921725,-0.496388852391768,17.5162440751432));
#5380=CARTESIAN_POINT('Ctrl Pts',(2.4162463403341,-0.416326366608398,17.5204596764026));
#5381=CARTESIAN_POINT('Ctrl Pts',(2.42739592099358,-0.335707153250742,17.524675277662));
#5382=CARTESIAN_POINT('Ctrl Pts',(2.43854522344226,-0.255089951550467,17.5288907737313));
#5383=CARTESIAN_POINT('Ctrl Pts',(2.44567414226284,-0.173916510720612,17.5331062698006));
#5384=CARTESIAN_POINT('Ctrl Pts',(2.44874905604843,-0.0926191691926037,
17.5373217658699));
#5385=CARTESIAN_POINT('Ctrl Pts',(2.45185655264164,-0.0104603740357106,
17.5415819307355));
#5386=CARTESIAN_POINT('Ctrl Pts',(2.45082358306199,0.0718244797267152,17.5458420956011));
#5387=CARTESIAN_POINT('Ctrl Pts',(2.44566947993344,0.153788962289517,17.5501022604666));
#5388=CARTESIAN_POINT('Ctrl Pts',(2.4405619914398,0.235012143342659,17.5543238956356));
#5389=CARTESIAN_POINT('Ctrl Pts',(2.43140772829692,0.31592026456825,17.5585455308046));
#5390=CARTESIAN_POINT('Ctrl Pts',(2.41827755582974,0.39608573941781,17.5627671659735));
#5391=CARTESIAN_POINT('Ctrl Pts',(2.40496763018349,0.477348686443871,17.5670465956874));
#5392=CARTESIAN_POINT('Ctrl Pts',(2.38757221436303,0.557848015856512,17.5713260254013));
#5393=CARTESIAN_POINT('Ctrl Pts',(2.36621781198581,0.6371526632143,17.5756054551152));
#5394=CARTESIAN_POINT('Ctrl Pts',(2.34486340960859,0.716457310572088,17.5798848848291));
#5395=CARTESIAN_POINT('Ctrl Pts',(2.31955023421858,0.794566829372656,17.584164314543));
#5396=CARTESIAN_POINT('Ctrl Pts',(2.29045513733653,0.871071474592463,17.5884437442568));
#5397=CARTESIAN_POINT('Ctrl Pts',(2.26169133209598,0.946704998825821,17.5926744461971));
#5398=CARTESIAN_POINT('Ctrl Pts',(2.2291231450125,1.02105450572532,17.5969051481374));
#5399=CARTESIAN_POINT('Ctrl Pts',(2.1928856722894,1.09371050935239,17.6011358500776));
#5400=CARTESIAN_POINT('Ctrl Pts',(2.1567002628436,1.16626212629407,17.6053604736633));
#5401=CARTESIAN_POINT('Ctrl Pts',(2.11685624355658,1.23712465959145,17.609585097249));
#5402=CARTESIAN_POINT('Ctrl Pts',(2.07353737771213,1.30590696193516,17.6138097208347));
#5403=CARTESIAN_POINT('Ctrl Pts',(2.03004801738214,1.37495997781263,17.6180509717029));
#5404=CARTESIAN_POINT('Ctrl Pts',(1.98305656789875,1.44191590929957,17.6222922225712));
#5405=CARTESIAN_POINT('Ctrl Pts',(1.93279642548741,1.50640241224683,17.6265334734395));
#5406=CARTESIAN_POINT('Ctrl Pts',(1.88282367186057,1.57052017971487,17.6307504727265));
#5407=CARTESIAN_POINT('Ctrl Pts',(1.82961979357151,1.63219631202484,17.6349674720134));
#5408=CARTESIAN_POINT('Ctrl Pts',(1.77345747833991,1.69109397211398,17.6391844713004));
#5409=CARTESIAN_POINT('Ctrl Pts',(1.71731378214439,1.74997210634039,17.6434000725598));
#5410=CARTESIAN_POINT('Ctrl Pts',(1.65821391736659,1.80607326123916,17.6476156738193));
#5411=CARTESIAN_POINT('Ctrl Pts',(1.5964692222879,1.85909555222088,17.6518312750787));
#5412=CARTESIAN_POINT('Ctrl Pts',(1.53472606789875,1.91211652015956,17.656046771148));
#5413=CARTESIAN_POINT('Ctrl Pts',(1.47033856795327,1.9620584747717,17.6602622672173));
#5414=CARTESIAN_POINT('Ctrl Pts',(1.40365201121218,2.00865907545806,17.6644777632866));
#5415=CARTESIAN_POINT('Ctrl Pts',(1.33625882156986,2.05575347158492,17.6687379281522));
#5416=CARTESIAN_POINT('Ctrl Pts',(1.26651794977077,2.09943498925052,17.6729980930178));
#5417=CARTESIAN_POINT('Ctrl Pts',(1.19481520194372,2.13947818011874,17.6772582578834));
#5418=CARTESIAN_POINT('Ctrl Pts',(1.12376094665349,2.17915921317272,17.6814798930524));
#5419=CARTESIAN_POINT('Ctrl Pts',(1.05078060854846,2.21526731287341,17.6857015282213));
#5420=CARTESIAN_POINT('Ctrl Pts',(0.976272051562424,2.24763055935314,17.6899231633903));
#5421=CARTESIAN_POINT('Ctrl Pts',(0.900743466086785,2.28043686143293,17.6942025931042));
#5422=CARTESIAN_POINT('Ctrl Pts',(0.823644965085444,2.30939482529144,17.6984820228181));
#5423=CARTESIAN_POINT('Ctrl Pts',(0.745407459787558,2.33437742640154,17.702761452532));
#5424=CARTESIAN_POINT('Ctrl Pts',(0.667169954489682,2.35936002751163,17.7070408822459));
#5425=CARTESIAN_POINT('Ctrl Pts',(0.587793935910716,2.38036720367035,17.7113203119598));
#5426=CARTESIAN_POINT('Ctrl Pts',(0.507719649770126,2.39732580331446,17.7155997416737));
#5427=CARTESIAN_POINT('Ctrl Pts',(0.428557130371937,2.41409130367665,17.7198304436139));
#5428=CARTESIAN_POINT('Ctrl Pts',(0.348414420808694,2.42696305918836,17.7240611455542));
#5429=CARTESIAN_POINT('Ctrl Pts',(0.267708942148703,2.43583295246074,17.7282918474944));
#5430=CARTESIAN_POINT('Ctrl Pts',(0.187119415054621,2.44469010213713,17.7325164710801));
#5431=CARTESIAN_POINT('Ctrl Pts',(0.105969183031929,2.44955675817102,17.7367410946658));
#5432=CARTESIAN_POINT('Ctrl Pts',(0.0246865977423455,2.4503756491387,17.7409657182515));
#5433=CARTESIAN_POINT('Ctrl Pts',(-0.0569158997213942,2.45119776309921,
17.7452069691197));
#5434=CARTESIAN_POINT('Ctrl Pts',(-0.138651330262372,2.44794008292565,17.749448219988));
#5435=CARTESIAN_POINT('Ctrl Pts',(-0.220080279254648,2.44059724671712,17.7536894708563));
#5436=CARTESIAN_POINT('Ctrl Pts',(-0.301043615426376,2.43329639703452,17.7579064701433));
#5437=CARTESIAN_POINT('Ctrl Pts',(-0.381703497639979,2.42195702478503,17.7621234694302));
#5438=CARTESIAN_POINT('Ctrl Pts',(-0.461629091239075,2.40662602664431,17.7663404687172));
#5439=CARTESIAN_POINT('Ctrl Pts',(-0.541528187755332,2.39130011106488,17.7705560699766));
#5440=CARTESIAN_POINT('Ctrl Pts',(-0.62069302270116,2.37198528500524,17.774771671236));
#5441=CARTESIAN_POINT('Ctrl Pts',(-0.698701222103131,2.34877986457471,17.7789872724955));
#5442=CARTESIAN_POINT('Ctrl Pts',(-0.776707474999244,2.32557502317929,17.7832027685648));
#5443=CARTESIAN_POINT('Ctrl Pts',(-0.853556704287896,2.29847991407354,17.7874182646341));
#5444=CARTESIAN_POINT('Ctrl Pts',(-0.928841401711176,2.26764280707241,17.7916337607034));
#5445=CARTESIAN_POINT('Ctrl Pts',(-1.00492384078969,2.23647893984478,17.795893925569));
#5446=CARTESIAN_POINT('Ctrl Pts',(-1.0794079395581,2.20149346835275,17.8001540904345));
#5447=CARTESIAN_POINT('Ctrl Pts',(-1.15189527062322,2.1628887016016,17.8044142553001));
#5448=CARTESIAN_POINT('Ctrl Pts',(-1.22372701323978,2.12463308329846,17.8086358904691));
#5449=CARTESIAN_POINT('Ctrl Pts',(-1.2935975893135,2.08282366793475,17.812857525638));
#5450=CARTESIAN_POINT('Ctrl Pts',(-1.36114704767522,2.03770188315294,17.817079160807));
#5451=CARTESIAN_POINT('Ctrl Pts',(-1.4296212638737,1.99196237729538,17.8213585905209));
#5452=CARTESIAN_POINT('Ctrl Pts',(-1.49570993162505,1.94281941724692,17.8256380202348));
#5453=CARTESIAN_POINT('Ctrl Pts',(-1.55907295365824,1.89056652228145,17.8299174499487));
#5454=CARTESIAN_POINT('Ctrl Pts',(-1.62243597569142,1.83831362731599,17.8341968796625));
#5455=CARTESIAN_POINT('Ctrl Pts',(-1.68307303386725,1.78295117658104,17.8384763093764));
#5456=CARTESIAN_POINT('Ctrl Pts',(-1.74068427121074,1.72480970485429,17.8427557390903));
#5457=CARTESIAN_POINT('Ctrl Pts',(-1.79684041836039,1.6681367154804,17.8469270830123));
#5458=CARTESIAN_POINT('Ctrl Pts',(-1.85034552545446,1.60859737264218,17.8510984269343));
#5459=CARTESIAN_POINT('Ctrl Pts',(-1.90088679305653,1.54647329430006,17.8552697708562));
#5460=CARTESIAN_POINT('Ctrl Pts',(-1.95136270988477,1.4844295435157,17.859435721155));
#5461=CARTESIAN_POINT('Ctrl Pts',(-1.99888208736877,1.41980805190744,17.8636016714538));
#5462=CARTESIAN_POINT('Ctrl Pts',(-2.04316834329773,1.35292770351782,17.8677676217525));
#5463=CARTESIAN_POINT('Ctrl Pts',(-2.08741180345981,1.28611198456545,17.8719295463094));
#5464=CARTESIAN_POINT('Ctrl Pts',(-2.1284280766816,1.21704213571831,17.8760914708662));
#5465=CARTESIAN_POINT('Ctrl Pts',(-2.16598137453289,1.14606934134747,17.880253395423));
#5466=CARTESIAN_POINT('Ctrl Pts',(-2.20351064302982,1.07514196057606,17.8844126568753));
#5467=CARTESIAN_POINT('Ctrl Pts',(-2.2375811105656,1.00231447313695,17.8885719183275));
#5468=CARTESIAN_POINT('Ctrl Pts',(-2.26800165933593,0.927964828670506,17.8927311797798));
#5469=CARTESIAN_POINT('Ctrl Pts',(-2.29842423865501,0.853610221421215,17.8968907188596));
#5470=CARTESIAN_POINT('Ctrl Pts',(-2.3251962132241,0.777733690129484,17.9010502579394));
#5471=CARTESIAN_POINT('Ctrl Pts',(-2.34817408744007,0.700734404089727,17.9052097970192));
#5472=CARTESIAN_POINT('Ctrl Pts',(-2.37115120639293,0.623737648950773,17.9093691993785));
#5473=CARTESIAN_POINT('Ctrl Pts',(-2.39033434371149,0.545618674236535,17.9135286017379));
#5474=CARTESIAN_POINT('Ctrl Pts',(-2.40563014694911,0.466791009006805,17.9176880040972));
#5475=CARTESIAN_POINT('Ctrl Pts',(-2.42094168019271,0.38788227842697,17.921851683932));
#5476=CARTESIAN_POINT('Ctrl Pts',(-2.43235781014975,0.308263874397381,17.9260153637668));
#5477=CARTESIAN_POINT('Ctrl Pts',(-2.43983664962272,0.228357993417779,17.9301790436017));
#5478=CARTESIAN_POINT('Ctrl Pts',(-2.44701757026798,0.151635155271715,17.9341768636638));
#5479=CARTESIAN_POINT('Ctrl Pts',(-2.45056895731561,0.0746477053583067,
17.9381746837259));
#5480=CARTESIAN_POINT('Ctrl Pts',(-2.45049898498602,-0.00223037720147216,
17.942172503788));
#5481=CARTESIAN_POINT('',(-2.4506184992838,0.00106435978254121,18.742172503788));
#5482=CARTESIAN_POINT('Ctrl Pts',(-2.45086623049305,-0.00223071145829692,
17.942172503788));
#5483=CARTESIAN_POINT('Ctrl Pts',(-2.45251448448338,-0.180067494476928,
17.9514189146944));
#5484=CARTESIAN_POINT('Ctrl Pts',(-2.35363103519027,-1.17128619448211,18.0030506580727));
#5485=CARTESIAN_POINT('Ctrl Pts',(-1.00509395767141,-2.71753796896942,18.0970677339241));
#5486=CARTESIAN_POINT('Ctrl Pts',(1.74062071602852,-2.31634755584424,18.2242237313404));
#5487=CARTESIAN_POINT('Ctrl Pts',(2.8898793093525,0.2093419544921,18.3513797287573));
#5488=CARTESIAN_POINT('Ctrl Pts',(1.38860906978141,2.54302798408779,18.478535726174));
#5489=CARTESIAN_POINT('Ctrl Pts',(-1.38626050840876,2.54430899840504,18.6056917235908));
#5490=CARTESIAN_POINT('Ctrl Pts',(-2.42529377406342,0.93243124355413,18.693570649462));
#5491=CARTESIAN_POINT('Ctrl Pts',(-2.45429862551719,0.0606504956432896,
18.7390642428612));
#5492=CARTESIAN_POINT('Ctrl Pts',(-2.45397396328318,0.00106581713746319,
18.742172503788));
#5493=CARTESIAN_POINT('',(-2.45049945194367,0.00163890932561317,19.5421725037581));
#5494=CARTESIAN_POINT('Ctrl Pts',(-2.45049976887328,0.00106430821520263,
18.742172503788));
#5495=CARTESIAN_POINT('Ctrl Pts',(-2.45053457116055,-0.0790656726323252,
18.7463584563462));
#5496=CARTESIAN_POINT('Ctrl Pts',(-2.44663482555748,-0.159355808443341,
18.7505444089043));
#5497=CARTESIAN_POINT('Ctrl Pts',(-2.43877965671853,-0.239382614188756,
18.7547303614625));
#5498=CARTESIAN_POINT('Ctrl Pts',(-2.43054835629879,-0.323241369261778,
18.7591167513359));
#5499=CARTESIAN_POINT('Ctrl Pts',(-2.41797325303157,-0.406810428678383,
18.7635031412093));
#5500=CARTESIAN_POINT('Ctrl Pts',(-2.40109181530018,-0.489600188417552,
18.7678895310827));
#5501=CARTESIAN_POINT('Ctrl Pts',(-2.38502088583557,-0.568415062501779,
18.7720653224686));
#5502=CARTESIAN_POINT('Ctrl Pts',(-2.36504768720019,-0.646523207224635,
18.7762411138544));
#5503=CARTESIAN_POINT('Ctrl Pts',(-2.34125756179545,-0.72350762216829,18.7804169052403));
#5504=CARTESIAN_POINT('Ctrl Pts',(-2.31747992244937,-0.800451632452265,
18.7845905049952));
#5505=CARTESIAN_POINT('Ctrl Pts',(-2.28988947121388,-0.876272629655242,
18.7887641047501));
#5506=CARTESIAN_POINT('Ctrl Pts',(-2.25862197796099,-0.950566678708845,
18.7929377045049));
#5507=CARTESIAN_POINT('Ctrl Pts',(-2.22736082903732,-1.02484565313201,18.7971104574157));
#5508=CARTESIAN_POINT('Ctrl Pts',(-2.19242430421625,-1.09759785649272,18.8012832103266));
#5509=CARTESIAN_POINT('Ctrl Pts',(-2.15399652099998,-1.16843880349806,18.8054559632374));
#5510=CARTESIAN_POINT('Ctrl Pts',(-2.11556416357172,-1.2392881829833,18.8096292128476));
#5511=CARTESIAN_POINT('Ctrl Pts',(-2.07363995182133,-1.30822543773806,18.8138024624578));
#5512=CARTESIAN_POINT('Ctrl Pts',(-2.02845344465767,-1.37489158585557,18.817975712068));
#5513=CARTESIAN_POINT('Ctrl Pts',(-1.98321910359077,-1.44162830597076,18.822153379431));
#5514=CARTESIAN_POINT('Ctrl Pts',(-1.93471584461297,-1.50608872883522,18.826331046794));
#5515=CARTESIAN_POINT('Ctrl Pts',(-1.88321550237799,-1.56794439365789,18.830508714157));
#5516=CARTESIAN_POINT('Ctrl Pts',(-1.83168330219513,-1.62983832219806,18.8346889658117));
#5517=CARTESIAN_POINT('Ctrl Pts',(-1.7771506534256,-1.68912393887204,18.8388692174664));
#5518=CARTESIAN_POINT('Ctrl Pts',(-1.71992671606776,-1.74550919257286,18.8430494691212));
#5519=CARTESIAN_POINT('Ctrl Pts',(-1.66261026310583,-1.80198560595351,18.8472364791103));
#5520=CARTESIAN_POINT('Ctrl Pts',(-1.60259419652498,-1.85555198760924,18.8514234890995));
#5521=CARTESIAN_POINT('Ctrl Pts',(-1.54022063938599,-1.90595661860637,18.8556104990887));
#5522=CARTESIAN_POINT('Ctrl Pts',(-1.51840549222406,-1.9235856347036,18.8570749055339));
#5523=CARTESIAN_POINT('Ctrl Pts',(-1.49630221864495,-1.94082828205246,18.858539311979));
#5524=CARTESIAN_POINT('Ctrl Pts',(-1.47392622329029,-1.95767508496615,18.8600037184242));
#5525=CARTESIAN_POINT('Ctrl Pts',(-1.40928148802946,-2.00634586349845,18.8642344203645));
#5526=CARTESIAN_POINT('Ctrl Pts',(-1.34210184128869,-2.05190276253577,18.8684651223047));
#5527=CARTESIAN_POINT('Ctrl Pts',(-1.27271981542049,-2.09407127897692,18.872695824245));
#5528=CARTESIAN_POINT('Ctrl Pts',(-1.20343747243254,-2.13617921086289,18.8769204478307));
#5529=CARTESIAN_POINT('Ctrl Pts',(-1.13195942866265,-2.17490818912327,18.8811450714163));
#5530=CARTESIAN_POINT('Ctrl Pts',(-1.05864962455525,-2.21002516330222,18.885369695002));
#5531=CARTESIAN_POINT('Ctrl Pts',(-0.985051287562888,-2.24528035094382,
18.8896109458703));
#5532=CARTESIAN_POINT('Ctrl Pts',(-0.909607119529883,-2.27689475581945,
18.8938521967386));
#5533=CARTESIAN_POINT('Ctrl Pts',(-0.832713038728724,-2.30467768790588,
18.8980934476069));
#5534=CARTESIAN_POINT('Ctrl Pts',(-0.756258640255346,-2.33230175647348,
18.9023104468938));
#5535=CARTESIAN_POINT('Ctrl Pts',(-0.678371307078897,-2.35613789064822,
18.9065274461808));
#5536=CARTESIAN_POINT('Ctrl Pts',(-0.599461283012488,-2.37604638426295,
18.9107444454678));
#5537=CARTESIAN_POINT('Ctrl Pts',(-0.520577419345309,-2.39594827777652,
18.9149600467272));
#5538=CARTESIAN_POINT('Ctrl Pts',(-0.440671988645958,-2.41192500280049,
18.9191756479866));
#5539=CARTESIAN_POINT('Ctrl Pts',(-0.360169313483692,-2.42388702616782,
18.9233912492461));
#5540=CARTESIAN_POINT('Ctrl Pts',(-0.279668647070996,-2.43584875105179,
18.9276067453154));
#5541=CARTESIAN_POINT('Ctrl Pts',(-0.198571225995115,-2.4437959061757,18.9318222413847));
#5542=CARTESIAN_POINT('Ctrl Pts',(-0.117309027645596,-2.44769051189746,
18.936037737454));
#5543=CARTESIAN_POINT('Ctrl Pts',(-0.035185748056052,-2.4516263861548,18.9402979023196));
#5544=CARTESIAN_POINT('Ctrl Pts',(0.0471053385277078,-2.45142327603028,
18.9445580671852));
#5545=CARTESIAN_POINT('Ctrl Pts',(0.129117630040629,-2.44709601111454,18.9488182320507));
#5546=CARTESIAN_POINT('Ctrl Pts',(0.21038818765119,-2.44280788276032,18.9530398672197));
#5547=CARTESIAN_POINT('Ctrl Pts',(0.291384511415768,-2.43447000829624,18.9572615023887));
#5548=CARTESIAN_POINT('Ctrl Pts',(0.371678321882915,-2.42214893741948,18.9614831375577));
#5549=CARTESIAN_POINT('Ctrl Pts',(0.453071361452038,-2.40965919003333,18.9657625672715));
#5550=CARTESIAN_POINT('Ctrl Pts',(0.533742022627916,-2.39307645947105,18.9700419969854));
#5551=CARTESIAN_POINT('Ctrl Pts',(0.613257987155049,-2.37252289582009,18.9743214266993));
#5552=CARTESIAN_POINT('Ctrl Pts',(0.692773951682181,-2.35196933216913,18.9786008564132));
#5553=CARTESIAN_POINT('Ctrl Pts',(0.771134770927409,-2.3274451444598,18.9828802861271));
#5554=CARTESIAN_POINT('Ctrl Pts',(0.847928937232347,-2.29912304311971,18.987159715841));
#5555=CARTESIAN_POINT('Ctrl Pts',(0.923848685915583,-2.27112343169892,18.9913904177812));
#5556=CARTESIAN_POINT('Ctrl Pts',(0.99852284809259,-2.23930668313419,18.9956211197215));
#5557=CARTESIAN_POINT('Ctrl Pts',(1.07154059626096,-2.20380375727166,18.9998518216617));
#5558=CARTESIAN_POINT('Ctrl Pts',(1.14445343801666,-2.16835183934468,19.0040764452474));
#5559=CARTESIAN_POINT('Ctrl Pts',(1.21571417750632,-2.12922446394546,19.008301068833));
#5560=CARTESIAN_POINT('Ctrl Pts',(1.28492983413793,-2.086601440463,19.0125256924187));
#5561=CARTESIAN_POINT('Ctrl Pts',(1.35441790990017,-2.0438106611928,19.016766943287));
#5562=CARTESIAN_POINT('Ctrl Pts',(1.42184432495419,-1.9974968226691,19.0210081941553));
#5563=CARTESIAN_POINT('Ctrl Pts',(1.48683440038543,-1.94788955432039,19.0252494450236));
#5564=CARTESIAN_POINT('Ctrl Pts',(1.55145286089693,-1.89856594160562,19.0294664443105));
#5565=CARTESIAN_POINT('Ctrl Pts',(1.61366239489437,-1.84598674570537,19.0336834435975));
#5566=CARTESIAN_POINT('Ctrl Pts',(1.67312343250635,-1.79042124361787,19.0379004428844));
#5567=CARTESIAN_POINT('Ctrl Pts',(1.73256475748355,-1.73487416270991,19.0421160441438));
#5568=CARTESIAN_POINT('Ctrl Pts',(1.78925905601717,-1.67634305891479,19.0463316454033));
#5569=CARTESIAN_POINT('Ctrl Pts',(1.84290131915776,-1.61513621030754,19.0505472466627));
#5570=CARTESIAN_POINT('Ctrl Pts',(1.8965422437854,-1.55393088896916,19.054762742732));
#5571=CARTESIAN_POINT('Ctrl Pts',(1.94713097872967,-1.49005030603181,19.0589782388013));
#5572=CARTESIAN_POINT('Ctrl Pts',(1.99440171464466,-1.42383708710738,19.0631937348706));
#5573=CARTESIAN_POINT('Ctrl Pts',(2.04217334697579,-1.35692225092613,19.0674538997361));
#5574=CARTESIAN_POINT('Ctrl Pts',(2.08655594974478,-1.28762543457542,19.0717140646017));
#5575=CARTESIAN_POINT('Ctrl Pts',(2.12732019539282,-1.21633015101733,19.0759742294673));
#5576=CARTESIAN_POINT('Ctrl Pts',(2.16771576187756,-1.14567967481608,19.0801958646363));
#5577=CARTESIAN_POINT('Ctrl Pts',(2.20455800040119,-1.07306718226491,19.0844174998052));
#5578=CARTESIAN_POINT('Ctrl Pts',(2.23767098755369,-0.998888783329006,19.0886391349742));
#5579=CARTESIAN_POINT('Ctrl Pts',(2.27123729431996,-0.923694875795193,19.0929185646881));
#5580=CARTESIAN_POINT('Ctrl Pts',(2.30097129046953,-0.846892323751072,19.097197994402));
#5581=CARTESIAN_POINT('Ctrl Pts',(2.32674161238239,-0.768910735526684,19.1014774241159));
#5582=CARTESIAN_POINT('Ctrl Pts',(2.35251193429526,-0.690929147302285,19.1057568538298));
#5583=CARTESIAN_POINT('Ctrl Pts',(2.37431851481993,-0.611769013260816,19.1100362835437));
#5584=CARTESIAN_POINT('Ctrl Pts',(2.39208376642655,-0.531869819033359,19.1143157132576));
#5585=CARTESIAN_POINT('Ctrl Pts',(2.40964673379977,-0.452880397862379,19.1185464151979));
#5586=CARTESIAN_POINT('Ctrl Pts',(2.42332603911252,-0.372871569647813,19.1227771171382));
#5587=CARTESIAN_POINT('Ctrl Pts',(2.43300936096404,-0.292259643915091,19.1270078190784));
#5588=CARTESIAN_POINT('Ctrl Pts',(2.44267877054649,-0.211763535338648,19.1312324426641));
#5589=CARTESIAN_POINT('Ctrl Pts',(2.44836354387022,-0.130666507954575,19.1354570662498));
#5590=CARTESIAN_POINT('Ctrl Pts',(2.45000209268376,-0.0493963140853163,
19.1396816898355));
#5591=CARTESIAN_POINT('Ctrl Pts',(2.45164709050125,0.0321937431880368,19.1439229407038));
#5592=CARTESIAN_POINT('Ctrl Pts',(2.44921384221651,0.113957869726645,19.1481641915721));
#5593=CARTESIAN_POINT('Ctrl Pts',(2.44269255489609,0.195456727321471,19.1524054424403));
#5594=CARTESIAN_POINT('Ctrl Pts',(2.43620855646396,0.276489572356577,19.1566224417273));
#5595=CARTESIAN_POINT('Ctrl Pts',(2.42568318062485,0.357259705606298,19.1608394410143));
#5596=CARTESIAN_POINT('Ctrl Pts',(2.41115897688971,0.437335841389852,19.1650564403012));
#5597=CARTESIAN_POINT('Ctrl Pts',(2.39663958824586,0.517385430182562,19.1692720415607));
#5598=CARTESIAN_POINT('Ctrl Pts',(2.37812408725167,0.59674102116807,19.1734876428201));
#5599=CARTESIAN_POINT('Ctrl Pts',(2.35570652555938,0.674979270375724,19.1777032440795));
#5600=CARTESIAN_POINT('Ctrl Pts',(2.33328952324318,0.753215567336904,19.1819187401488));
#5601=CARTESIAN_POINT('Ctrl Pts',(2.3069707829594,0.830334131182133,19.1861342362181));
#5602=CARTESIAN_POINT('Ctrl Pts',(2.27689445744002,0.905925979138979,19.1903497322874));
#5603=CARTESIAN_POINT('Ctrl Pts',(2.24649943318727,0.982318823420394,19.194609897153));
#5604=CARTESIAN_POINT('Ctrl Pts',(2.21226688043444,1.05715194788344,19.1988700620186));
#5605=CARTESIAN_POINT('Ctrl Pts',(2.17439507993251,1.13002490519691,19.2031302268842));
#5606=CARTESIAN_POINT('Ctrl Pts',(2.13686579880013,1.20223878638869,19.2073518620531));
#5607=CARTESIAN_POINT('Ctrl Pts',(2.09576312380878,1.27252743926019,19.2115734972221));
#5608=CARTESIAN_POINT('Ctrl Pts',(2.05132484037338,1.34052849625329,19.2157951323911));
#5609=CARTESIAN_POINT('Ctrl Pts',(2.00627819305383,1.40946049350692,19.220074562105));
#5610=CARTESIAN_POINT('Ctrl Pts',(1.95780420739321,1.47604138597362,19.2243539918189));
#5611=CARTESIAN_POINT('Ctrl Pts',(1.90619295800689,1.5399281336624,19.2286334215328));
#5612=CARTESIAN_POINT('Ctrl Pts',(1.85458170862056,1.60381488135119,19.2329128512467));
#5613=CARTESIAN_POINT('Ctrl Pts',(1.79983357142846,1.66500716231549,19.2371922809606));
#5614=CARTESIAN_POINT('Ctrl Pts',(1.74227604047339,1.72320180152888,19.2414717106744));
#5615=CARTESIAN_POINT('Ctrl Pts',(1.68537388897927,1.7807338068411,19.2457024126147));
#5616=CARTESIAN_POINT('Ctrl Pts',(1.62551200269707,1.83555251310885,19.249933114555));
#5617=CARTESIAN_POINT('Ctrl Pts',(1.56297958485521,1.88733809036056,19.2541638164952));
#5618=CARTESIAN_POINT('Ctrl Pts',(1.50053700889162,1.93904926598687,19.2583884400809));
#5619=CARTESIAN_POINT('Ctrl Pts',(1.4354318766455,1.98773567326336,19.2626130636666));
#5620=CARTESIAN_POINT('Ctrl Pts',(1.36799047949101,2.03311394122955,19.2668376872523));
#5621=CARTESIAN_POINT('Ctrl Pts',(1.30028364634036,2.07867080908053,19.2710789381206));
#5622=CARTESIAN_POINT('Ctrl Pts',(1.23022245239293,2.12089310400263,19.2753201889889));
#5623=CARTESIAN_POINT('Ctrl Pts',(1.15817097254293,2.15953472960241,19.2795614398571));
#5624=CARTESIAN_POINT('Ctrl Pts',(1.08653148490415,2.19795540139516,19.2837784391441));
#5625=CARTESIAN_POINT('Ctrl Pts',(1.01292482457118,2.23283601945678,19.2879954384311));
#5626=CARTESIAN_POINT('Ctrl Pts',(0.937736635034028,2.26397885443196,19.292212437718));
#5627=CARTESIAN_POINT('Ctrl Pts',(0.862573372026473,2.29511136487609,19.2964280389775));
#5628=CARTESIAN_POINT('Ctrl Pts',(0.785830050330047,2.32250837516458,19.3006436402369));
#5629=CARTESIAN_POINT('Ctrl Pts',(0.707913520251607,2.34601975649076,19.3048592414963));
#5630=CARTESIAN_POINT('Ctrl Pts',(0.62999893439183,2.36953055114726,19.3090747375656));
#5631=CARTESIAN_POINT('Ctrl Pts',(0.550911643900613,2.38915577630448,19.3132902336349));
#5632=CARTESIAN_POINT('Ctrl Pts',(0.47107355011746,2.4047952013383,19.3175057297043));
#5633=CARTESIAN_POINT('Ctrl Pts',(0.390389465379234,2.42060034691347,19.3217658945698));
#5634=CARTESIAN_POINT('Ctrl Pts',(0.308939043421075,2.43233461074559,19.3260260594354));
#5635=CARTESIAN_POINT('Ctrl Pts',(0.227166314896766,2.43994789193872,19.330286224301));
#5636=CARTESIAN_POINT('Ctrl Pts',(0.146133153624064,2.44749231724861,19.3345078594699));
#5637=CARTESIAN_POINT('Ctrl Pts',(0.064783964777887,2.45099004336911,19.3387294946389));
#5638=CARTESIAN_POINT('Ctrl Pts',(-0.0164478485506242,2.45044480008795,
19.3429511298079));
#5639=CARTESIAN_POINT('Ctrl Pts',(-0.0987917323201158,2.44989209237983,
19.3472305595217));
#5640=CARTESIAN_POINT('Ctrl Pts',(-0.181014508632247,2.44518490819366,19.3515099892356));
#5641=CARTESIAN_POINT('Ctrl Pts',(-0.262670714200779,2.4363814040296,19.3557894189495));
#5642=CARTESIAN_POINT('Ctrl Pts',(-0.344326919769299,2.42757789986554,19.3600688486634));
#5643=CARTESIAN_POINT('Ctrl Pts',(-0.425416080387719,2.41467821747543,19.3643482783773));
#5644=CARTESIAN_POINT('Ctrl Pts',(-0.505505990217372,2.39779355738862,19.3686277080912));
#5645=CARTESIAN_POINT('Ctrl Pts',(-0.584683955405516,2.38110115467008,19.3728584100314));
#5646=CARTESIAN_POINT('Ctrl Pts',(-0.663183129486453,2.3604513204167,19.3770891119717));
#5647=CARTESIAN_POINT('Ctrl Pts',(-0.740578034951599,2.33591404468299,19.3813198139119));
#5648=CARTESIAN_POINT('Ctrl Pts',(-0.817861745233491,2.31141202226285,19.3855444374976));
#5649=CARTESIAN_POINT('Ctrl Pts',(-0.89404389828307,2.28303379020035,19.3897690610833));
#5650=CARTESIAN_POINT('Ctrl Pts',(-0.968709589818176,2.25090026002804,19.3939936846689));
#5651=CARTESIAN_POINT('Ctrl Pts',(-1.04366915074293,2.21864025863844,19.3982349355372));
#5652=CARTESIAN_POINT('Ctrl Pts',(-1.11709982321787,2.18259543341046,19.4024761864055));
#5653=CARTESIAN_POINT('Ctrl Pts',(-1.1885975853881,2.14293864354759,19.4067174372738));
#5654=CARTESIAN_POINT('Ctrl Pts',(-1.25968652151896,2.10350861222711,19.4109344365608));
#5655=CARTESIAN_POINT('Ctrl Pts',(-1.32886418144413,2.0605080386378,19.4151514358477));
#5656=CARTESIAN_POINT('Ctrl Pts',(-1.39575553076662,2.0141541024297,19.4193684351347));
#5657=CARTESIAN_POINT('Ctrl Pts',(-1.46262470414334,1.9678155335656,19.4235840363941));
#5658=CARTESIAN_POINT('Ctrl Pts',(-1.52720869015421,1.91812607443534,19.4277996376536));
#5659=CARTESIAN_POINT('Ctrl Pts',(-1.58916099329976,1.86534650598073,19.432015238913));
#5660=CARTESIAN_POINT('Ctrl Pts',(-1.65111175057533,1.81256825451267,19.4362307349823));
#5661=CARTESIAN_POINT('Ctrl Pts',(-1.71043060224302,1.75670034944633,19.4404462310516));
#5662=CARTESIAN_POINT('Ctrl Pts',(-1.76680485626834,1.6980432414596,19.4446617271209));
#5663=CARTESIAN_POINT('Ctrl Pts',(-1.8237764706109,1.63876458327692,19.4489218919865));
#5664=CARTESIAN_POINT('Ctrl Pts',(-1.87774036455189,1.5766375977102,19.4531820568521));
#5665=CARTESIAN_POINT('Ctrl Pts',(-1.92841401193,1.51200848165348,19.4574422217177));
#5666=CARTESIAN_POINT('Ctrl Pts',(-1.97862935773484,1.44796388293663,19.4616638568866));
#5667=CARTESIAN_POINT('Ctrl Pts',(-2.02561351182488,1.38146265077972,19.4658854920556));
#5668=CARTESIAN_POINT('Ctrl Pts',(-2.06913496047938,1.3128711914434,19.4701071272246));
#5669=CARTESIAN_POINT('Ctrl Pts',(-2.1132522214718,1.2433407091882,19.4743865569385));
#5670=CARTESIAN_POINT('Ctrl Pts',(-2.15381100609893,1.17166276615782,19.4786659866523));
#5671=CARTESIAN_POINT('Ctrl Pts',(-2.19061903077547,1.09824337557954,19.4829454163662));
#5672=CARTESIAN_POINT('Ctrl Pts',(-2.22742705545201,1.02482398500127,19.4872248460801));
#5673=CARTESIAN_POINT('Ctrl Pts',(-2.26048418261586,0.949663622313898,19.491504275794));
#5674=CARTESIAN_POINT('Ctrl Pts',(-2.28964990358747,0.873185873111714,19.4957837055079));
#5675=CARTESIAN_POINT('Ctrl Pts',(-2.32256423751001,0.786878588702949,19.5006131619352));
#5676=CARTESIAN_POINT('Ctrl Pts',(-2.35062682282925,0.698624244662392,19.5054426183624));
#5677=CARTESIAN_POINT('Ctrl Pts',(-2.37363404666324,0.608943070016463,19.5102720747896));
#5678=CARTESIAN_POINT('Ctrl Pts',(-2.39654583737175,0.519633889612662,19.5150814988077));
#5679=CARTESIAN_POINT('Ctrl Pts',(-2.41444399167664,0.428909874622092,19.5198909228258));
#5680=CARTESIAN_POINT('Ctrl Pts',(-2.42717418291908,0.337306590168482,19.5247003468439));
#5681=CARTESIAN_POINT('Ctrl Pts',(-2.43981461087022,0.246349219994555,19.5294758585883));
#5682=CARTESIAN_POINT('Ctrl Pts',(-2.44735958946859,0.154525137024291,19.5342513703327));
#5683=CARTESIAN_POINT('Ctrl Pts',(-2.44970596636029,0.0623773066010869,
19.5390268820771));
#5684=CARTESIAN_POINT('Ctrl Pts',(-2.45022115121846,0.0421447654799862,
19.5400754226374));
#5685=CARTESIAN_POINT('Ctrl Pts',(-2.45048590341901,0.0218966818193598,
19.5411239631978));
#5686=CARTESIAN_POINT('Ctrl Pts',(-2.45049945194367,0.00163890932561401,
19.5421725037581));
#5687=CARTESIAN_POINT('',(-2.45049932159731,-0.00182341742444998,20.3421725038169));
#5688=CARTESIAN_POINT('Ctrl Pts',(-2.45049945194406,0.00163890874735187,
19.542172503788));
#5689=CARTESIAN_POINT('Ctrl Pts',(-2.45055421052195,-0.0802362202537292,
19.5464103534165));
#5690=CARTESIAN_POINT('Ctrl Pts',(-2.44650126866438,-0.162135992966076,
19.5506482030451));
#5691=CARTESIAN_POINT('Ctrl Pts',(-2.43835979033724,-0.2436222134095,19.5548860526736));
#5692=CARTESIAN_POINT('Ctrl Pts',(-2.43021791027491,-0.325112454729847,
19.5591241114157));
#5693=CARTESIAN_POINT('Ctrl Pts',(-2.41798713907103,-0.406188647603719,
19.5633621701577));
#5694=CARTESIAN_POINT('Ctrl Pts',(-2.40173848544174,-0.486418027573028,
19.5676002288998));
#5695=CARTESIAN_POINT('Ctrl Pts',(-2.38548424781723,-0.566674979086692,
19.5718397440887));
#5696=CARTESIAN_POINT('Ctrl Pts',(-2.36520947641946,-0.646084091091731,
19.5760792592776));
#5697=CARTESIAN_POINT('Ctrl Pts',(-2.34103593495839,-0.724224413585654,
19.5803187744664));
#5698=CARTESIAN_POINT('Ctrl Pts',(-2.3168305613789,-0.802467632546112,19.5845638723189));
#5699=CARTESIAN_POINT('Ctrl Pts',(-2.28871630843004,-0.879438289975786,
19.5888089701714));
#5700=CARTESIAN_POINT('Ctrl Pts',(-2.25686416502947,-0.954732627810438,
19.5930540680238));
#5701=CARTESIAN_POINT('Ctrl Pts',(-2.22498765303189,-1.03008456984939,19.5973024136037));
#5702=CARTESIAN_POINT('Ctrl Pts',(-2.18936775799712,-1.10375722818418,19.6015507591836));
#5703=CARTESIAN_POINT('Ctrl Pts',(-2.1502216757483,-1.17537100319098,19.6057991047634));
#5704=CARTESIAN_POINT('Ctrl Pts',(-2.11100646740166,-1.2471112373613,19.6100549522831));
#5705=CARTESIAN_POINT('Ctrl Pts',(-2.06825288421315,-1.31678494323608,19.6143107998027));
#5706=CARTESIAN_POINT('Ctrl Pts',(-2.02222143977996,-1.38404143669699,19.6185666473224));
#5707=CARTESIAN_POINT('Ctrl Pts',(-2.00645504894737,-1.40707769321667,19.6200243325231));
#5708=CARTESIAN_POINT('Ctrl Pts',(-1.99030445809036,-1.42983066454289,19.6214820177239));
#5709=CARTESIAN_POINT('Ctrl Pts',(-1.97378117384991,-1.452287205671,19.6229397029246));
#5710=CARTESIAN_POINT('Ctrl Pts',(-1.92582494114591,-1.51746378294187,19.6271704048649));
#5711=CARTESIAN_POINT('Ctrl Pts',(-1.87454674116935,-1.58038502095654,19.6314011068051));
#5712=CARTESIAN_POINT('Ctrl Pts',(-1.82018633211568,-1.64069252645926,19.6356318087454));
#5713=CARTESIAN_POINT('Ctrl Pts',(-1.76590402401204,-1.70091338667074,19.6398564323311));
#5714=CARTESIAN_POINT('Ctrl Pts',(-1.70854861038336,-1.75852762992536,19.6440810559168));
#5715=CARTESIAN_POINT('Ctrl Pts',(-1.64840183330512,-1.81320755732936,19.6483056795025));
#5716=CARTESIAN_POINT('Ctrl Pts',(-1.58801833041233,-1.86810269410921,19.6525469303708));
#5717=CARTESIAN_POINT('Ctrl Pts',(-1.52482172567811,-1.92003998548926,19.6567881812391));
#5718=CARTESIAN_POINT('Ctrl Pts',(-1.45913655136522,-1.96872313301541,19.6610294321073));
#5719=CARTESIAN_POINT('Ctrl Pts',(-1.39382696656495,-2.01712790905449,19.6652464313943));
#5720=CARTESIAN_POINT('Ctrl Pts',(-1.32605757175241,-2.0623153751098,19.6694634306813));
#5721=CARTESIAN_POINT('Ctrl Pts',(-1.25618125472064,-2.10403396010817,19.6736804299682));
#5722=CARTESIAN_POINT('Ctrl Pts',(-1.1863281032167,-2.14573871448291,19.6778960312277));
#5723=CARTESIAN_POINT('Ctrl Pts',(-1.11436981556875,-2.18397663331378,19.6821116324871));
#5724=CARTESIAN_POINT('Ctrl Pts',(-1.04068716597744,-2.21854016699492,19.6863272337466));
#5725=CARTESIAN_POINT('Ctrl Pts',(-0.967006354958359,-2.25310283822671,
19.6905427298159));
#5726=CARTESIAN_POINT('Ctrl Pts',(-0.891601689044287,-2.28399111008071,
19.6947582258852));
#5727=CARTESIAN_POINT('Ctrl Pts',(-0.814876071390042,-2.31104462057225,
19.6989737219545));
#5728=CARTESIAN_POINT('Ctrl Pts',(-0.737337443611625,-2.33838479904505,
19.7032338868201));
#5729=CARTESIAN_POINT('Ctrl Pts',(-0.658450154460479,-2.36180828715453,
19.7074940516857));
#5730=CARTESIAN_POINT('Ctrl Pts',(-0.578646273066033,-2.38120111302401,
19.7117542165512));
#5731=CARTESIAN_POINT('Ctrl Pts',(-0.499564152315685,-2.40041854669144,
19.7159758517202));
#5732=CARTESIAN_POINT('Ctrl Pts',(-0.419582425747597,-2.41567790543166,
19.7201974868892));
#5733=CARTESIAN_POINT('Ctrl Pts',(-0.339130454725297,-2.42692002024744,
19.7244191220581));
#5734=CARTESIAN_POINT('Ctrl Pts',(-0.257577089370006,-2.4383160405722,19.728698551772));
#5735=CARTESIAN_POINT('Ctrl Pts',(-0.175540999423107,-2.44558394767281,
19.7329779814859));
#5736=CARTESIAN_POINT('Ctrl Pts',(-0.0934713727919753,-2.44871667460088,
19.7372574111998));
#5737=CARTESIAN_POINT('Ctrl Pts',(-0.011401746160844,-2.45184940152895,
19.7415368409136));
#5738=CARTESIAN_POINT('Ctrl Pts',(0.0707009274029293,-2.45084701976013,
19.7458162706275));
#5739=CARTESIAN_POINT('Ctrl Pts',(0.152392883928873,-2.44575686831865,19.7500957003414));
#5740=CARTESIAN_POINT('Ctrl Pts',(0.233154654091345,-2.44072467594267,19.7543264022816));
#5741=CARTESIAN_POINT('Ctrl Pts',(0.313818783242086,-2.43167844719997,19.7585571042219));
#5742=CARTESIAN_POINT('Ctrl Pts',(0.393954141627843,-2.41862572224275,19.7627878061621));
#5743=CARTESIAN_POINT('Ctrl Pts',(0.473974367553377,-2.40559175045975,19.7670124297478));
#5744=CARTESIAN_POINT('Ctrl Pts',(0.553466876399462,-2.38856278878793,19.7712370533335));
#5745=CARTESIAN_POINT('Ctrl Pts',(0.632003614358565,-2.36759829393369,19.7754616769192));
#5746=CARTESIAN_POINT('Ctrl Pts',(0.710849457380148,-2.34655128697543,19.7797029277875));
#5747=CARTESIAN_POINT('Ctrl Pts',(0.788731516292138,-2.32153773094152,19.7839441786558));
#5748=CARTESIAN_POINT('Ctrl Pts',(0.865224970328596,-2.2926700592802,19.7881854295241));
#5749=CARTESIAN_POINT('Ctrl Pts',(0.94128103283131,-2.26396745370647,19.792402428811));
#5750=CARTESIAN_POINT('Ctrl Pts',(1.01596388804196,-2.23145485462082,19.796619428098));
#5751=CARTESIAN_POINT('Ctrl Pts',(1.08887096805657,-2.19529275153077,19.8008364273849));
#5752=CARTESIAN_POINT('Ctrl Pts',(1.16175387777927,-2.15914263696897,19.8050520286444));
#5753=CARTESIAN_POINT('Ctrl Pts',(1.23286176508415,-2.11934562752396,19.8092676299038));
#5754=CARTESIAN_POINT('Ctrl Pts',(1.30181397541562,-2.07610949215415,19.8134832311632));
#5755=CARTESIAN_POINT('Ctrl Pts',(1.37076446521134,-2.03287443563761,19.8176987272325));
#5756=CARTESIAN_POINT('Ctrl Pts',(1.43755899154933,-1.98620067179778,19.8219142233018));
#5757=CARTESIAN_POINT('Ctrl Pts',(1.50184459234358,-1.93634012261492,19.8261297193711));
#5758=CARTESIAN_POINT('Ctrl Pts',(1.56681138471259,-1.88595123449461,19.8303898842367));
#5759=CARTESIAN_POINT('Ctrl Pts',(1.62921537143732,-1.83230790661755,19.8346500491023));
#5760=CARTESIAN_POINT('Ctrl Pts',(1.6887268024599,-1.7757116986306,19.8389102139679));
#5761=CARTESIAN_POINT('Ctrl Pts',(1.74770000140581,-1.71962735691929,19.8431318491369));
#5762=CARTESIAN_POINT('Ctrl Pts',(1.80383247632686,-1.66064371619423,19.8473534843058));
#5763=CARTESIAN_POINT('Ctrl Pts',(1.85684201911488,-1.59908973045586,19.8515751194748));
#5764=CARTESIAN_POINT('Ctrl Pts',(1.9105772670573,-1.53669306541155,19.8558545491887));
#5765=CARTESIAN_POINT('Ctrl Pts',(1.96110312556306,-1.47165553663221,19.8601339789026));
#5766=CARTESIAN_POINT('Ctrl Pts',(2.00817045738781,-1.40435097610064,19.8644134086165));
#5767=CARTESIAN_POINT('Ctrl Pts',(2.05523778921256,-1.33704641556908,19.8686928383304));
#5768=CARTESIAN_POINT('Ctrl Pts',(2.09884638929266,-1.2674752737454,19.8729722680443));
#5769=CARTESIAN_POINT('Ctrl Pts',(2.13879579919823,-1.19603627843473,19.8772516977581));
#5770=CARTESIAN_POINT('Ctrl Pts',(2.17829032470731,-1.12541072403208,19.8814823996984));
#5771=CARTESIAN_POINT('Ctrl Pts',(2.21435715494294,-1.05269401520356,19.8857131016387));
#5772=CARTESIAN_POINT('Ctrl Pts',(2.24676921058904,-0.978252709860344,19.8899438035789));
#5773=CARTESIAN_POINT('Ctrl Pts',(2.27913469902963,-0.903918356189735,19.8941684271646));
#5774=CARTESIAN_POINT('Ctrl Pts',(2.3078556573884,-0.827864749771428,19.8983930507503));
#5775=CARTESIAN_POINT('Ctrl Pts',(2.33275032093623,-0.750483970629553,19.9026176743359));
#5776=CARTESIAN_POINT('Ctrl Pts',(2.35774296495447,-0.67279863605048,19.9068589252042));
#5777=CARTESIAN_POINT('Ctrl Pts',(2.37887889886256,-0.593776073553013,19.9111001760725));
#5778=CARTESIAN_POINT('Ctrl Pts',(2.39602264893265,-0.513834327192877,19.9153414269408));
#5779=CARTESIAN_POINT('Ctrl Pts',(2.41306837059979,-0.434349689790429,19.9195584262278));
#5780=CARTESIAN_POINT('Ctrl Pts',(2.42616734086354,-0.353956811127188,19.9237754255147));
#5781=CARTESIAN_POINT('Ctrl Pts',(2.43523653745251,-0.273081044117545,19.9279924248017));
#5782=CARTESIAN_POINT('Ctrl Pts',(2.4443027274044,-0.192232089193979,19.9322080260611));
#5783=CARTESIAN_POINT('Ctrl Pts',(2.44934174488284,-0.110901025629182,19.9364236273205));
#5784=CARTESIAN_POINT('Ctrl Pts',(2.45032218231686,-0.0295203801798546,
19.94063922858));
#5785=CARTESIAN_POINT('Ctrl Pts',(2.45130259528643,0.0518582346122204,19.9448547246493));
#5786=CARTESIAN_POINT('Ctrl Pts',(2.44822462504793,0.133285963789158,19.9490702207186));
#5787=CARTESIAN_POINT('Ctrl Pts',(2.44110897904676,0.21432965827732,19.9532857167879));
#5788=CARTESIAN_POINT('Ctrl Pts',(2.43391793329751,0.296232118666215,19.9575458816535));
#5789=CARTESIAN_POINT('Ctrl Pts',(2.42260315950359,0.377741873167508,19.961806046519));
#5790=CARTESIAN_POINT('Ctrl Pts',(2.407239665619,0.458418413974113,19.9660662113846));
#5791=CARTESIAN_POINT('Ctrl Pts',(2.392015121934,0.538365301647637,19.9702878465536));
#5792=CARTESIAN_POINT('Ctrl Pts',(2.37281496915214,0.617493544058887,19.9745094817226));
#5793=CARTESIAN_POINT('Ctrl Pts',(2.34976298701108,0.695387773025081,19.9787311168915));
#5794=CARTESIAN_POINT('Ctrl Pts',(2.32639542127166,0.774348380618402,19.9830105466054));
#5795=CARTESIAN_POINT('Ctrl Pts',(2.29906992801884,0.852040464809562,19.9872899763193));
#5796=CARTESIAN_POINT('Ctrl Pts',(2.26796592344903,0.928052164522017,19.9915694060332));
#5797=CARTESIAN_POINT('Ctrl Pts',(2.23686191887921,1.00406386423447,19.9958488357471));
#5798=CARTESIAN_POINT('Ctrl Pts',(2.20197967069624,1.07839476317501,20.000128265461));
#5799=CARTESIAN_POINT('Ctrl Pts',(2.16354588173326,1.15066044845343,20.0044076951749));
#5800=CARTESIAN_POINT('Ctrl Pts',(2.12554971953229,1.22210327970922,20.0086383971151));
#5801=CARTESIAN_POINT('Ctrl Pts',(2.08393960868892,1.29179642615617,20.0128690990553));
#5802=CARTESIAN_POINT('Ctrl Pts',(2.03890079209274,1.35935051035544,20.0170998009956));
#5803=CARTESIAN_POINT('Ctrl Pts',(1.9939266838832,1.4268075379238,20.0213244245813));
#5804=CARTESIAN_POINT('Ctrl Pts',(1.94553390923101,1.49213122321264,20.0255490481669));
#5805=CARTESIAN_POINT('Ctrl Pts',(1.89395370278847,1.55495646938873,20.0297736717526));
#5806=CARTESIAN_POINT('Ctrl Pts',(1.84217048685824,1.61802898330412,20.0340149226209));
#5807=CARTESIAN_POINT('Ctrl Pts',(1.78717491795365,1.67858293021672,20.0382561734892));
#5808=CARTESIAN_POINT('Ctrl Pts',(1.72924512267837,1.73627807556655,20.0424974243575));
#5809=CARTESIAN_POINT('Ctrl Pts',(1.67164657145958,1.79364331859418,20.0467144236444));
#5810=CARTESIAN_POINT('Ctrl Pts',(1.61114759160327,1.84818203326596,20.0509314229314));
#5811=CARTESIAN_POINT('Ctrl Pts',(1.54806085253091,1.89959412687586,20.0551484222183));
#5812=CARTESIAN_POINT('Ctrl Pts',(1.48499502809271,1.95098917625198,20.0593640234777));
#5813=CARTESIAN_POINT('Ctrl Pts',(1.41934350830265,1.99925936940418,20.0635796247372));
#5814=CARTESIAN_POINT('Ctrl Pts',(1.35145293885435,2.04414412507091,20.0677952259966));
#5815=CARTESIAN_POINT('Ctrl Pts',(1.28356406345103,2.08902776074712,20.0720107220659));
#5816=CARTESIAN_POINT('Ctrl Pts',(1.21343663801286,2.13052587131964,20.0762262181352));
#5817=CARTESIAN_POINT('Ctrl Pts',(1.14144604713833,2.16842135468923,20.0804417142045));
#5818=CARTESIAN_POINT('Ctrl Pts',(1.06869262005518,2.2067183911855,20.0847018790701));
#5819=CARTESIAN_POINT('Ctrl Pts',(0.994036728186423,2.24133575668558,20.0889620439356));
#5820=CARTESIAN_POINT('Ctrl Pts',(0.917889341979701,2.27209801854587,20.0932222088012));
#5821=CARTESIAN_POINT('Ctrl Pts',(0.842430646418192,2.30258206098165,20.0974438439702));
#5822=CARTESIAN_POINT('Ctrl Pts',(0.765507791157719,2.32928035591761,20.1016654791391));
#5823=CARTESIAN_POINT('Ctrl Pts',(0.68753701593911,2.35207208684461,20.1058871143081));
#5824=CARTESIAN_POINT('Ctrl Pts',(0.608498814168257,2.37517583850879,20.110166544022));
#5825=CARTESIAN_POINT('Ctrl Pts',(0.528384264147741,2.39426513924305,20.1144459737359));
#5826=CARTESIAN_POINT('Ctrl Pts',(0.447636779230287,2.40926784809833,20.1187254034498));
#5827=CARTESIAN_POINT('Ctrl Pts',(0.366889294312832,2.4242705569536,20.1230048331637));
#5828=CARTESIAN_POINT('Ctrl Pts',(0.285509369438124,2.43518667361783,20.1272842628776));
#5829=CARTESIAN_POINT('Ctrl Pts',(0.203942942235041,2.4419986745108,20.1315636925915));
#5830=CARTESIAN_POINT('Ctrl Pts',(0.123305272055105,2.44873311048046,20.1357943945318));
#5831=CARTESIAN_POINT('Ctrl Pts',(0.0421820279336449,2.4514817918581,20.1400250964721));
#5832=CARTESIAN_POINT('Ctrl Pts',(-0.0389991254234243,2.45018964943863,
20.1442557984123));
#5833=CARTESIAN_POINT('Ctrl Pts',(-0.120063643800722,2.44889936347227,20.148480421998));
#5834=CARTESIAN_POINT('Ctrl Pts',(-0.201185445118454,2.44357979119288,20.1527050455837));
#5835=CARTESIAN_POINT('Ctrl Pts',(-0.281932378287374,2.43422767712333,20.1569296691694));
#5836=CARTESIAN_POINT('Ctrl Pts',(-0.362997115409843,2.42483875498307,20.1611709200377));
#5837=CARTESIAN_POINT('Ctrl Pts',(-0.443683554332787,2.4113854409016,20.1654121709059));
#5838=CARTESIAN_POINT('Ctrl Pts',(-0.52355505925226,2.39391736489198,20.1696534217742));
#5839=CARTESIAN_POINT('Ctrl Pts',(-0.60296985685643,2.37654917178936,20.1738704210612));
#5840=CARTESIAN_POINT('Ctrl Pts',(-0.681578555905518,2.35521210555354,20.1780874203482));
#5841=CARTESIAN_POINT('Ctrl Pts',(-0.758959568270523,2.33000657160675,20.1823044196351));
#5842=CARTESIAN_POINT('Ctrl Pts',(-0.836314927137037,2.30480939384589,20.1865200208946));
#5843=CARTESIAN_POINT('Ctrl Pts',(-0.912442965719734,2.2757464390876,20.190735622154));
#5844=CARTESIAN_POINT('Ctrl Pts',(-0.986936920277564,2.24296807052464,20.1949512234135));
#5845=CARTESIAN_POINT('Ctrl Pts',(-1.06142901601894,2.21019051986659,20.1991667194828));
#5846=CARTESIAN_POINT('Ctrl Pts',(-1.13428668356774,2.17369792802846,20.2033822155521));
#5847=CARTESIAN_POINT('Ctrl Pts',(-1.20512415503216,2.13368836078702,20.2075977116214));
#5848=CARTESIAN_POINT('Ctrl Pts',(-1.27671224386866,2.09325483888431,20.211857876487));
#5849=CARTESIAN_POINT('Ctrl Pts',(-1.34623663860525,2.04922958793242,20.2161180413525));
#5850=CARTESIAN_POINT('Ctrl Pts',(-1.41332733865816,2.00186315311548,20.2203782062181));
#5851=CARTESIAN_POINT('Ctrl Pts',(-1.47981125836325,1.954925108847,20.2245998413871));
#5852=CARTESIAN_POINT('Ctrl Pts',(-1.54390499578371,1.90470641275263,20.2288214765561));
#5853=CARTESIAN_POINT('Ctrl Pts',(-1.60528161640392,1.85149161003652,20.233043111725));
#5854=CARTESIAN_POINT('Ctrl Pts',(-1.66749848818651,1.7975482921401,20.2373225414389));
#5855=CARTESIAN_POINT('Ctrl Pts',(-1.72692292784225,1.74052655506493,20.2416019711528));
#5856=CARTESIAN_POINT('Ctrl Pts',(-1.78325421308347,1.68076014395869,20.2458814008667));
#5857=CARTESIAN_POINT('Ctrl Pts',(-1.8395854983247,1.62099373285245,20.2501608305806));
#5858=CARTESIAN_POINT('Ctrl Pts',(-1.89282336092282,1.55848306367045,20.2544402602945));
#5859=CARTESIAN_POINT('Ctrl Pts',(-1.94271163188089,1.49359357435504,20.2587196900084));
#5860=CARTESIAN_POINT('Ctrl Pts',(-1.99209745833045,1.42935761275148,20.262956019893));
#5861=CARTESIAN_POINT('Ctrl Pts',(-2.03838923801818,1.3625456306175,20.2671923497777));
#5862=CARTESIAN_POINT('Ctrl Pts',(-2.08130749356415,1.29348728916589,20.2714286796623));
#5863=CARTESIAN_POINT('Ctrl Pts',(-2.1241647396303,1.22452711604464,20.2756589874876));
#5864=CARTESIAN_POINT('Ctrl Pts',(-2.16365774029402,1.15332731246913,20.2798892953129));
#5865=CARTESIAN_POINT('Ctrl Pts',(-2.19954791923293,1.08024960124876,20.2841196031382));
#5866=CARTESIAN_POINT('Ctrl Pts',(-2.23539796364722,1.007253609855,20.2883451803826));
#5867=CARTESIAN_POINT('Ctrl Pts',(-2.26765298493047,0.932384294424062,20.292570757627));
#5868=CARTESIAN_POINT('Ctrl Pts',(-2.29611906075136,0.856030086418862,20.2967963348715));
#5869=CARTESIAN_POINT('Ctrl Pts',(-2.32456236915141,0.779736947188911,20.3010185324616));
#5870=CARTESIAN_POINT('Ctrl Pts',(-2.34922259155999,0.701961707252038,20.3052407300517));
#5871=CARTESIAN_POINT('Ctrl Pts',(-2.36995348616987,0.623113732308394,20.3094629276419));
#5872=CARTESIAN_POINT('Ctrl Pts',(-2.39067451838823,0.54430326802761,20.313683116589));
#5873=CARTESIAN_POINT('Ctrl Pts',(-2.4074698210759,0.46442153025925,20.3179033055362));
#5874=CARTESIAN_POINT('Ctrl Pts',(-2.42024309441087,0.383892711517824,20.3221234944834));
#5875=CARTESIAN_POINT('Ctrl Pts',(-2.43301721239666,0.303358567693985,20.3263439624965));
#5876=CARTESIAN_POINT('Ctrl Pts',(-2.44176868987456,0.222177713509171,20.3305644305097));
#5877=CARTESIAN_POINT('Ctrl Pts',(-2.44645260879332,0.14078310597631,20.3347848985228));
#5878=CARTESIAN_POINT('Ctrl Pts',(-2.44918555562594,0.0932914352820124,
20.3372474336112));
#5879=CARTESIAN_POINT('Ctrl Pts',(-2.45053470395961,0.0457271215552733,
20.3397099686996));
#5880=CARTESIAN_POINT('Ctrl Pts',(-2.45049932159773,-0.0018234168666027,
20.342172503788));
#5881=CARTESIAN_POINT('',(-2.45075217663585,-0.000775521780153733,21.142172503788));
#5882=CARTESIAN_POINT('Ctrl Pts',(-2.45049932159731,-0.00182341742446744,
20.3421725038169));
#5883=CARTESIAN_POINT('Ctrl Pts',(-2.45042940194528,-0.0957887692889192,
20.3470387573598));
#5884=CARTESIAN_POINT('Ctrl Pts',(-2.44495079787555,-0.189533578807969,
20.3519050109027));
#5885=CARTESIAN_POINT('Ctrl Pts',(-2.43416311526865,-0.282489253363092,
20.3567712644456));
#5886=CARTESIAN_POINT('Ctrl Pts',(-2.4232718287915,-0.376337665311091,20.3616842530213));
#5887=CARTESIAN_POINT('Ctrl Pts',(-2.40696909966942,-0.469381553096781,
20.366597241597));
#5888=CARTESIAN_POINT('Ctrl Pts',(-2.38540708047413,-0.561055532388618,
20.3715102301727));
#5889=CARTESIAN_POINT('Ctrl Pts',(-2.36439147661448,-0.650406349470546,
20.3762987159235));
#5890=CARTESIAN_POINT('Ctrl Pts',(-2.338380089688,-0.7384557897747,20.3810872016743));
#5891=CARTESIAN_POINT('Ctrl Pts',(-2.30755712572132,-0.824700164625149,
20.385875687425));
#5892=CARTESIAN_POINT('Ctrl Pts',(-2.28032455570955,-0.900898416641911,
20.3901063893653));
#5893=CARTESIAN_POINT('Ctrl Pts',(-2.24926248145955,-0.975889639657493,
20.3943370913055));
#5894=CARTESIAN_POINT('Ctrl Pts',(-2.21449771314159,-1.04926170638724,20.3985677932458));
#5895=CARTESIAN_POINT('Ctrl Pts',(-2.17978289222991,-1.12252835764599,20.4027924168314));
#5896=CARTESIAN_POINT('Ctrl Pts',(-2.14137614001279,-1.19418005603748,20.4070170404171));
#5897=CARTESIAN_POINT('Ctrl Pts',(-2.0994532936976,-1.26382202765355,20.4112416640028));
#5898=CARTESIAN_POINT('Ctrl Pts',(-2.05736544735351,-1.33373809629161,20.4154829148711));
#5899=CARTESIAN_POINT('Ctrl Pts',(-2.01173392995459,-1.40162813757682,20.4197241657394));
#5900=CARTESIAN_POINT('Ctrl Pts',(-1.96278458077881,-1.46711517593437,20.4239654166076));
#5901=CARTESIAN_POINT('Ctrl Pts',(-1.91411512523816,-1.53222775772554,20.4281824158946));
#5902=CARTESIAN_POINT('Ctrl Pts',(-1.86216595908491,-1.59496436663692,20.4323994151815));
#5903=CARTESIAN_POINT('Ctrl Pts',(-1.80720292121011,-1.65498273452313,20.4366164144685));
#5904=CARTESIAN_POINT('Ctrl Pts',(-1.75225810478478,-1.71498120500737,20.4408320157279));
#5905=CARTESIAN_POINT('Ctrl Pts',(-1.69430171464561,-1.77226288130747,20.4450476169874));
#5906=CARTESIAN_POINT('Ctrl Pts',(-1.63363893730903,-1.82651966113366,20.4492632182468));
#5907=CARTESIAN_POINT('Ctrl Pts',(-1.57297767366546,-1.88077508711303,20.4534787143161));
#5908=CARTESIAN_POINT('Ctrl Pts',(-1.50961050445715,-1.93200545746302,20.4576942103854));
#5909=CARTESIAN_POINT('Ctrl Pts',(-1.44387735730175,-1.97994152112413,20.4619097064547));
#5910=CARTESIAN_POINT('Ctrl Pts',(-1.3774476798894,-2.02838553123513,20.4661698713203));
#5911=CARTESIAN_POINT('Ctrl Pts',(-1.30860196654479,-2.07346470535092,20.4704300361859));
#5912=CARTESIAN_POINT('Ctrl Pts',(-1.23772139805952,-2.11494586001287,20.4746902010515));
#5913=CARTESIAN_POINT('Ctrl Pts',(-1.16748188617345,-2.15605185165756,20.4789118362204));
#5914=CARTESIAN_POINT('Ctrl Pts',(-1.09524462394142,-2.19362448211044,20.4831334713894));
#5915=CARTESIAN_POINT('Ctrl Pts',(-1.02140392707523,-2.22748384231071,20.4873551065583));
#5916=CARTESIAN_POINT('Ctrl Pts',(-0.946552344781212,-2.26180674003535,
20.4916345362722));
#5917=CARTESIAN_POINT('Ctrl Pts',(-0.870053552593081,-2.29231374449783,
20.4959139659862));
#5918=CARTESIAN_POINT('Ctrl Pts',(-0.792335812250154,-2.31886916634507,
20.5001933957001));
#5919=CARTESIAN_POINT('Ctrl Pts',(-0.714618071907238,-2.34542458819231,
20.504472825414));
#5920=CARTESIAN_POINT('Ctrl Pts',(-0.635681873070596,-2.36802835533114,
20.5087522551279));
#5921=CARTESIAN_POINT('Ctrl Pts',(-0.55596589658677,-2.3865984521558,20.5130316848418));
#5922=CARTESIAN_POINT('Ctrl Pts',(-0.477157606948787,-2.40495710036806,
20.517262386782));
#5923=CARTESIAN_POINT('Ctrl Pts',(-0.397290797063437,-2.41944256428234,
20.5214930887223));
#5924=CARTESIAN_POINT('Ctrl Pts',(-0.316780622574167,-2.42993832990912,
20.5257237906625));
#5925=CARTESIAN_POINT('Ctrl Pts',(-0.236386119052694,-2.44041901600868,
20.5299484142482));
#5926=CARTESIAN_POINT('Ctrl Pts',(-0.155350543958637,-2.44692132847492,
20.5341730378339));
#5927=CARTESIAN_POINT('Ctrl Pts',(-0.0741010067723045,-2.44937936849222,
20.5383976614195));
#5928=CARTESIAN_POINT('Ctrl Pts',(0.00746831251776109,-2.45184708286871,
20.5426389122878));
#5929=CARTESIAN_POINT('Ctrl Pts',(0.0892528195580796,-2.45023851393666,
20.5468801631561));
#5930=CARTESIAN_POINT('Ctrl Pts',(0.170813297237658,-2.44453943872599,20.5511214140244));
#5931=CARTESIAN_POINT('Ctrl Pts',(0.251907410012081,-2.43887295097369,20.5553384133114));
#5932=CARTESIAN_POINT('Ctrl Pts',(0.332779579891918,-2.42916264198655,20.5595554125983));
#5933=CARTESIAN_POINT('Ctrl Pts',(0.412998114034193,-2.41544670978355,20.5637724118853));
#5934=CARTESIAN_POINT('Ctrl Pts',(0.493190053977476,-2.40173532471214,20.5679880131447));
#5935=CARTESIAN_POINT('Ctrl Pts',(0.572728330457082,-2.38402103182902,20.5722036144041));
#5936=CARTESIAN_POINT('Ctrl Pts',(0.651188672559655,-2.36239360876421,20.5764192156636));
#5937=CARTESIAN_POINT('Ctrl Pts',(0.729647056874019,-2.34076672535947,20.5806347117328));
#5938=CARTESIAN_POINT('Ctrl Pts',(0.807027112238553,-2.31522703054067,20.5848502078021));
#5939=CARTESIAN_POINT('Ctrl Pts',(0.882918422960261,-2.28591454529634,20.5890657038714));
#5940=CARTESIAN_POINT('Ctrl Pts',(0.959613903213687,-2.25629145522376,20.593325868737));
#5941=CARTESIAN_POINT('Ctrl Pts',(1.03478844276558,-2.22281530269604,20.5975860336026));
#5942=CARTESIAN_POINT('Ctrl Pts',(1.10803961507263,-2.18568032004447,20.6018461984682));
#5943=CARTESIAN_POINT('Ctrl Pts',(1.1806282906134,-2.14888119284951,20.6060678336371));
#5944=CARTESIAN_POINT('Ctrl Pts',(1.25132787185416,-2.10848943841504,20.6102894688061));
#5945=CARTESIAN_POINT('Ctrl Pts',(1.31977361170098,-2.06473917574539,20.6145111039751));
#5946=CARTESIAN_POINT('Ctrl Pts',(1.38915637955478,-2.02038996825425,20.618790533689));
#5947=CARTESIAN_POINT('Ctrl Pts',(1.45622272539164,-1.9725898868357,20.6230699634029));
#5948=CARTESIAN_POINT('Ctrl Pts',(1.52062670138809,-1.92162553194569,20.6273493931168));
#5949=CARTESIAN_POINT('Ctrl Pts',(1.58503067738455,-1.87066117705569,20.6316288228307));
#5950=CARTESIAN_POINT('Ctrl Pts',(1.64677195781943,-1.81653292134836,20.6359082525446));
#5951=CARTESIAN_POINT('Ctrl Pts',(1.70554408044806,-1.7595651848251,20.6401876822585));
#5952=CARTESIAN_POINT('Ctrl Pts',(1.76364699365394,-1.70324611206228,20.6444183841988));
#5953=CARTESIAN_POINT('Ctrl Pts',(1.81906659342486,-1.64394009257578,20.648649086139));
#5954=CARTESIAN_POINT('Ctrl Pts',(1.87148014956412,-1.58193308954186,20.6528797880793));
#5955=CARTESIAN_POINT('Ctrl Pts',(1.92381840184519,-1.5200151735096,20.657104411665));
#5956=CARTESIAN_POINT('Ctrl Pts',(1.97315889030846,-1.45540433311518,20.6613290352506));
#5957=CARTESIAN_POINT('Ctrl Pts',(2.01921496789655,-1.38842398546789,20.6655536588363));
#5958=CARTESIAN_POINT('Ctrl Pts',(2.06545231309406,-1.32118001642399,20.6697949097046));
#5959=CARTESIAN_POINT('Ctrl Pts',(2.10837899763112,-1.25154817858745,20.6740361605729));
#5960=CARTESIAN_POINT('Ctrl Pts',(2.14774526609161,-1.17989004656411,20.6782774114412));
#5961=CARTESIAN_POINT('Ctrl Pts',(2.18688643721854,-1.1086416575791,20.6824944107281));
#5962=CARTESIAN_POINT('Ctrl Pts',(2.22250757270814,-1.0353904960309,20.6867114100151));
#5963=CARTESIAN_POINT('Ctrl Pts',(2.25440706421301,-0.960520191784876,20.690928409302));
#5964=CARTESIAN_POINT('Ctrl Pts',(2.28629598033859,-0.88567470868263,20.6951440105615));
#5965=CARTESIAN_POINT('Ctrl Pts',(2.31446552046467,-0.80921157634547,20.6993596118209));
#5966=CARTESIAN_POINT('Ctrl Pts',(2.33876146051047,-0.731536110408039,20.7035752130803));
#5967=CARTESIAN_POINT('Ctrl Pts',(2.36305679430983,-0.653862582674075,20.7077907091496));
#5968=CARTESIAN_POINT('Ctrl Pts',(2.38347858240881,-0.574977225664457,20.712006205219));
#5969=CARTESIAN_POINT('Ctrl Pts',(2.39992234458874,-0.495300908482584,20.7162217012882));
#5970=CARTESIAN_POINT('Ctrl Pts',(2.41654035033359,-0.414780314583919,20.7204818661538));
#5971=CARTESIAN_POINT('Ctrl Pts',(2.42909540951905,-0.333452369363806,20.7247420310194));
#5972=CARTESIAN_POINT('Ctrl Pts',(2.437532945941,-0.25176057565112,20.729002195885));
#5973=CARTESIAN_POINT('Ctrl Pts',(2.44589417176728,-0.170807617201268,20.733223831054));
#5974=CARTESIAN_POINT('Ctrl Pts',(2.4502120911814,-0.0894978380484811,20.7374454662229));
#5975=CARTESIAN_POINT('Ctrl Pts',(2.45048606309993,-0.00826465685841186,
20.7416671013919));
#5976=CARTESIAN_POINT('Ctrl Pts',(2.45076378571736,0.0740806134990697,20.7459465311058));
#5977=CARTESIAN_POINT('Ctrl Pts',(2.44688602179799,0.156346678644228,20.7502259608197));
#5978=CARTESIAN_POINT('Ctrl Pts',(2.43890643258138,0.238087511459872,20.7545053905336));
#5979=CARTESIAN_POINT('Ctrl Pts',(2.43092684336478,0.319828344275527,20.7587848202475));
#5980=CARTESIAN_POINT('Ctrl Pts',(2.4188455658134,0.401043469149773,20.7630642499614));
#5981=CARTESIAN_POINT('Ctrl Pts',(2.40276943619427,0.4812995808129,20.7673436796753));
#5982=CARTESIAN_POINT('Ctrl Pts',(2.38687635760234,0.560641855375478,20.7715743816155));
#5983=CARTESIAN_POINT('Ctrl Pts',(2.36701920340017,0.639345282321904,20.7758050835558));
#5984=CARTESIAN_POINT('Ctrl Pts',(2.34326366932778,0.716983699960119,20.780035785496));
#5985=CARTESIAN_POINT('Ctrl Pts',(2.31954226542135,0.794510572554981,20.7842604090817));
#5986=CARTESIAN_POINT('Ctrl Pts',(2.29193374025465,0.870975033819044,20.7884850326674));
#5987=CARTESIAN_POINT('Ctrl Pts',(2.2605548150828,0.945960981228063,20.7927096562531));
#5988=CARTESIAN_POINT('Ctrl Pts',(2.2290523886697,1.02124205849034,20.7969509071214));
#5989=CARTESIAN_POINT('Ctrl Pts',(2.19374991270405,1.09503249334827,20.8011921579897));
#5990=CARTESIAN_POINT('Ctrl Pts',(2.15481616321484,1.16692654128188,20.805433408858));
#5991=CARTESIAN_POINT('Ctrl Pts',(2.11610503790453,1.23840949720407,20.8096504081449));
#5992=CARTESIAN_POINT('Ctrl Pts',(2.07380427750083,1.30801728147431,20.8138674074319));
#5993=CARTESIAN_POINT('Ctrl Pts',(2.02812726855146,1.37537268860408,20.8180844067189));
#5994=CARTESIAN_POINT('Ctrl Pts',(1.98246540252982,1.44270576594285,20.8223000079783));
#5995=CARTESIAN_POINT('Ctrl Pts',(1.93342977151677,1.50778756438828,20.8265156092377));
#5996=CARTESIAN_POINT('Ctrl Pts',(1.88127764893699,1.57026897619806,20.8307312104972));
#5997=CARTESIAN_POINT('Ctrl Pts',(1.82912682768737,1.63274882893525,20.8349467065665));
#5998=CARTESIAN_POINT('Ctrl Pts',(1.77385996832765,1.69262806770978,20.8391622026358));
#5999=CARTESIAN_POINT('Ctrl Pts',(1.71577435289462,1.74959098647343,20.8433776987051));
#6000=CARTESIAN_POINT('Ctrl Pts',(1.65707324299081,1.8071575032411,20.8476378635707));
#6001=CARTESIAN_POINT('Ctrl Pts',(1.59549361899103,1.86174517669302,20.8518980284363));
#6002=CARTESIAN_POINT('Ctrl Pts',(1.53137881103169,1.91306800378951,20.8561581933018));
#6003=CARTESIAN_POINT('Ctrl Pts',(1.46784386891713,1.96392665801488,20.8603798284708));
#6004=CARTESIAN_POINT('Ctrl Pts',(1.40181983312183,2.01157905891197,20.8646014636398));
#6005=CARTESIAN_POINT('Ctrl Pts',(1.33367075655938,2.055790009485,20.8688230988088));
#6006=CARTESIAN_POINT('Ctrl Pts',(1.26458871333628,2.10060621173568,20.8731025285226));
#6007=CARTESIAN_POINT('Ctrl Pts',(1.19332343285252,2.1418857747785,20.8773819582365));
#6008=CARTESIAN_POINT('Ctrl Pts',(1.12027896859314,2.17943233033923,20.8816613879504));
#6009=CARTESIAN_POINT('Ctrl Pts',(1.04723450433375,2.21697888589997,20.8859408176643));
#6010=CARTESIAN_POINT('Ctrl Pts',(0.972411330326129,2.25079229162891,20.8902202473782));
#6011=CARTESIAN_POINT('Ctrl Pts',(0.896231593656129,2.28072777431516,20.894499677092));
#6012=CARTESIAN_POINT('Ctrl Pts',(0.820919278397737,2.31032239629771,20.8987303790323));
#6013=CARTESIAN_POINT('Ctrl Pts',(0.74399788158306,2.33623831222166,20.9029610809726));
#6014=CARTESIAN_POINT('Ctrl Pts',(0.665861270312645,2.3583000272861,20.9071917829128));
#6015=CARTESIAN_POINT('Ctrl Pts',(0.587836919852729,2.38033004573645,20.9114164064985));
#6016=CARTESIAN_POINT('Ctrl Pts',(0.508601266212819,2.39851673566404,20.9156410300842));
#6017=CARTESIAN_POINT('Ctrl Pts',(0.428567344990767,2.41273294850623,20.9198656536698));
#6018=CARTESIAN_POINT('Ctrl Pts',(0.348218426089122,2.42700511354956,20.9241069045381));
#6019=CARTESIAN_POINT('Ctrl Pts',(0.267065384158193,2.43727530688718,20.9283481554064));
#6020=CARTESIAN_POINT('Ctrl Pts',(0.18554072929708,2.44346575334542,20.9325894062747));
#6021=CARTESIAN_POINT('Ctrl Pts',(0.10448223450514,2.44962080267191,20.9368064055617));
#6022=CARTESIAN_POINT('Ctrl Pts',(0.0230568334225161,2.45174259914223,20.9410234048486));
#6023=CARTESIAN_POINT('Ctrl Pts',(-0.0583028055937678,2.44980632558166,
20.9452404041356));
#6024=CARTESIAN_POINT('Ctrl Pts',(-0.139635472109807,2.44787069393813,20.949456005395));
#6025=CARTESIAN_POINT('Ctrl Pts',(-0.220901955293346,2.44187967493463,20.9536716066544));
#6026=CARTESIAN_POINT('Ctrl Pts',(-0.30166944930381,2.43186056207109,20.9578872079139));
#6027=CARTESIAN_POINT('Ctrl Pts',(-0.382434927956733,2.42184169921029,20.9621027039832));
#6028=CARTESIAN_POINT('Ctrl Pts',(-0.462700980802887,2.40779500065897,20.9663182000525));
#6029=CARTESIAN_POINT('Ctrl Pts',(-0.542041223590698,2.38979948153152,20.9705336961218));
#6030=CARTESIAN_POINT('Ctrl Pts',(-0.622222181939403,2.3716132759072,20.9747938609873));
#6031=CARTESIAN_POINT('Ctrl Pts',(-0.701457116992228,2.34939415684168,20.9790540258529));
#6032=CARTESIAN_POINT('Ctrl Pts',(-0.779319686538854,2.3232759362962,20.9833141907185));
#6033=CARTESIAN_POINT('Ctrl Pts',(-0.856478053014138,2.29739393363093,20.9875358258875));
#6034=CARTESIAN_POINT('Ctrl Pts',(-0.932288362688646,2.26768330319341,20.9917574610564));
#6035=CARTESIAN_POINT('Ctrl Pts',(-1.00635576935863,2.23432278676976,20.9959790962254));
#6036=CARTESIAN_POINT('Ctrl Pts',(-1.0814371651327,2.20050556203565,21.0002585259393));
#6037=CARTESIAN_POINT('Ctrl Pts',(-1.15472713540308,2.16293798578629,21.0045379556532));
#6038=CARTESIAN_POINT('Ctrl Pts',(-1.22584182272251,2.12185345291901,21.0088173853671));
#6039=CARTESIAN_POINT('Ctrl Pts',(-1.29695651004194,2.08076892005174,21.013096815081));
#6040=CARTESIAN_POINT('Ctrl Pts',(-1.36589553808481,2.03616775203882,21.0173762447949));
#6041=CARTESIAN_POINT('Ctrl Pts',(-1.43230863225167,1.98832649028709,21.0216556745088));
#6042=CARTESIAN_POINT('Ctrl Pts',(-1.49744651369032,1.94140383934071,21.0258529339321));
#6043=CARTESIAN_POINT('Ctrl Pts',(-1.56040816290392,1.89118166509473,21.0300501933555));
#6044=CARTESIAN_POINT('Ctrl Pts',(-1.62083593804574,1.83789039715087,21.0342474527789));
#6045=CARTESIAN_POINT('Ctrl Pts',(-1.68117667131803,1.78467589145055,21.0384386663516));
#6046=CARTESIAN_POINT('Ctrl Pts',(-1.73899042455939,1.72840137849704,21.0426298799243));
#6047=CARTESIAN_POINT('Ctrl Pts',(-1.79394951889461,1.66933980173534,21.046821093497));
#6048=CARTESIAN_POINT('Ctrl Pts',(-1.84884541217999,1.6103461437358,21.0510074873196));
#6049=CARTESIAN_POINT('Ctrl Pts',(-1.90089284763766,1.54857213380643,21.0551938811423));
#6050=CARTESIAN_POINT('Ctrl Pts',(-1.94979936015366,1.48432904207401,21.0593802749649));
#6051=CARTESIAN_POINT('Ctrl Pts',(-1.9986756118002,1.42012570070844,21.0635640784594));
#6052=CARTESIAN_POINT('Ctrl Pts',(-2.04441451086866,1.35345668447912,21.0677478819538));
#6053=CARTESIAN_POINT('Ctrl Pts',(-2.08676327369869,1.2846669955838,21.0719316854483));
#6054=CARTESIAN_POINT('Ctrl Pts',(-2.12909933263255,1.21589794240503,21.0761142338741));
#6055=CARTESIAN_POINT('Ctrl Pts',(-2.16804702656771,1.145009882353,21.0802967822999));
#6056=CARTESIAN_POINT('Ctrl Pts',(-2.20339726727559,1.07237620850262,21.0844793307257));
#6057=CARTESIAN_POINT('Ctrl Pts',(-2.23874817182219,0.999741170671587,21.0886619576952));
#6058=CARTESIAN_POINT('Ctrl Pts',(-2.27050128388474,0.92536088040813,21.0928445846646));
#6059=CARTESIAN_POINT('Ctrl Pts',(-2.29849448721701,0.849631297818651,21.0970272116341));
#6060=CARTESIAN_POINT('Ctrl Pts',(-2.32651476312671,0.773828476201683,21.1012138836745));
#6061=CARTESIAN_POINT('Ctrl Pts',(-2.35076770707166,0.696674202014863,21.1054005557149));
#6062=CARTESIAN_POINT('Ctrl Pts',(-2.37114045908625,0.618581581753182,21.1095872277552));
#6063=CARTESIAN_POINT('Ctrl Pts',(-2.39152389618704,0.540448003530648,21.1137760956183));
#6064=CARTESIAN_POINT('Ctrl Pts',(-2.40802299471514,0.461375563096551,21.1179649634814));
#6065=CARTESIAN_POINT('Ctrl Pts',(-2.42057614060237,0.38178711024148,21.1221538313445));
#6066=CARTESIAN_POINT('Ctrl Pts',(-2.43314987512159,0.302068122986412,21.1263495694423));
#6067=CARTESIAN_POINT('Ctrl Pts',(-2.4417646874607,0.221831904192904,21.1305453075402));
#6068=CARTESIAN_POINT('Ctrl Pts',(-2.44641093600422,0.141505414026922,21.134741045638));
#6069=CARTESIAN_POINT('Ctrl Pts',(-2.44915406890088,0.0940808659031447,
21.1372181983547));
#6070=CARTESIAN_POINT('Ctrl Pts',(-2.45051487677001,0.0466248548191888,
21.1396953510713));
#6071=CARTESIAN_POINT('Ctrl Pts',(-2.45049987730867,-0.000775441941961462,
21.142172503788));
#6072=CARTESIAN_POINT('',(-2.45034181611172,0.00225396750469473,21.942172503788));
#6073=CARTESIAN_POINT('Ctrl Pts',(-2.45424120969512,-0.000776625857978041,
21.142172503788));
#6074=CARTESIAN_POINT('Ctrl Pts',(-2.4544169492817,-0.0431881484021115,
21.1443855598339));
#6075=CARTESIAN_POINT('Ctrl Pts',(-2.45341298330889,-0.0855911780851724,
21.1465986158797));
#6076=CARTESIAN_POINT('Ctrl Pts',(-2.40888059246768,-0.938845702385758,
21.1911970043977));
#6077=CARTESIAN_POINT('Ctrl Pts',(-1.43961468312248,-2.51450512838468,21.2759676693421));
#6078=CARTESIAN_POINT('Ctrl Pts',(1.33466465959828,-2.57174973956534,21.403123666759));
#6079=CARTESIAN_POINT('Ctrl Pts',(2.8848211986208,-0.270246421845255,21.5302796641756));
#6080=CARTESIAN_POINT('Ctrl Pts',(1.78908808406994,2.27912051106948,21.6574356615925));
#6081=CARTESIAN_POINT('Ctrl Pts',(-0.947554232492991,2.73813211022012,21.7845916590091));
#6082=CARTESIAN_POINT('Ctrl Pts',(-2.3415517179439,1.2062176692426,21.879503939741));
#6083=CARTESIAN_POINT('Ctrl Pts',(-2.45213225552358,0.197415099304688,21.9320308880006));
#6084=CARTESIAN_POINT('Ctrl Pts',(-2.45034181611172,0.00225396750469473,
21.942172503788));
#6085=CARTESIAN_POINT('',(-2.45013029362686,-0.000414097013525958,22.742172523057));
#6086=CARTESIAN_POINT('Ctrl Pts',(-2.45034181611172,0.00225396750469473,
21.942172503788));
#6087=CARTESIAN_POINT('Ctrl Pts',(-2.44464938777012,-0.618231009799729,
21.9744162204729));
#6088=CARTESIAN_POINT('Ctrl Pts',(-1.89007733222012,-2.06341747834654,22.0490452696298));
#6089=CARTESIAN_POINT('Ctrl Pts',(0.540405455967006,-2.84660998728302,22.1660596512595));
#6090=CARTESIAN_POINT('Ctrl Pts',(2.68589067766831,-1.08683841676111,22.293215648676));
#6091=CARTESIAN_POINT('Ctrl Pts',(2.36794060637167,1.66975559925104,22.4203716460929));
#6092=CARTESIAN_POINT('Ctrl Pts',(-0.121828485691317,2.89488934099512,22.5475276435095));
#6093=CARTESIAN_POINT('Ctrl Pts',(-2.12790080642062,1.68857040030348,22.6547945960747));
#6094=CARTESIAN_POINT('Ctrl Pts',(-2.44587090828161,0.434202251858068,22.7196762161674));
#6095=CARTESIAN_POINT('Ctrl Pts',(-2.44652397570074,-0.000413115186416297,
22.742172503788));
#6096=CARTESIAN_POINT('',(-2.45049912112546,-0.00207541883967445,23.542172503788));
#6097=CARTESIAN_POINT('Ctrl Pts',(-2.45049996499496,-0.000414197657279032,
22.7421725250322));
#6098=CARTESIAN_POINT('Ctrl Pts',(-2.45048532431713,-0.0870322165490495,
22.7466487192745));
#6099=CARTESIAN_POINT('Ctrl Pts',(-2.44587388563628,-0.173537469021683,
22.7511249135167));
#6100=CARTESIAN_POINT('Ctrl Pts',(-2.43672683137232,-0.259446717593862,
22.7556011077589));
#6101=CARTESIAN_POINT('Ctrl Pts',(-2.42754837478386,-0.345650897192244,
22.7600926690144));
#6102=CARTESIAN_POINT('Ctrl Pts',(-2.41380320605056,-0.431254610293177,
22.7645842302699));
#6103=CARTESIAN_POINT('Ctrl Pts',(-2.39560398952757,-0.515782682299014,
22.7690757915254));
#6104=CARTESIAN_POINT('Ctrl Pts',(-2.37737168474098,-0.600464436037548,
22.7735755189546));
#6105=CARTESIAN_POINT('Ctrl Pts',(-2.35466927232878,-0.684066288703808,
22.7780752463837));
#6106=CARTESIAN_POINT('Ctrl Pts',(-2.32765907930728,-0.766128879835755,
22.7825749738129));
#6107=CARTESIAN_POINT('Ctrl Pts',(-2.30057021386355,-0.848430494169568,
22.7870878075703));
#6108=CARTESIAN_POINT('Ctrl Pts',(-2.26914861576414,-0.929183536036788,
22.7916006413278));
#6109=CARTESIAN_POINT('Ctrl Pts',(-2.23360485339984,-1.00794821735477,22.7961134750852));
#6110=CARTESIAN_POINT('Ctrl Pts',(-2.21857147695705,-1.04126205432324,22.7980221961712));
#6111=CARTESIAN_POINT('Ctrl Pts',(-2.20280124228042,-1.07422051047084,22.7999309172571));
#6112=CARTESIAN_POINT('Ctrl Pts',(-2.18631246248549,-1.10679178998611,22.8018396383431));
#6113=CARTESIAN_POINT('Ctrl Pts',(-2.14976489501527,-1.1789864005322,22.8060703402833));
#6114=CARTESIAN_POINT('Ctrl Pts',(-2.10956882614387,-1.24950456864088,22.8103010422236));
#6115=CARTESIAN_POINT('Ctrl Pts',(-2.06590160807848,-1.31795326007365,22.8145317441639));
#6116=CARTESIAN_POINT('Ctrl Pts',(-2.0222971277901,-1.38630360957098,22.8187563677495));
#6117=CARTESIAN_POINT('Ctrl Pts',(-1.97523165093686,-1.45258999872332,22.8229809913352));
#6118=CARTESIAN_POINT('Ctrl Pts',(-1.92492900182785,-1.51644274139251,22.8272056149209));
#6119=CARTESIAN_POINT('Ctrl Pts',(-1.87442837144414,-1.58054679582383,22.8314468657892));
#6120=CARTESIAN_POINT('Ctrl Pts',(-1.82066524674817,-1.64219758258895,22.8356881166575));
#6121=CARTESIAN_POINT('Ctrl Pts',(-1.76391083588765,-1.70104932704438,22.8399293675258));
#6122=CARTESIAN_POINT('Ctrl Pts',(-1.70748094820521,-1.7595645557144,22.8441463668127));
#6123=CARTESIAN_POINT('Ctrl Pts',(-1.6480942161064,-1.81531232708116,22.8483633660997));
#6124=CARTESIAN_POINT('Ctrl Pts',(-1.58605719311587,-1.86798630352725,22.8525803653866));
#6125=CARTESIAN_POINT('Ctrl Pts',(-1.52404073675561,-1.92064281739784,22.8567959666461));
#6126=CARTESIAN_POINT('Ctrl Pts',(-1.45937608854149,-1.97022725920252,22.8610115679055));
#6127=CARTESIAN_POINT('Ctrl Pts',(-1.39240456823055,-2.01647210949487,22.8652271691649));
#6128=CARTESIAN_POINT('Ctrl Pts',(-1.32543471903204,-2.06271580585875,22.8694426652342));
#6129=CARTESIAN_POINT('Ctrl Pts',(-1.25615849549141,-2.10561981303346,22.8736581613035));
#6130=CARTESIAN_POINT('Ctrl Pts',(-1.18494682731743,-2.14495950228212,22.8778736573728));
#6131=CARTESIAN_POINT('Ctrl Pts',(-1.11298057665873,-2.18471604794241,22.8821338222384));
#6132=CARTESIAN_POINT('Ctrl Pts',(-1.03903803618359,-2.22083204014725,22.886393987104));
#6133=CARTESIAN_POINT('Ctrl Pts',(-0.963526554605805,-2.25312379344089,
22.8906541519696));
#6134=CARTESIAN_POINT('Ctrl Pts',(-0.888698012437097,-2.2851234943148,22.8948757871385));
#6135=CARTESIAN_POINT('Ctrl Pts',(-0.812329257026773,-2.31336774702277,
22.8990974223075));
#6136=CARTESIAN_POINT('Ctrl Pts',(-0.734834006813902,-2.33772736486311,
22.9033190574765));
#6137=CARTESIAN_POINT('Ctrl Pts',(-0.656277840027232,-2.3624204679458,22.9075984871903));
#6138=CARTESIAN_POINT('Ctrl Pts',(-0.576564580054122,-2.38312164452855,
22.9118779169042));
#6139=CARTESIAN_POINT('Ctrl Pts',(-0.496136095112256,-2.39974982552906,
22.9161573466181));
#6140=CARTESIAN_POINT('Ctrl Pts',(-0.415707610170413,-2.41637800652957,
22.920436776332));
#6141=CARTESIAN_POINT('Ctrl Pts',(-0.334564395092533,-2.42893318165386,
22.9247162060459));
#6142=CARTESIAN_POINT('Ctrl Pts',(-0.253151943387779,-2.4373888371696,22.9289956357597));
#6143=CARTESIAN_POINT('Ctrl Pts',(-0.172666495462007,-2.44574821227058,
22.9332263377));
#6144=CARTESIAN_POINT('Ctrl Pts',(-0.0916151872469884,-2.45013243657524,
22.9374570396403));
#6145=CARTESIAN_POINT('Ctrl Pts',(-0.0104244858215312,-2.45047782689323,
22.9416877415805));
#6146=CARTESIAN_POINT('Ctrl Pts',(0.0706495669062312,-2.45082272098036,
22.9459123651662));
#6147=CARTESIAN_POINT('Ctrl Pts',(0.151862153987473,-2.44714030358704,22.9501369887519));
#6148=CARTESIAN_POINT('Ctrl Pts',(0.232781277887927,-2.43941860423029,22.9543616123376));
#6149=CARTESIAN_POINT('Ctrl Pts',(0.314018883450431,-2.43166651379259,22.9586028632059));
#6150=CARTESIAN_POINT('Ctrl Pts',(0.394960238836241,-2.41984322854105,22.9628441140742));
#6151=CARTESIAN_POINT('Ctrl Pts',(0.475167796108545,-2.40398956227795,22.9670853649425));
#6152=CARTESIAN_POINT('Ctrl Pts',(0.554916724509646,-2.38822654768547,22.9713023642294));
#6153=CARTESIAN_POINT('Ctrl Pts',(0.633939762958542,-2.36847920973697,22.9755193635164));
#6154=CARTESIAN_POINT('Ctrl Pts',(0.711813384088975,-2.34483943079943,22.9797363628034));
#6155=CARTESIAN_POINT('Ctrl Pts',(0.789661188410367,-2.32120748896578,22.9839519640628));
#6156=CARTESIAN_POINT('Ctrl Pts',(0.866359887472451,-2.29368580369894,22.9881675653222));
#6157=CARTESIAN_POINT('Ctrl Pts',(0.941499767728186,-2.26241650395496,22.9923831665817));
#6158=CARTESIAN_POINT('Ctrl Pts',(1.01663777304985,-2.23114798446076,22.996598662651));
#6159=CARTESIAN_POINT('Ctrl Pts',(1.09021660795235,-2.19613221609702,23.0008141587203));
#6160=CARTESIAN_POINT('Ctrl Pts',(1.16184658839672,-2.1575594441477,23.0050296547896));
#6161=CARTESIAN_POINT('Ctrl Pts',(1.23423558390143,-2.11857794229719,23.0092898196552));
#6162=CARTESIAN_POINT('Ctrl Pts',(1.30463374341914,-2.07596382114742,23.0135499845208));
#6163=CARTESIAN_POINT('Ctrl Pts',(1.37266608860179,-2.02996011271223,23.0178101493864));
#6164=CARTESIAN_POINT('Ctrl Pts',(1.44008313702903,-1.98437247008311,23.0220317845553));
#6165=CARTESIAN_POINT('Ctrl Pts',(1.50517665385351,-1.93545663745826,23.0262534197243));
#6166=CARTESIAN_POINT('Ctrl Pts',(1.56761403231989,-1.88349050851704,23.0304750548933));
#6167=CARTESIAN_POINT('Ctrl Pts',(1.63090618381365,-1.830812958846,23.0347544846072));
#6168=CARTESIAN_POINT('Ctrl Pts',(1.69146855702982,-1.77500129807639,23.039033914321));
#6169=CARTESIAN_POINT('Ctrl Pts',(1.74899375983996,-1.71638313847488,23.0433133440349));
#6170=CARTESIAN_POINT('Ctrl Pts',(1.8065189626501,-1.65776497887337,23.0475927737488));
#6171=CARTESIAN_POINT('Ctrl Pts',(1.86100671849117,-1.59634073090099,23.0518722034627));
#6172=CARTESIAN_POINT('Ctrl Pts',(1.91219354027986,-1.53247059172826,23.0561516331766));
#6173=CARTESIAN_POINT('Ctrl Pts',(1.96279752275772,-1.46932771059964,23.0603823351168));
#6174=CARTESIAN_POINT('Ctrl Pts',(2.01036573076248,-1.40355688444331,23.0646130370571));
#6175=CARTESIAN_POINT('Ctrl Pts',(2.05461372784418,-1.33548218983041,23.0688437389973));
#6176=CARTESIAN_POINT('Ctrl Pts',(2.09879815272924,-1.26750529982241,23.073068362583));
#6177=CARTESIAN_POINT('Ctrl Pts',(2.13967158932969,-1.19723150186965,23.0772929861687));
#6178=CARTESIAN_POINT('Ctrl Pts',(2.17699008478924,-1.12501752018773,23.0815176097543));
#6179=CARTESIAN_POINT('Ctrl Pts',(2.21445545846371,-1.05251931856092,23.0857588606226));
#6180=CARTESIAN_POINT('Ctrl Pts',(2.24833755111558,-0.978065998397429,23.0900001114909));
#6181=CARTESIAN_POINT('Ctrl Pts',(2.27843378361977,-0.902047528492861,23.0942413623592));
#6182=CARTESIAN_POINT('Ctrl Pts',(2.30835792509389,-0.82646373415073,23.0984583616461));
#6183=CARTESIAN_POINT('Ctrl Pts',(2.33453921131295,-0.749333077381762,23.1026753609331));
#6184=CARTESIAN_POINT('Ctrl Pts',(2.35682559033486,-0.671061388207306,23.10689236022));
#6185=CARTESIAN_POINT('Ctrl Pts',(2.37910458093457,-0.592815647810155,23.1111079614794));
#6186=CARTESIAN_POINT('Ctrl Pts',(2.39749110128002,-0.513430073130127,23.1153235627389));
#6187=CARTESIAN_POINT('Ctrl Pts',(2.41188282359221,-0.433326084214705,23.1195391639983));
#6188=CARTESIAN_POINT('Ctrl Pts',(2.42627418679377,-0.35322409410068,23.1237546600676));
#6189=CARTESIAN_POINT('Ctrl Pts',(2.43667086898207,-0.27240418331667,23.1279701561368));
#6190=CARTESIAN_POINT('Ctrl Pts',(2.44302184075576,-0.1912969827005,23.1321856522061));
#6191=CARTESIAN_POINT('Ctrl Pts',(2.44944010953551,-0.109330343251132,23.1364458170717));
#6192=CARTESIAN_POINT('Ctrl Pts',(2.45172636412338,-0.0270707710126519,
23.1407059819373));
#6193=CARTESIAN_POINT('Ctrl Pts',(2.44988191779356,0.0550348877364602,23.1449661468029));
#6194=CARTESIAN_POINT('Ctrl Pts',(2.4480541529678,0.136397968152651,23.1491877819719));
#6195=CARTESIAN_POINT('Ctrl Pts',(2.44217019982977,0.217609443384783,23.1534094171408));
#6196=CARTESIAN_POINT('Ctrl Pts',(2.43228362234344,0.298239216871039,23.1576310523097));
#6197=CARTESIAN_POINT('Ctrl Pts',(2.42226169676943,0.379972818822361,23.1619104820237));
#6198=CARTESIAN_POINT('Ctrl Pts',(2.40812680941357,0.461108184027478,23.1661899117376));
#6199=CARTESIAN_POINT('Ctrl Pts',(2.38998797701386,0.541209497079656,23.1704693414515));
#6200=CARTESIAN_POINT('Ctrl Pts',(2.37184914461414,0.621310810131857,23.1747487711654));
#6201=CARTESIAN_POINT('Ctrl Pts',(2.34970656253426,0.700377616280184,23.1790282008793));
#6202=CARTESIAN_POINT('Ctrl Pts',(2.32372041422682,0.777993371761954,23.1833076305932));
#6203=CARTESIAN_POINT('Ctrl Pts',(2.2980301574838,0.854725354587563,23.1875383325335));
#6204=CARTESIAN_POINT('Ctrl Pts',(2.26848683192573,0.930327787756541,23.1917690344737));
#6205=CARTESIAN_POINT('Ctrl Pts',(2.23520891010426,1.00438607028898,23.195999736414));
#6206=CARTESIAN_POINT('Ctrl Pts',(2.20197879949977,1.07833795144711,23.2002243599996));
#6207=CARTESIAN_POINT('Ctrl Pts',(2.16502493798028,1.1507496674678,23.2044489835853));
#6208=CARTESIAN_POINT('Ctrl Pts',(2.12451516514728,1.22122297843564,23.208673607171));
#6209=CARTESIAN_POINT('Ctrl Pts',(2.08384595386308,1.29197365841266,23.2129148580393));
#6210=CARTESIAN_POINT('Ctrl Pts',(2.03959293116593,1.36077019224979,23.2171561089076));
#6211=CARTESIAN_POINT('Ctrl Pts',(1.99197428751635,1.42723112629795,23.2213973597759));
#6212=CARTESIAN_POINT('Ctrl Pts',(1.94462792849352,1.49331203501919,23.2256143590628));
#6213=CARTESIAN_POINT('Ctrl Pts',(1.89395460707359,1.55708359966987,23.2298313583498));
#6214=CARTESIAN_POINT('Ctrl Pts',(1.84021320517734,1.61819826025458,23.2340483576367));
#6215=CARTESIAN_POINT('Ctrl Pts',(1.78648961973151,1.6792926599923,23.2382639588962));
#6216=CARTESIAN_POINT('Ctrl Pts',(1.72970028052972,1.73773155586434,23.2424795601556));
#6217=CARTESIAN_POINT('Ctrl Pts',(1.67014409817548,1.79320075321466,23.246695161415));
#6218=CARTESIAN_POINT('Ctrl Pts',(1.61058940190177,1.84866856646527,23.2509106574843));
#6219=CARTESIAN_POINT('Ctrl Pts',(1.54826834080045,1.90116651235743,23.2551261535536));
#6220=CARTESIAN_POINT('Ctrl Pts',(1.48351534306565,1.95041853890102,23.2593416496229));
#6221=CARTESIAN_POINT('Ctrl Pts',(1.41807620106281,2.00019245627414,23.2636018144885));
#6222=CARTESIAN_POINT('Ctrl Pts',(1.3501536521806,2.04665094891246,23.2678619793541));
#6223=CARTESIAN_POINT('Ctrl Pts',(1.28012409681148,2.08955319309239,23.2721221442197));
#6224=CARTESIAN_POINT('Ctrl Pts',(1.21072790132587,2.13206742166615,23.2763437793886));
#6225=CARTESIAN_POINT('Ctrl Pts',(1.13926310063557,2.17108929855892,23.2805654145576));
#6226=CARTESIAN_POINT('Ctrl Pts',(1.06612030182519,2.20643099870269,23.2847870497266));
#6227=CARTESIAN_POINT('Ctrl Pts',(0.991976171870974,2.24225652973078,23.2890664794405));
#6228=CARTESIAN_POINT('Ctrl Pts',(0.916108207728978,2.27430016473751,23.2933459091544));
#6229=CARTESIAN_POINT('Ctrl Pts',(0.838941847434474,2.30241760474142,23.2976253388683));
#6230=CARTESIAN_POINT('Ctrl Pts',(0.761775487139992,2.33053504474533,23.3019047685822));
#6231=CARTESIAN_POINT('Ctrl Pts',(0.683311218800494,2.35472620779236,23.3061841982961));
#6232=CARTESIAN_POINT('Ctrl Pts',(0.603985979936962,2.37490024759769,23.31046362801));
#6233=CARTESIAN_POINT('Ctrl Pts',(0.525563978780602,2.39484457547629,23.3146943299502));
#6234=CARTESIAN_POINT('Ctrl Pts',(0.446005557894012,2.41093785519662,23.3189250318905));
#6235=CARTESIAN_POINT('Ctrl Pts',(0.365723438613052,2.4230552235657,23.3231557338308));
#6236=CARTESIAN_POINT('Ctrl Pts',(0.285556662647317,2.43515518261062,23.3273803574164));
#6237=CARTESIAN_POINT('Ctrl Pts',(0.204668709248952,2.44329050640896,23.3316049810021));
#6238=CARTESIAN_POINT('Ctrl Pts',(0.123485271971385,2.44738669556042,23.3358296045878));
#6239=CARTESIAN_POINT('Ctrl Pts',(0.0419823127465615,2.45149900650197,23.3400708554561));
#6240=CARTESIAN_POINT('Ctrl Pts',(-0.0398180013644822,2.45154020316717,
23.3443121063244));
#6241=CARTESIAN_POINT('Ctrl Pts',(-0.121476829436484,2.44748720730264,23.3485533571927));
#6242=CARTESIAN_POINT('Ctrl Pts',(-0.202668730233576,2.44345738657249,23.3527703564796));
#6243=CARTESIAN_POINT('Ctrl Pts',(-0.283720289484594,2.43538009094083,23.3569873557666));
#6244=CARTESIAN_POINT('Ctrl Pts',(-0.364199131769934,2.42328480423124,23.3612043550536));
#6245=CARTESIAN_POINT('Ctrl Pts',(-0.444651293558449,2.4111935273738,23.365419956313));
#6246=CARTESIAN_POINT('Ctrl Pts',(-0.524530655896258,2.39508697373109,23.3696355575725));
#6247=CARTESIAN_POINT('Ctrl Pts',(-0.603411223520832,2.37504634593287,23.3738511588319));
#6248=CARTESIAN_POINT('Ctrl Pts',(-0.682289822871506,2.35500621820008,23.3780666549012));
#6249=CARTESIAN_POINT('Ctrl Pts',(-0.760169226587464,2.33103232705677,23.3822821509705));
#6250=CARTESIAN_POINT('Ctrl Pts',(-0.836636278495167,2.30325638770541,23.3864976470398));
#6251=CARTESIAN_POINT('Ctrl Pts',(-0.913913600678824,2.27518612527656,23.3907578119054));
#6252=CARTESIAN_POINT('Ctrl Pts',(-0.989748000478733,2.24323290960372,23.395017976771));
#6253=CARTESIAN_POINT('Ctrl Pts',(-1.0637332159061,2.20758281733168,23.3992781416365));
#6254=CARTESIAN_POINT('Ctrl Pts',(-1.13704929574981,2.17225515090055,23.4034997768055));
#6255=CARTESIAN_POINT('Ctrl Pts',(-1.20854912200814,2.13329748850934,23.4077214119745));
#6256=CARTESIAN_POINT('Ctrl Pts',(-1.27786330003922,2.09093654528608,23.4119430471435));
#6257=CARTESIAN_POINT('Ctrl Pts',(-1.34812639506922,2.04799567714332,23.4162224768573));
#6258=CARTESIAN_POINT('Ctrl Pts',(-1.41614313681858,2.00155791913076,23.4205019065712));
#6259=CARTESIAN_POINT('Ctrl Pts',(-1.48156186764085,1.95190283629912,23.4247813362851));
#6260=CARTESIAN_POINT('Ctrl Pts',(-1.54698059846309,1.90224775346751,23.429060765999));
#6261=CARTESIAN_POINT('Ctrl Pts',(-1.60980098518759,1.84937571182598,23.4333401957129));
#6262=CARTESIAN_POINT('Ctrl Pts',(-1.66971008496689,1.79360488462756,23.4376196254267));
#6263=CARTESIAN_POINT('Ctrl Pts',(-1.73069629536512,1.7368313491524,23.4419759953585));
#6264=CARTESIAN_POINT('Ctrl Pts',(-1.78892059448107,1.67681583651013,23.4463323652902));
#6265=CARTESIAN_POINT('Ctrl Pts',(-1.84401397873797,1.61386576152385,23.4506887352219));
#6266=CARTESIAN_POINT('Ctrl Pts',(-1.89663132731377,1.55374482172135,23.4548493188984));
#6267=CARTESIAN_POINT('Ctrl Pts',(-1.94639272356835,1.49094779758332,23.4590099025749));
#6268=CARTESIAN_POINT('Ctrl Pts',(-1.99301105788344,1.42578300352975,23.4631704862514));
#6269=CARTESIAN_POINT('Ctrl Pts',(-2.03958588784644,1.36067902143325,23.4673271872603));
#6270=CARTESIAN_POINT('Ctrl Pts',(-2.08302319534376,1.29321203995815,23.4714838882691));
#6271=CARTESIAN_POINT('Ctrl Pts',(-2.12307550508346,1.22372409051821,23.475640589278));
#6272=CARTESIAN_POINT('Ctrl Pts',(-2.16310357207426,1.15427820054801,23.4797947743307));
#6273=CARTESIAN_POINT('Ctrl Pts',(-2.19975046767757,1.08281418484751,23.4839489593833));
#6274=CARTESIAN_POINT('Ctrl Pts',(-2.2328124301214,1.00970238283139,23.4881031444359));
#6275=CARTESIAN_POINT('Ctrl Pts',(-2.26586521913785,0.936610866538073,23.4922561768614));
#6276=CARTESIAN_POINT('Ctrl Pts',(-2.2953348535945,0.86187290949826,23.4964092092869));
#6277=CARTESIAN_POINT('Ctrl Pts',(-2.32106460665762,0.785881251666771,23.5005622417124));
#6278=CARTESIAN_POINT('Ctrl Pts',(-2.3468068264979,0.709852773774781,23.504717286397));
#6279=CARTESIAN_POINT('Ctrl Pts',(-2.36880538969028,0.632569836508464,23.5088723310816));
#6280=CARTESIAN_POINT('Ctrl Pts',(-2.38695297832087,0.554441817763704,23.5130273757662));
#6281=CARTESIAN_POINT('Ctrl Pts',(-2.40510579337014,0.476291298523437,23.5171836170838));
#6282=CARTESIAN_POINT('Ctrl Pts',(-2.41940533677258,0.397295685264915,23.5213398584014));
#6283=CARTESIAN_POINT('Ctrl Pts',(-2.42979556890754,0.317873785199872,23.525496099719));
#6284=CARTESIAN_POINT('Ctrl Pts',(-2.44019766461207,0.238361201190058,23.529657086634));
#6285=CARTESIAN_POINT('Ctrl Pts',(-2.44668150234323,0.158421837288855,23.5338180735489));
#6286=CARTESIAN_POINT('Ctrl Pts',(-2.44924304161786,0.0784778509293303,
23.5379790604638));
#6287=CARTESIAN_POINT('Ctrl Pts',(-2.45010354819081,0.0516219965564258,
23.5393768749052));
#6288=CARTESIAN_POINT('Ctrl Pts',(-2.45052185378629,0.0247656044405823,
23.5407746893466));
#6289=CARTESIAN_POINT('Ctrl Pts',(-2.45049912112546,-0.00207541883967445,
23.542172503788));
#6290=CARTESIAN_POINT('',(-2.45049951066269,0.00154862580971605,24.342172503788));
#6291=CARTESIAN_POINT('Ctrl Pts',(-2.45186154582452,-0.00207657272782114,
23.542172503788));
#6292=CARTESIAN_POINT('Ctrl Pts',(-2.45316845875649,-0.146834277057642,
23.5497068768065));
#6293=CARTESIAN_POINT('Ctrl Pts',(-2.37555079931057,-1.10454055339028,23.5996265822973));
#6294=CARTESIAN_POINT('Ctrl Pts',(-1.11386918866955,-2.67479380645871,23.69193162026));
#6295=CARTESIAN_POINT('Ctrl Pts',(1.64579104116926,-2.38465895367458,23.819087617677));
#6296=CARTESIAN_POINT('Ctrl Pts',(2.89597072162243,0.0926285919153641,23.9462436150936));
#6297=CARTESIAN_POINT('Ctrl Pts',(1.49003467016963,2.484959387641,24.0733996125105));
#6298=CARTESIAN_POINT('Ctrl Pts',(-1.28252587751089,2.59814430893544,24.2005556099271));
#6299=CARTESIAN_POINT('Ctrl Pts',(-2.40720983591924,0.998919587715902,24.2901465736863));
#6300=CARTESIAN_POINT('Ctrl Pts',(-2.45396553830505,0.0940230514378206,
24.3373522049733));
#6301=CARTESIAN_POINT('Ctrl Pts',(-2.45328314078313,0.00155038496185235,
24.342172503788));
#6302=CARTESIAN_POINT('',(-2.45039359417306,0.00121703786866738,25.1421724505541));
#6303=CARTESIAN_POINT('Ctrl Pts',(-2.45049951066269,0.00154862580971605,
24.342172503788));
#6304=CARTESIAN_POINT('Ctrl Pts',(-2.45055002102087,-0.0783774655753502,
24.3463435443076));
#6305=CARTESIAN_POINT('Ctrl Pts',(-2.44668598205677,-0.158458895276197,
24.3505145848272));
#6306=CARTESIAN_POINT('Ctrl Pts',(-2.43888821404374,-0.238274063629557,
24.3546856253467));
#6307=CARTESIAN_POINT('Ctrl Pts',(-2.43108444750466,-0.318150630753082,
24.358859874489));
#6308=CARTESIAN_POINT('Ctrl Pts',(-2.41934085684055,-0.397760046305185,
24.3630341236312));
#6309=CARTESIAN_POINT('Ctrl Pts',(-2.40369055215446,-0.476678066920835,
24.3672083727735));
#6310=CARTESIAN_POINT('Ctrl Pts',(-2.38808610712647,-0.555364836227617,
24.3713703902281));
#6311=CARTESIAN_POINT('Ctrl Pts',(-2.36859787333247,-0.633363780969989,
24.3755324076827));
#6312=CARTESIAN_POINT('Ctrl Pts',(-2.34531045813516,-0.710259885508011,
24.3796944251373));
#6313=CARTESIAN_POINT('Ctrl Pts',(-2.32203341019326,-0.787121756896964,
24.3838545897156));
#6314=CARTESIAN_POINT('Ctrl Pts',(-2.29496067507136,-0.862881304691709,
24.388014754294));
#6315=CARTESIAN_POINT('Ctrl Pts',(-2.26422727925646,-0.937136637780686,
24.3921749188724));
#6316=CARTESIAN_POINT('Ctrl Pts',(-2.23349754837497,-1.01138311597927,24.3963345873544));
#6317=CARTESIAN_POINT('Ctrl Pts',(-2.19910820756057,-1.08412529377258,24.4004942558364));
#6318=CARTESIAN_POINT('Ctrl Pts',(-2.16124259240263,-1.15498082528878,24.4046539243184));
#6319=CARTESIAN_POINT('Ctrl Pts',(-2.12315117743541,-1.22625888171145,24.4088383976886));
#6320=CARTESIAN_POINT('Ctrl Pts',(-2.08154210565957,-1.29562727592315,24.4130228710588));
#6321=CARTESIAN_POINT('Ctrl Pts',(-2.0366481729518,-1.36272318157874,24.417207344429));
#6322=CARTESIAN_POINT('Ctrl Pts',(-1.99196174743553,-1.42950895884718,24.4213724764703));
#6323=CARTESIAN_POINT('Ctrl Pts',(-1.94402109266038,-1.49404285456841,24.4255376085116));
#6324=CARTESIAN_POINT('Ctrl Pts',(-1.89309724305004,-1.5559990611682,24.4297027405529));
#6325=CARTESIAN_POINT('Ctrl Pts',(-1.84181868622524,-1.61838682024548,24.4338968845875));
#6326=CARTESIAN_POINT('Ctrl Pts',(-1.78751554941226,-1.67816048007871,24.4380910286221));
#6327=CARTESIAN_POINT('Ctrl Pts',(-1.73050189298297,-1.73502548926013,24.4422851726568));
#6328=CARTESIAN_POINT('Ctrl Pts',(-1.67348823655367,-1.79189049844156,24.4464793166914));
#6329=CARTESIAN_POINT('Ctrl Pts',(-1.61376446905642,-1.84584658183965,24.450673460726));
#6330=CARTESIAN_POINT('Ctrl Pts',(-1.55167630420413,-1.89664200548533,24.4548676047607));
#6331=CARTESIAN_POINT('Ctrl Pts',(-1.48904695305653,-1.94788018319222,24.4590983067009));
#6332=CARTESIAN_POINT('Ctrl Pts',(-1.4237591760496,-1.99610924247822,24.4633290086412));
#6333=CARTESIAN_POINT('Ctrl Pts',(-1.35613416485727,-2.04104149318599,24.4675597105814));
#6334=CARTESIAN_POINT('Ctrl Pts',(-1.28860631219858,-2.08590918861287,24.4717843341671));
#6335=CARTESIAN_POINT('Ctrl Pts',(-1.21874827851865,-2.12748922743726,24.4760089577528));
#6336=CARTESIAN_POINT('Ctrl Pts',(-1.14691430973509,-2.16553407179958,24.4802335813385));
#6337=CARTESIAN_POINT('Ctrl Pts',(-1.07479761666243,-2.20372865314232,24.4844748322068));
#6338=CARTESIAN_POINT('Ctrl Pts',(-1.00068976864271,-2.23835985219343,24.488716083075));
#6339=CARTESIAN_POINT('Ctrl Pts',(-0.924978671719143,-2.26922116746356,
24.4929573339433));
#6340=CARTESIAN_POINT('Ctrl Pts',(-0.849700492791117,-2.29990601694084,
24.4971743332303));
#6341=CARTESIAN_POINT('Ctrl Pts',(-0.772837785029174,-2.32686380092333,
24.5013913325172));
#6342=CARTESIAN_POINT('Ctrl Pts',(-0.694794824440356,-2.34993838258174,
24.5056083318042));
#6343=CARTESIAN_POINT('Ctrl Pts',(-0.616777736800381,-2.37300531451151,
24.5098239330636));
#6344=CARTESIAN_POINT('Ctrl Pts',(-0.537581618970728,-2.39219146885364,
24.5140395343231));
#6345=CARTESIAN_POINT('Ctrl Pts',(-0.457626837638351,-2.40739027319484,
24.5182551355825));
#6346=CARTESIAN_POINT('Ctrl Pts',(-0.37767405138428,-2.42258869828662,24.5224706316518));
#6347=CARTESIAN_POINT('Ctrl Pts',(-0.29696309634789,-2.43379988541412,24.5266861277211));
#6348=CARTESIAN_POINT('Ctrl Pts',(-0.215924066859916,-2.44096846504634,
24.5309016237904));
#6349=CARTESIAN_POINT('Ctrl Pts',(-0.134026320903077,-2.44821300532897,
24.535161788656));
#6350=CARTESIAN_POINT('Ctrl Pts',(-0.0517939874886304,-2.45132869563445,
24.5394219535216));
#6351=CARTESIAN_POINT('Ctrl Pts',(0.0303260965835189,-2.45031234291998,
24.5436821183871));
#6352=CARTESIAN_POINT('Ctrl Pts',(0.111703471857997,-2.44930518228211,24.5479037535561));
#6353=CARTESIAN_POINT('Ctrl Pts',(0.192970154550918,-2.44424051071892,24.5521253887251));
#6354=CARTESIAN_POINT('Ctrl Pts',(0.273695529801835,-2.43516755213404,24.556347023894));
#6355=CARTESIAN_POINT('Ctrl Pts',(0.355526042313421,-2.4259703839736,24.5606264536079));
#6356=CARTESIAN_POINT('Ctrl Pts',(0.436799825928479,-2.41265443022044,24.5649058833218));
#6357=CARTESIAN_POINT('Ctrl Pts',(0.51707998801538,-2.39532430706032,24.5691853130357));
#6358=CARTESIAN_POINT('Ctrl Pts',(0.59736015010228,-2.37799418390021,24.5734647427496));
#6359=CARTESIAN_POINT('Ctrl Pts',(0.676646233963054,-2.35665008210095,24.5777441724635));
#6360=CARTESIAN_POINT('Ctrl Pts',(0.754520101636108,-2.33144797630722,24.5820236021773));
#6361=CARTESIAN_POINT('Ctrl Pts',(0.8315072576559,-2.30653283456911,24.5862543041176));
#6362=CARTESIAN_POINT('Ctrl Pts',(0.907403777978842,-2.27775342892994,24.5904850060578));
#6363=CARTESIAN_POINT('Ctrl Pts',(0.981793887963596,-2.2452240448466,24.5947157079981));
#6364=CARTESIAN_POINT('Ctrl Pts',(1.05607711982936,-2.21274139653745,24.5989403315838));
#6365=CARTESIAN_POINT('Ctrl Pts',(1.12885781728276,-2.17651965477304,24.6031649551694));
#6366=CARTESIAN_POINT('Ctrl Pts',(1.19973606806975,-2.13672263454397,24.6073895787551));
#6367=CARTESIAN_POINT('Ctrl Pts',(1.27089328162899,-2.0967689811169,24.6116308296234));
#6368=CARTESIAN_POINT('Ctrl Pts',(1.34013258959559,-2.05321199180245,24.6158720804917));
#6369=CARTESIAN_POINT('Ctrl Pts',(1.40707035736177,-2.00626599917205,24.62011333136));
#6370=CARTESIAN_POINT('Ctrl Pts',(1.47362537325352,-1.95958844493264,24.6243303306469));
#6371=CARTESIAN_POINT('Ctrl Pts',(1.53790471347347,-1.90956080874431,24.6285473299339));
#6372=CARTESIAN_POINT('Ctrl Pts',(1.59955822498833,-1.85643845437229,24.6327643292208));
#6373=CARTESIAN_POINT('Ctrl Pts',(1.66119129701531,-1.80333371122292,24.6369799304802));
#6374=CARTESIAN_POINT('Ctrl Pts',(1.72019991700233,-1.74713659061232,24.6411955317397));
#6375=CARTESIAN_POINT('Ctrl Pts',(1.77626689188701,-1.68814281942792,24.6454111329991));
#6376=CARTESIAN_POINT('Ctrl Pts',(1.8323324677559,-1.62915052029044,24.6496266290684));
#6377=CARTESIAN_POINT('Ctrl Pts',(1.88545622487061,-1.56736204717701,24.6538421251377));
#6378=CARTESIAN_POINT('Ctrl Pts',(1.93535875271566,-1.50310902741181,24.658057621207));
#6379=CARTESIAN_POINT('Ctrl Pts',(1.98579006431816,-1.43817516131103,24.6623177860726));
#6380=CARTESIAN_POINT('Ctrl Pts',(2.03293116385415,-1.37072457999829,24.6665779509381));
#6381=CARTESIAN_POINT('Ctrl Pts',(2.07653744401198,-1.30113123612347,24.6708381158037));
#6382=CARTESIAN_POINT('Ctrl Pts',(2.11974934113558,-1.23216730695727,24.6750597509727));
#6383=CARTESIAN_POINT('Ctrl Pts',(2.15948992514904,-1.16109965892969,24.6792813861416));
#6384=CARTESIAN_POINT('Ctrl Pts',(2.19556744143292,-1.08831698512873,24.6835030213106));
#6385=CARTESIAN_POINT('Ctrl Pts',(2.23213886198692,-1.01453791032563,24.6877824510245));
#6386=CARTESIAN_POINT('Ctrl Pts',(2.26494596294823,-0.938996950217633,24.6920618807384));
#6387=CARTESIAN_POINT('Ctrl Pts',(2.29384016231569,-0.862118066013883,24.6963413104523));
#6388=CARTESIAN_POINT('Ctrl Pts',(2.32273436168315,-0.785239181810154,24.7006207401662));
#6389=CARTESIAN_POINT('Ctrl Pts',(2.34771557258452,-0.707022860766869,24.7049001698801));
#6390=CARTESIAN_POINT('Ctrl Pts',(2.36868854702988,-0.627905102041274,24.709179599594));
#6391=CARTESIAN_POINT('Ctrl Pts',(2.38942271247033,-0.549688218548305,24.7134103015343));
#6392=CARTESIAN_POINT('Ctrl Pts',(2.40631748587856,-0.47029613696848,24.7176410034746));
#6393=CARTESIAN_POINT('Ctrl Pts',(2.41924384829596,-0.390140298459629,24.7218717054148));
#6394=CARTESIAN_POINT('Ctrl Pts',(2.43215163908734,-0.310099621835258,24.7260963290005));
#6395=CARTESIAN_POINT('Ctrl Pts',(2.44110226899636,-0.229297822830013,24.7303209525862));
#6396=CARTESIAN_POINT('Ctrl Pts',(2.44601694947688,-0.148159822056558,24.7345455761718));
#6397=CARTESIAN_POINT('Ctrl Pts',(2.45095097316743,-0.066702478164706,24.7387868270401));
#6398=CARTESIAN_POINT('Ctrl Pts',(2.45181708829447,0.0150932609078766,24.7430280779084));
#6399=CARTESIAN_POINT('Ctrl Pts',(2.44858779225845,0.0967888092853415,24.7472693287767));
#6400=CARTESIAN_POINT('Ctrl Pts',(2.44537696142007,0.178017220420015,24.7514863280637));
#6401=CARTESIAN_POINT('Ctrl Pts',(2.43811744621298,0.259146114167406,24.7557033273506));
#6402=CARTESIAN_POINT('Ctrl Pts',(2.42683436864361,0.339742839762895,24.7599203266376));
#6403=CARTESIAN_POINT('Ctrl Pts',(2.41555503166129,0.420312845780755,24.764135927897));
#6404=CARTESIAN_POINT('Ctrl Pts',(2.4002548456395,0.500350573793417,24.7683515291565));
#6405=CARTESIAN_POINT('Ctrl Pts',(2.38101071310204,0.579429231307268,24.7725671304159));
#6406=CARTESIAN_POINT('Ctrl Pts',(2.36176706075539,0.658505915604342,24.7767826264852));
#6407=CARTESIAN_POINT('Ctrl Pts',(2.33857976857915,0.736623125367781,24.7809981225545));
#6408=CARTESIAN_POINT('Ctrl Pts',(2.31157637857783,0.813366397142773,24.7852136186238));
#6409=CARTESIAN_POINT('Ctrl Pts',(2.2842868516884,0.890922866111448,24.7894737834894));
#6410=CARTESIAN_POINT('Ctrl Pts',(2.25310001776106,0.967075643962771,24.793733948355));
#6411=CARTESIAN_POINT('Ctrl Pts',(2.21819784700319,1.04141661286461,24.7979941132206));
#6412=CARTESIAN_POINT('Ctrl Pts',(2.18361133774984,1.1150852286841,24.8022157483895));
#6413=CARTESIAN_POINT('Ctrl Pts',(2.14537670099685,1.1869742902046,24.8064373835585));
#6414=CARTESIAN_POINT('Ctrl Pts',(2.10371691515956,1.2567121352448,24.8106590187274));
#6415=CARTESIAN_POINT('Ctrl Pts',(2.06148680330678,1.32740469732185,24.8149384484413));
#6416=CARTESIAN_POINT('Ctrl Pts',(2.01573732590791,1.39588628495846,24.8192178781553));
#6417=CARTESIAN_POINT('Ctrl Pts',(1.96674448748338,1.46180243909829,24.8234973078692));
#6418=CARTESIAN_POINT('Ctrl Pts',(1.91775164905886,1.52771859323813,24.8277767375831));
#6419=CARTESIAN_POINT('Ctrl Pts',(1.86551581223935,1.59106897703644,24.8320561672969));
#6420=CARTESIAN_POINT('Ctrl Pts',(1.81035197820623,1.65153745492035,24.8363355970108));
#6421=CARTESIAN_POINT('Ctrl Pts',(1.75581626777779,1.71131740781386,24.8405662989511));
#6422=CARTESIAN_POINT('Ctrl Pts',(1.69821380838736,1.7685056291386,24.8447970008914));
#6423=CARTESIAN_POINT('Ctrl Pts',(1.63782066989105,1.82277088611752,24.8490277028316));
#6424=CARTESIAN_POINT('Ctrl Pts',(1.57751429971716,1.87695817885362,24.8532523264173));
#6425=CARTESIAN_POINT('Ctrl Pts',(1.51442555639558,1.92823053948165,24.857476950003));
#6426=CARTESIAN_POINT('Ctrl Pts',(1.44886903807584,1.97629166888523,24.8617015735887));
#6427=CARTESIAN_POINT('Ctrl Pts',(1.38305450227006,2.02454195738547,24.8659428244569));
#6428=CARTESIAN_POINT('Ctrl Pts',(1.31475304428376,2.06955533231758,24.8701840753252));
#6429=CARTESIAN_POINT('Ctrl Pts',(1.24431851825835,2.11107121507526,24.8744253261935));
#6430=CARTESIAN_POINT('Ctrl Pts',(1.17428673866064,2.15234970894971,24.8786423254805));
#6431=CARTESIAN_POINT('Ctrl Pts',(1.10214662337518,2.1901703610904,24.8828593247674));
#6432=CARTESIAN_POINT('Ctrl Pts',(1.02827552813907,2.2243200507639,24.8870763240544));
#6433=CARTESIAN_POINT('Ctrl Pts',(0.954428922787074,2.25845841906819,24.8912919253138));
#6434=CARTESIAN_POINT('Ctrl Pts',(0.878852898869528,2.28892804667599,24.8955075265733));
#6435=CARTESIAN_POINT('Ctrl Pts',(0.801947921323598,2.31556251945068,24.8997231278327));
#6436=CARTESIAN_POINT('Ctrl Pts',(0.725044862755625,2.34219632762643,24.903938623902));
#6437=CARTESIAN_POINT('Ctrl Pts',(0.64681335629807,2.36499502006848,24.9081541199713));
#6438=CARTESIAN_POINT('Ctrl Pts',(0.567670917970752,2.38384143325227,24.9123696160406));
#6439=CARTESIAN_POINT('Ctrl Pts',(0.487689860084349,2.4028875492889,24.9166297809062));
#6440=CARTESIAN_POINT('Ctrl Pts',(0.406778917865274,2.41789700011419,24.9208899457718));
#6441=CARTESIAN_POINT('Ctrl Pts',(0.325379740277146,2.42880181871992,24.9251501106373));
#6442=CARTESIAN_POINT('Ctrl Pts',(0.244716751478899,2.43960801218653,24.9293717458063));
#6443=CARTESIAN_POINT('Ctrl Pts',(0.163574796899474,2.44638354323401,24.9335933809753));
#6444=CARTESIAN_POINT('Ctrl Pts',(0.0823870774693992,2.44911466033464,24.9378150161442));
#6445=CARTESIAN_POINT('Ctrl Pts',(8.78912474756577E-5,2.45188316666092,
24.9420944458581));
#6446=CARTESIAN_POINT('Ctrl Pts',(-0.0822578277790784,2.45049569217383,
24.946373875572));
#6447=CARTESIAN_POINT('Ctrl Pts',(-0.164202633375031,2.44499238141813,24.9506533052859));
#6448=CARTESIAN_POINT('Ctrl Pts',(-0.246147438970984,2.43948907066243,24.9549327349998));
#6449=CARTESIAN_POINT('Ctrl Pts',(-0.327690851599038,2.42987004615084,24.9592121647136));
#6450=CARTESIAN_POINT('Ctrl Pts',(-0.40839653252675,2.41622898795212,24.9634915944275));
#6451=CARTESIAN_POINT('Ctrl Pts',(-0.488183257328567,2.40274325381301,24.9677222963678));
#6452=CARTESIAN_POINT('Ctrl Pts',(-0.567451338534409,2.38527593323873,24.971952998308));
#6453=CARTESIAN_POINT('Ctrl Pts',(-0.645772822204555,2.36387980068826,24.9761837002483));
#6454=CARTESIAN_POINT('Ctrl Pts',(-0.723981779453544,2.34251440849292,24.980408323834));
#6455=CARTESIAN_POINT('Ctrl Pts',(-0.801246395387,2.31723153636686,24.9846329474197));
#6456=CARTESIAN_POINT('Ctrl Pts',(-0.877147227128712,2.28813526521935,24.9888575710053));
#6457=CARTESIAN_POINT('Ctrl Pts',(-0.953346789527392,2.25892447690521,24.9930988218736));
#6458=CARTESIAN_POINT('Ctrl Pts',(-1.02817134162205,2.22587028670691,24.9973400727419));
#6459=CARTESIAN_POINT('Ctrl Pts',(-1.101210219165,2.18912911981148,25.0015813236102));
#6460=CARTESIAN_POINT('Ctrl Pts',(-1.17383145853132,2.15259803985147,25.0057983228972));
#6461=CARTESIAN_POINT('Ctrl Pts',(-1.2446869693642,2.11242224432312,25.0100153221841));
#6462=CARTESIAN_POINT('Ctrl Pts',(-1.31339326393733,2.06880361181144,25.0142323214711));
#6463=CARTESIAN_POINT('Ctrl Pts',(-1.38207678087071,2.02519943983068,25.0184479227305));
#6464=CARTESIAN_POINT('Ctrl Pts',(-1.44861210416238,1.97815494650584,25.0226635239899));
#6465=CARTESIAN_POINT('Ctrl Pts',(-1.51264250341395,1.92791672716058,25.0268791252494));
#6466=CARTESIAN_POINT('Ctrl Pts',(-1.57667130494176,1.87767976138859,25.0310946213187));
#6467=CARTESIAN_POINT('Ctrl Pts',(-1.6381949414896,1.82424951596874,25.035310117388));
#6468=CARTESIAN_POINT('Ctrl Pts',(-1.69688885882357,1.7679135869155,25.0395256134573));
#6469=CARTESIAN_POINT('Ctrl Pts',(-1.75620471639741,1.71098070364929,25.0437857783229));
#6470=CARTESIAN_POINT('Ctrl Pts',(-1.81263016772042,1.65108051476925,25.0480459431884));
#6471=CARTESIAN_POINT('Ctrl Pts',(-1.86586895503825,1.58854754182066,25.052306108054));
#6472=CARTESIAN_POINT('Ctrl Pts',(-1.91862624119627,1.52658012831694,25.056527743223));
#6473=CARTESIAN_POINT('Ctrl Pts',(-1.96825403535061,1.46202777234665,25.060749378392));
#6474=CARTESIAN_POINT('Ctrl Pts',(-2.01450623568522,1.3952472456111,25.0649710135609));
#6475=CARTESIAN_POINT('Ctrl Pts',(-2.0613916325807,1.3275524877783,25.0692504432748));
#6476=CARTESIAN_POINT('Ctrl Pts',(-2.10480805075346,1.25756850989394,25.0735298729887));
#6477=CARTESIAN_POINT('Ctrl Pts',(-2.14454698933912,1.18569324047854,25.0778093027026));
#6478=CARTESIAN_POINT('Ctrl Pts',(-2.18428592792479,1.11381797106313,25.0820887324165));
#6479=CARTESIAN_POINT('Ctrl Pts',(-2.22034723029967,1.04005187962111,25.0863681621304));
#6480=CARTESIAN_POINT('Ctrl Pts',(-2.25257341972751,0.964812540723382,25.0906475918443));
#6481=CARTESIAN_POINT('Ctrl Pts',(-2.28784259062639,0.882468672304055,25.0953311098341));
#6482=CARTESIAN_POINT('Ctrl Pts',(-2.3186323432272,0.798096502576319,25.1000146278239));
#6483=CARTESIAN_POINT('Ctrl Pts',(-2.34472986509261,0.712174213056611,25.1046981458138));
#6484=CARTESIAN_POINT('Ctrl Pts',(-2.37074857500766,0.626511400404119,25.1093675200397));
#6485=CARTESIAN_POINT('Ctrl Pts',(-2.39210319657215,0.539308069372609,25.1140368942657));
#6486=CARTESIAN_POINT('Ctrl Pts',(-2.40862911253218,0.451061024987151,25.1187062684916));
#6487=CARTESIAN_POINT('Ctrl Pts',(-2.42506955792525,0.363270386463512,25.1233514931295));
#6488=CARTESIAN_POINT('Ctrl Pts',(-2.43673099334932,0.274447073716838,25.1279967177674));
#6489=CARTESIAN_POINT('Ctrl Pts',(-2.44349925207794,0.185099041311755,25.1326419424054));
#6490=CARTESIAN_POINT('Ctrl Pts',(-2.44812801520265,0.123994569062097,25.1358187778917));
#6491=CARTESIAN_POINT('Ctrl Pts',(-2.45046918747822,0.0626450716972059,
25.1389956133781));
#6492=CARTESIAN_POINT('Ctrl Pts',(-2.45049969773741,0.0012171231945159,
25.1421724488644));
#6493=CARTESIAN_POINT('',(-2.45049910673901,-0.00209233632933992,25.9421725277106));
#6494=CARTESIAN_POINT('Ctrl Pts',(-2.4470507577615,0.00121434964273421,
25.142172503788));
#6495=CARTESIAN_POINT('Ctrl Pts',(-2.4448728557432,-0.48557354190418,25.1673828656123));
#6496=CARTESIAN_POINT('Ctrl Pts',(-2.06824726699471,-1.79388675645704,25.2349785599091));
#6497=CARTESIAN_POINT('Ctrl Pts',(0.0634192777159373,-2.89675757904347,
25.3449595866777));
#6498=CARTESIAN_POINT('Ctrl Pts',(2.46980667520369,-1.51501863475477,25.4721155840945));
#6499=CARTESIAN_POINT('Ctrl Pts',(2.61094590709541,1.25625950613601,25.5992715815113));
#6500=CARTESIAN_POINT('Ctrl Pts',(0.357387413898736,2.8753261924378,25.7264275789279));
#6501=CARTESIAN_POINT('Ctrl Pts',(-1.96297985249653,1.96014493364779,25.8407278863536));
#6502=CARTESIAN_POINT('Ctrl Pts',(-2.44422981805528,0.567055840943636,25.9126428613069));
#6503=CARTESIAN_POINT('Ctrl Pts',(-2.44883297466156,-0.00209045264269275,
25.942172503788));
#6504=CARTESIAN_POINT('',(-2.45089310683891,-0.000179724726367168,26.742172503788));
#6505=CARTESIAN_POINT('Ctrl Pts',(-2.45049910673901,-0.00209233632933992,
25.9421725277106));
#6506=CARTESIAN_POINT('Ctrl Pts',(-2.45041577647178,-0.0996869450663497,
25.9472327318638));
#6507=CARTESIAN_POINT('Ctrl Pts',(-2.4444983547822,-0.197027745374281,25.952292936017));
#6508=CARTESIAN_POINT('Ctrl Pts',(-2.43286032705321,-0.293497664472038,
25.9573531401702));
#6509=CARTESIAN_POINT('Ctrl Pts',(-2.42106460921947,-0.391274708110316,
25.9624819078413));
#6510=CARTESIAN_POINT('Ctrl Pts',(-2.40339228844551,-0.488157094530591,
25.9676106755125));
#6511=CARTESIAN_POINT('Ctrl Pts',(-2.38001045809284,-0.583524180620417,
25.9727394431836));
#6512=CARTESIAN_POINT('Ctrl Pts',(-2.36785304147323,-0.633110435413318,
25.9754061533763));
#6513=CARTESIAN_POINT('Ctrl Pts',(-2.35415285291789,-0.682287388048195,
25.9780728635689));
#6514=CARTESIAN_POINT('Ctrl Pts',(-2.33893842772718,-0.730970096037509,
25.9807395737615));
#6515=CARTESIAN_POINT('Ctrl Pts',(-2.31480093488955,-0.808204595578558,
25.9849702757017));
#6516=CARTESIAN_POINT('Ctrl Pts',(-2.28678837606447,-0.884387484301311,
25.989200977642));
#6517=CARTESIAN_POINT('Ctrl Pts',(-2.25501083799109,-0.959101856187706,
25.9934316795822));
#6518=CARTESIAN_POINT('Ctrl Pts',(-2.22327895549613,-1.03370888407986,25.9976563031679));
#6519=CARTESIAN_POINT('Ctrl Pts',(-2.1877930172753,-1.10685116109401,26.0018809267536));
#6520=CARTESIAN_POINT('Ctrl Pts',(-2.14871279704817,-1.178127143309,26.0061055503393));
#6521=CARTESIAN_POINT('Ctrl Pts',(-2.10947876480593,-1.24968365368861,26.0103468012075));
#6522=CARTESIAN_POINT('Ctrl Pts',(-2.06662223866485,-1.31935869407582,26.0145880520758));
#6523=CARTESIAN_POINT('Ctrl Pts',(-2.0203536715094,-1.38676648792018,26.0188293029441));
#6524=CARTESIAN_POINT('Ctrl Pts',(-1.97434966920874,-1.45378884226887,26.0230463022311));
#6525=CARTESIAN_POINT('Ctrl Pts',(-1.92497280611408,-1.51856942078306,26.027263301518));
#6526=CARTESIAN_POINT('Ctrl Pts',(-1.8724749018644,-1.58075551300253,26.0314803008049));
#6527=CARTESIAN_POINT('Ctrl Pts',(-1.81999440181849,-1.64292098917196,26.0356959020644));
#6528=CARTESIAN_POINT('Ctrl Pts',(-1.76439521510405,-1.70249333203664,26.0399115033238));
#6529=CARTESIAN_POINT('Ctrl Pts',(-1.70596985481669,-1.75915238238668,26.0441271045832));
#6530=CARTESIAN_POINT('Ctrl Pts',(-1.64754595239291,-1.81581001894713,26.0483426006525));
#6531=CARTESIAN_POINT('Ctrl Pts',(-1.58629635121864,-1.86955418454366,26.0525580967218));
#6532=CARTESIAN_POINT('Ctrl Pts',(-1.5225498440212,-1.92010213855175,26.0567735927911));
#6533=CARTESIAN_POINT('Ctrl Pts',(-1.45812785766353,-1.9711857154673,26.0610337576567));
#6534=CARTESIAN_POINT('Ctrl Pts',(-1.39115610371382,-2.01900462760259,26.0652939225222));
#6535=CARTESIAN_POINT('Ctrl Pts',(-1.32200604904805,-2.0633105089347,26.0695540873878));
#6536=CARTESIAN_POINT('Ctrl Pts',(-1.25348139990362,-2.10721567991383,26.0737757225568));
#6537=CARTESIAN_POINT('Ctrl Pts',(-1.1828181321915,-2.14767092938976,26.0779973577257));
#6538=CARTESIAN_POINT('Ctrl Pts',(-1.11040298547257,-2.18448059269329,26.0822189928947));
#6539=CARTESIAN_POINT('Ctrl Pts',(-1.03699646922851,-2.22179418342198,26.0864984226086));
#6540=CARTESIAN_POINT('Ctrl Pts',(-0.961790195748017,-2.25536141382185,
26.0907778523225));
#6541=CARTESIAN_POINT('Ctrl Pts',(-0.885206606296767,-2.28502943398298,
26.0950572820364));
#6542=CARTESIAN_POINT('Ctrl Pts',(-0.808623016845516,-2.3146974541441,26.0993367117503));
#6543=CARTESIAN_POINT('Ctrl Pts',(-0.73066259777886,-2.3404661722849,26.1036161414642));
#6544=CARTESIAN_POINT('Ctrl Pts',(-0.651760365548761,-2.36223594839714,
26.1078955711781));
#6545=CARTESIAN_POINT('Ctrl Pts',(-0.573756554456445,-2.38375784271351,
26.1121262731184));
#6546=CARTESIAN_POINT('Ctrl Pts',(-0.494538886439508,-2.4014523915938,26.1163569750587));
#6547=CARTESIAN_POINT('Ctrl Pts',(-0.414517480633748,-2.41518643343512,
26.1205876769989));
#6548=CARTESIAN_POINT('Ctrl Pts',(-0.334611043569686,-2.42890074323732,
26.1248123005846));
#6549=CARTESIAN_POINT('Ctrl Pts',(-0.253903616583434,-2.43866576896868,
26.1290369241703));
#6550=CARTESIAN_POINT('Ctrl Pts',(-0.172819304132042,-2.44439844095011,
26.133261547756));
#6551=CARTESIAN_POINT('Ctrl Pts',(-0.0914158598690766,-2.45015367559426,
26.1375027986243));
#6552=CARTESIAN_POINT('Ctrl Pts',(-0.00963301454602711,-2.45184462109823,
26.1417440494925));
#6553=CARTESIAN_POINT('Ctrl Pts',(0.0720909456153298,-2.44943935331338,
26.1459853003608));
#6554=CARTESIAN_POINT('Ctrl Pts',(0.153347606074818,-2.44704783891147,26.1502022996478));
#6555=CARTESIAN_POINT('Ctrl Pts',(0.234545583426826,-2.44060684242898,26.1544192989348));
#6556=CARTESIAN_POINT('Ctrl Pts',(0.31525199556275,-2.43013712150029,26.1586362982217));
#6557=CARTESIAN_POINT('Ctrl Pts',(0.395931651757442,-2.41967087151313,26.1628518994812));
#6558=CARTESIAN_POINT('Ctrl Pts',(0.476119605525667,-2.40517860915679,26.1670675007406));
#6559=CARTESIAN_POINT('Ctrl Pts',(0.555388310547945,-2.38673292902803,26.1712831020001));
#6560=CARTESIAN_POINT('Ctrl Pts',(0.634655037611317,-2.36828770916661,26.1754985980694));
#6561=CARTESIAN_POINT('Ctrl Pts',(0.713002108821671,-2.34588937412875,26.1797140941387));
#6562=CARTESIAN_POINT('Ctrl Pts',(0.790013795594285,-2.31966127974985,26.183929590208));
#6563=CARTESIAN_POINT('Ctrl Pts',(0.867841523774748,-2.29315526377283,26.1881897550736));
#6564=CARTESIAN_POINT('Ctrl Pts',(0.944304934861096,-2.26273798332415,26.1924499199392));
#6565=CARTESIAN_POINT('Ctrl Pts',(1.01899409668388,-2.22858728366726,26.1967100848047));
#6566=CARTESIAN_POINT('Ctrl Pts',(1.0930077563053,-2.19474544907504,26.2009317199737));
#6567=CARTESIAN_POINT('Ctrl Pts',(1.16527874189663,-2.15723772646195,26.2051533551427));
#6568=CARTESIAN_POINT('Ctrl Pts',(1.23543316153551,-2.11628333485343,26.2093749903117));
#6569=CARTESIAN_POINT('Ctrl Pts',(1.30654800115254,-2.07476827413675,26.2136544200256));
#6570=CARTESIAN_POINT('Ctrl Pts',(1.37548747002772,-2.02971173012085,26.2179338497394));
#6571=CARTESIAN_POINT('Ctrl Pts',(1.44189434374375,-1.98138611872593,26.2222132794533));
#6572=CARTESIAN_POINT('Ctrl Pts',(1.50830121745975,-1.93306050733102,26.2264927091672));
#6573=CARTESIAN_POINT('Ctrl Pts',(1.572175155532,-1.88146618777238,26.2307721388811));
#6574=CARTESIAN_POINT('Ctrl Pts',(1.63319686181349,-1.82691495712378,26.235051568595));
#6575=CARTESIAN_POINT('Ctrl Pts',(1.69352374376341,-1.77298487466459,26.2392822705352));
#6576=CARTESIAN_POINT('Ctrl Pts',(1.75128995276365,-1.71596206270461,26.2435129724755));
#6577=CARTESIAN_POINT('Ctrl Pts',(1.80616148883622,-1.65611923672329,26.2477436744157));
#6578=CARTESIAN_POINT('Ctrl Pts',(1.86095418960974,-1.59636238841672,26.2519682980014));
#6579=CARTESIAN_POINT('Ctrl Pts',(1.91286016552293,-1.53379391262625,26.2561929215871));
#6580=CARTESIAN_POINT('Ctrl Pts',(1.96157995994097,-1.46872540345634,26.2604175451727));
#6581=CARTESIAN_POINT('Ctrl Pts',(2.01049150583093,-1.40340079750775,26.264658796041));
#6582=CARTESIAN_POINT('Ctrl Pts',(2.05619138227902,-1.33555675297573,26.2689000469093));
#6583=CARTESIAN_POINT('Ctrl Pts',(2.09841545546451,-1.26554447818623,26.2731412977776));
#6584=CARTESIAN_POINT('Ctrl Pts',(2.14039809031562,-1.19593253538123,26.2773582970646));
#6585=CARTESIAN_POINT('Ctrl Pts',(2.17894432091357,-1.12417749326991,26.2815752963515));
#6586=CARTESIAN_POINT('Ctrl Pts',(2.21383723189393,-1.05065453917081,26.2857922956384));
#6587=CARTESIAN_POINT('Ctrl Pts',(2.24871857511094,-0.977155959539449,26.2900078968979));
#6588=CARTESIAN_POINT('Ctrl Pts',(2.27994880462219,-0.901891051631597,26.2942234981573));
#6589=CARTESIAN_POINT('Ctrl Pts',(2.30735747623874,-0.825258581806462,26.2984390994167));
#6590=CARTESIAN_POINT('Ctrl Pts',(2.33476546393814,-0.748628024159358,26.302654595486));
#6591=CARTESIAN_POINT('Ctrl Pts',(2.35835192774011,-0.670630410702349,26.3068700915553));
#6592=CARTESIAN_POINT('Ctrl Pts',(2.37799549961059,-0.591682054681205,26.3110855876246));
#6593=CARTESIAN_POINT('Ctrl Pts',(2.39784722129216,-0.511897135661273,26.3153457524902));
#6594=CARTESIAN_POINT('Ctrl Pts',(2.41367186050755,-0.431141671582436,26.3196059173558));
#6595=CARTESIAN_POINT('Ctrl Pts',(2.42539699986717,-0.349856603532552,26.3238660822214));
#6596=CARTESIAN_POINT('Ctrl Pts',(2.43701609495931,-0.269306692245722,26.3280877173903));
#6597=CARTESIAN_POINT('Ctrl Pts',(2.44460956275498,-0.188237192057598,26.3323093525593));
#6598=CARTESIAN_POINT('Ctrl Pts',(2.44815928378296,-0.107081143192042,26.3365309877282));
#6599=CARTESIAN_POINT('Ctrl Pts',(2.45175760079407,-0.0248140611068261,
26.3408104174421));
#6600=CARTESIAN_POINT('Ctrl Pts',(2.45120061758862,0.0575414626740317,26.345089847156));
#6601=CARTESIAN_POINT('Ctrl Pts',(2.4465239643695,0.139537599827903,26.3493692768699));
#6602=CARTESIAN_POINT('Ctrl Pts',(2.44184731115039,0.221533736981752,26.3536487065838));
#6603=CARTESIAN_POINT('Ctrl Pts',(2.43305110558818,0.303170006760211,26.3579281362977));
#6604=CARTESIAN_POINT('Ctrl Pts',(2.4202246227018,0.384009147896178,26.3622075660116));
#6605=CARTESIAN_POINT('Ctrl Pts',(2.4075441887043,0.463927813259801,26.3664382679519));
#6606=CARTESIAN_POINT('Ctrl Pts',(2.39087714044248,0.543368013966587,26.3706689698921));
#6607=CARTESIAN_POINT('Ctrl Pts',(2.37027193396252,0.621901285631053,26.3748996718324));
#6608=CARTESIAN_POINT('Ctrl Pts',(2.34969633149461,0.700321726593133,26.3791242954181));
#6609=CARTESIAN_POINT('Ctrl Pts',(2.32519392503081,0.777837380339582,26.3833489190038));
#6610=CARTESIAN_POINT('Ctrl Pts',(2.29686456028903,0.85402777571242,26.3875735425894));
#6611=CARTESIAN_POINT('Ctrl Pts',(2.26842369677241,0.930518041407628,26.3918147934577));
#6612=CARTESIAN_POINT('Ctrl Pts',(2.23612576043026,1.0056721257536,26.396056044326));
#6613=CARTESIAN_POINT('Ctrl Pts',(2.20012302712518,1.07907780790523,26.4002972951943));
#6614=CARTESIAN_POINT('Ctrl Pts',(2.16432615837333,1.15206375448197,26.4045142944813));
#6615=CARTESIAN_POINT('Ctrl Pts',(2.12486695278524,1.2233208176833,26.4087312937682));
#6616=CARTESIAN_POINT('Ctrl Pts',(2.08194341137352,1.29246349342579,26.4129482930552));
#6617=CARTESIAN_POINT('Ctrl Pts',(2.03903410005481,1.36158324685864,26.4171638943146));
#6618=CARTESIAN_POINT('Ctrl Pts',(1.99266297873646,1.42858961002957,26.421379495574));
#6619=CARTESIAN_POINT('Ctrl Pts',(1.94307303273185,1.49312338387364,26.4255950968335));
#6620=CARTESIAN_POINT('Ctrl Pts',(1.89348432412446,1.55765554743338,26.4298105929028));
#6621=CARTESIAN_POINT('Ctrl Pts',(1.84067723475091,1.61971487623718,26.4340260889721));
#6622=CARTESIAN_POINT('Ctrl Pts',(1.78493607301311,1.67897393227427,26.4382415850414));
#6623=CARTESIAN_POINT('Ctrl Pts',(1.7286042594142,1.73886091694874,26.442501749907));
#6624=CARTESIAN_POINT('Ctrl Pts',(1.66927614260175,1.79588756633635,26.4467619147726));
#6625=CARTESIAN_POINT('Ctrl Pts',(1.60728323947997,1.84975426424343,26.4510220796382));
#6626=CARTESIAN_POINT('Ctrl Pts',(1.5458510113146,1.90313378205441,26.4552437148071));
#6627=CARTESIAN_POINT('Ctrl Pts',(1.48180241256385,1.95341003501743,26.4594653499761));
#6628=CARTESIAN_POINT('Ctrl Pts',(1.41549171495736,2.00033333594356,26.463686985145));
#6629=CARTESIAN_POINT('Ctrl Pts',(1.3482732182542,2.04789902085493,26.4679664148589));
#6630=CARTESIAN_POINT('Ctrl Pts',(1.27873063476726,2.09201898923055,26.4722458445728));
#6631=CARTESIAN_POINT('Ctrl Pts',(1.20725977014175,2.13248073787251,26.4765252742868));
#6632=CARTESIAN_POINT('Ctrl Pts',(1.13578890551627,2.17294248651446,26.4808047040007));
#6633=CARTESIAN_POINT('Ctrl Pts',(1.06239022765329,2.20974585407228,26.4850841337146));
#6634=CARTESIAN_POINT('Ctrl Pts',(0.987479701805511,2.24272916075974,26.4893635634285));
#6635=CARTESIAN_POINT('Ctrl Pts',(0.91342214548648,2.27533690266184,26.4935942653687));
#6636=CARTESIAN_POINT('Ctrl Pts',(0.837608461737238,2.30433382219647,26.497824967309));
#6637=CARTESIAN_POINT('Ctrl Pts',(0.760425119890666,2.32952868345493,26.5020556692492));
#6638=CARTESIAN_POINT('Ctrl Pts',(0.68335266926873,2.35468734663032,26.5062802928349));
#6639=CARTESIAN_POINT('Ctrl Pts',(0.604914907103,2.37605465728765,26.5105049164206));
#6640=CARTESIAN_POINT('Ctrl Pts',(0.525519405337245,2.39348691339936,26.5147295400063));
#6641=CARTESIAN_POINT('Ctrl Pts',(0.445811418584786,2.41098777942218,26.5189707908746));
#6642=CARTESIAN_POINT('Ctrl Pts',(0.365138571433456,2.42452235803861,26.5232120417429));
#6643=CARTESIAN_POINT('Ctrl Pts',(0.283929885615853,2.4339954950768,26.5274532926112));
#6644=CARTESIAN_POINT('Ctrl Pts',(0.203185553148079,2.44341446447427,26.5316702918981));
#6645=CARTESIAN_POINT('Ctrl Pts',(0.121911959835773,2.44881825868422,26.5358872911851));
#6646=CARTESIAN_POINT('Ctrl Pts',(0.0405404212310668,2.45016463206994,26.5401042904721));
#6647=CARTESIAN_POINT('Ctrl Pts',(-0.0408041409284087,2.45151055910343,
26.5443198917315));
#6648=CARTESIAN_POINT('Ctrl Pts',(-0.122246119270063,2.44880172881243,26.5485354929909));
#6649=CARTESIAN_POINT('Ctrl Pts',(-0.203351959350605,2.44204795829817,26.5527510942504));
#6650=CARTESIAN_POINT('Ctrl Pts',(-0.284455775630999,2.43529435630793,26.5569665903197));
#6651=CARTESIAN_POINT('Ctrl Pts',(-0.365223006960328,2.42449605444537,26.561182086389));
#6652=CARTESIAN_POINT('Ctrl Pts',(-0.445224429430876,2.40971480832026,26.5653975824583));
#6653=CARTESIAN_POINT('Ctrl Pts',(-0.52607357354143,2.39477693520253,26.5696577473239));
#6654=CARTESIAN_POINT('Ctrl Pts',(-0.606140103296564,2.37577127820766,26.5739179121894));
#6655=CARTESIAN_POINT('Ctrl Pts',(-0.684992626948215,2.35281434691022,26.578178077055));
#6656=CARTESIAN_POINT('Ctrl Pts',(-0.763131994206052,2.33006504222483,26.582399712224));
#6657=CARTESIAN_POINT('Ctrl Pts',(-0.840078802226663,2.30343585993539,26.5866213473929));
#6658=CARTESIAN_POINT('Ctrl Pts',(-0.915431317716265,2.27308947306178,26.5908429825619));
#6659=CARTESIAN_POINT('Ctrl Pts',(-0.991815415558578,2.24232764156811,26.5951224122758));
#6660=CARTESIAN_POINT('Ctrl Pts',(-1.0665607894182,2.20774626487489,26.5994018419897));
#6661=CARTESIAN_POINT('Ctrl Pts',(-1.13927448176761,2.16956306780724,26.6036812717035));
#6662=CARTESIAN_POINT('Ctrl Pts',(-1.21198817411702,2.13137987073958,26.6079607014174));
#6663=CARTESIAN_POINT('Ctrl Pts',(-1.28266979597243,2.08959515933178,26.6122401311313));
#6664=CARTESIAN_POINT('Ctrl Pts',(-1.35095820532172,2.04447112414774,26.6165195608451));
#6665=CARTESIAN_POINT('Ctrl Pts',(-1.41832965217767,1.99995300508045,26.6207415272709));
#6666=CARTESIAN_POINT('Ctrl Pts',(-1.48362752635917,1.95201570998207,26.6249634936967));
#6667=CARTESIAN_POINT('Ctrl Pts',(-1.54648268776721,1.90087915092893,26.6291854601224));
#6668=CARTESIAN_POINT('Ctrl Pts',(-1.60924745713461,1.84981613138824,26.6334013549361));
#6669=CARTESIAN_POINT('Ctrl Pts',(-1.66957613039096,1.79556327676192,26.6376172497497));
#6670=CARTESIAN_POINT('Ctrl Pts',(-1.72712802140379,1.73838403342927,26.6418331445633));
#6671=CARTESIAN_POINT('Ctrl Pts',(-1.78461321438355,1.68127105626088,26.6460441534925));
#6672=CARTESIAN_POINT('Ctrl Pts',(-1.83932769036454,1.6212387574482,26.6502551624216));
#6673=CARTESIAN_POINT('Ctrl Pts',(-1.8909645520255,1.55859016838392,26.6544661713508));
#6674=CARTESIAN_POINT('Ctrl Pts',(-1.94256868566679,1.49598128669512,26.6586745112954));
#6675=CARTESIAN_POINT('Ctrl Pts',(-1.99109878021824,1.4307597655692,26.6628828512401));
#6676=CARTESIAN_POINT('Ctrl Pts',(-2.03628630091386,1.36326385953364,26.6670911911847));
#6677=CARTESIAN_POINT('Ctrl Pts',(-2.08145918883104,1.29578981025462,26.6712981683703));
#6678=CARTESIAN_POINT('Ctrl Pts',(-2.1232913924644,1.22604322647842,26.6755051455558));
#6679=CARTESIAN_POINT('Ctrl Pts',(-2.16155690934235,1.15439247124813,26.6797121227413));
#6680=CARTESIAN_POINT('Ctrl Pts',(-2.19982189664528,1.08274270762734,26.6839190417044));
#6681=CARTESIAN_POINT('Ctrl Pts',(-2.23452007640588,1.00918923772036,26.6881259606676));
#6682=CARTESIAN_POINT('Ctrl Pts',(-2.26547144885562,0.934124919065986,26.6923328796307));
#6683=CARTESIAN_POINT('Ctrl Pts',(-2.29645345916513,0.858986296434502,26.6965439629001));
#6684=CARTESIAN_POINT('Ctrl Pts',(-2.32368107498441,0.782334270583932,26.7007550461695));
#6685=CARTESIAN_POINT('Ctrl Pts',(-2.34702275463055,0.704581038097405,26.7049661294388));
#6686=CARTESIAN_POINT('Ctrl Pts',(-2.37037558795416,0.626790651708913,26.7091792249484));
#6687=CARTESIAN_POINT('Ctrl Pts',(-2.38983867445901,0.547898464758642,26.7133923204579));
#6688=CARTESIAN_POINT('Ctrl Pts',(-2.40533126163322,0.46832870060454,26.7176054159674));
#6689=CARTESIAN_POINT('Ctrl Pts',(-2.42085181558977,0.388615299351612,26.7218261168383));
#6690=CARTESIAN_POINT('Ctrl Pts',(-2.43238748256542,0.308222340536783,26.7260468177092));
#6691=CARTESIAN_POINT('Ctrl Pts',(-2.43990926163117,0.227580853778281,26.7302675185802));
#6692=CARTESIAN_POINT('Ctrl Pts',(-2.44698128365247,0.151761241795204,26.7342358469828));
#6693=CARTESIAN_POINT('Ctrl Pts',(-2.45050555932684,0.0757222904315045,
26.7382041753854));
#6694=CARTESIAN_POINT('Ctrl Pts',(-2.45049999341142,-0.000179695899241593,
26.742172503788));
#6695=CARTESIAN_POINT('',(-2.45049902004185,0.00219152320424601,27.542172503788));
#6696=CARTESIAN_POINT('Ctrl Pts',(-2.45452295415184,-0.000179990904159599,
26.742172503788));
#6697=CARTESIAN_POINT('Ctrl Pts',(-2.45453308230378,-0.00977866906062366,
26.742673521946));
#6698=CARTESIAN_POINT('Ctrl Pts',(-2.45448165679552,-0.0193772356258571,
26.7431745401039));
#6699=CARTESIAN_POINT('Ctrl Pts',(-2.44478272895187,-0.840936602767608,
26.7860608907341));
#6700=CARTESIAN_POINT('Ctrl Pts',(-1.53984852038364,-2.45440278088368,26.8708315556785));
#6701=CARTESIAN_POINT('Ctrl Pts',(1.22986537187606,-2.62348196936699,26.9979875530954));
#6702=CARTESIAN_POINT('Ctrl Pts',(2.87157588413716,-0.386365653463097,27.125143550512));
#6703=CARTESIAN_POINT('Ctrl Pts',(1.87954503144942,2.20511608567141,27.2522995479289));
#6704=CARTESIAN_POINT('Ctrl Pts',(-0.836359992199049,2.77411759663995,27.3794555453455));
#6705=CARTESIAN_POINT('Ctrl Pts',(-2.31723874763037,1.2730729954971,27.4760796842579));
#6706=CARTESIAN_POINT('Ctrl Pts',(-2.4513351212562,0.230535148772026,27.5303184906982));
#6707=CARTESIAN_POINT('Ctrl Pts',(-2.44936820280003,0.00220089695502133,
27.5421719646662));
#6708=CARTESIAN_POINT('',(-2.45026626984745,-0.000935076283515541,28.3421725466424));
#6709=CARTESIAN_POINT('Ctrl Pts',(-2.45049902004185,0.00219152320424601,
27.542172503788));
#6710=CARTESIAN_POINT('Ctrl Pts',(-2.45057110097415,-0.0784073286065062,
27.5463547214738));
#6711=CARTESIAN_POINT('Ctrl Pts',(-2.44666247325055,-0.159090238606502,
27.5505369391595));
#6712=CARTESIAN_POINT('Ctrl Pts',(-2.43877499133098,-0.239430139411436,
27.5547191568453));
#6713=CARTESIAN_POINT('Ctrl Pts',(-2.43089124206684,-0.319732020329891,
27.5588993953471));
#6714=CARTESIAN_POINT('Ctrl Pts',(-2.41903242136486,-0.399690743455314,
27.5630796338489));
#6715=CARTESIAN_POINT('Ctrl Pts',(-2.40325239789582,-0.478882200554593,
27.5672598723508));
#6716=CARTESIAN_POINT('Ctrl Pts',(-2.3874748013853,-0.558061478053362,27.5714394679343));
#6717=CARTESIAN_POINT('Ctrl Pts',(-2.36777729279802,-0.63647325944333,27.5756190635179));
#6718=CARTESIAN_POINT('Ctrl Pts',(-2.34426496445741,-0.713703037976942,
27.5797986591014));
#6719=CARTESIAN_POINT('Ctrl Pts',(-2.32074874143595,-0.790945609175494,
27.5839789470107));
#6720=CARTESIAN_POINT('Ctrl Pts',(-2.29341658455421,-0.867005336428038,
27.5881592349201));
#6721=CARTESIAN_POINT('Ctrl Pts',(-2.26242315094726,-0.941483794899246,
27.5923395228294));
#6722=CARTESIAN_POINT('Ctrl Pts',(-2.23139545641689,-1.01604458373739,27.5965244317344));
#6723=CARTESIAN_POINT('Ctrl Pts',(-2.196698593716,-1.08902017892509,27.6007093406394));
#6724=CARTESIAN_POINT('Ctrl Pts',(-2.15853467669294,-1.16003374929961,27.6048942495445));
#6725=CARTESIAN_POINT('Ctrl Pts',(-2.12034575527327,-1.2310938466456,27.6090819003358));
#6726=CARTESIAN_POINT('Ctrl Pts',(-2.07868550646591,-1.30018895778965,27.6132695511272));
#6727=CARTESIAN_POINT('Ctrl Pts',(-2.03379981297051,-1.36697058152731,27.6174572019185));
#6728=CARTESIAN_POINT('Ctrl Pts',(-1.98884110883246,-1.43386083161975,27.6216516643029));
#6729=CARTESIAN_POINT('Ctrl Pts',(-1.94064677863042,-1.49842971071796,27.6258461266873));
#6730=CARTESIAN_POINT('Ctrl Pts',(-1.88950296486415,-1.56036175157223,27.6300405890716));
#6731=CARTESIAN_POINT('Ctrl Pts',(-1.87435517587577,-1.5787048006606,27.6312829061074));
#6732=CARTESIAN_POINT('Ctrl Pts',(-1.85894889207162,-1.59681678924659,27.6325252231432));
#6733=CARTESIAN_POINT('Ctrl Pts',(-1.84329213690865,-1.61469017090299,27.633767540179));
#6734=CARTESIAN_POINT('Ctrl Pts',(-1.78997316716346,-1.67555784660354,27.6379982421193));
#6735=CARTESIAN_POINT('Ctrl Pts',(-1.73353580191242,-1.73389616839656,27.6422289440595));
#6736=CARTESIAN_POINT('Ctrl Pts',(-1.6742493745229,-1.78936840307123,27.6464596459998));
#6737=CARTESIAN_POINT('Ctrl Pts',(-1.61504812541635,-1.84476093940835,27.6506842695855));
#6738=CARTESIAN_POINT('Ctrl Pts',(-1.55300628043507,-1.89729525171571,27.6549088931712));
#6739=CARTESIAN_POINT('Ctrl Pts',(-1.48843239794904,-1.94666875629514,27.6591335167569));
#6740=CARTESIAN_POINT('Ctrl Pts',(-1.42360436543733,-1.99623658522016,27.6633747676251));
#6741=CARTESIAN_POINT('Ctrl Pts',(-1.3562246341688,-2.04261831545966,27.6676160184934));
#6742=CARTESIAN_POINT('Ctrl Pts',(-1.28664173093568,-2.08554628484118,27.6718572693617));
#6743=CARTESIAN_POINT('Ctrl Pts',(-1.21745670452936,-2.12822879099186,27.6760742686487));
#6744=CARTESIAN_POINT('Ctrl Pts',(-1.14609403315353,-2.16749667985583,27.6802912679356));
#6745=CARTESIAN_POINT('Ctrl Pts',(-1.07292669755125,-2.20312926349812,27.6845082672226));
#6746=CARTESIAN_POINT('Ctrl Pts',(-0.999783618521376,-2.23875003415941,
27.688723868482));
#6747=CARTESIAN_POINT('Ctrl Pts',(-0.924837481141474,-2.27073768942765,
27.6929394697414));
#6748=CARTESIAN_POINT('Ctrl Pts',(-0.848485312637826,-2.29891777239594,
27.6971550710009));
#6749=CARTESIAN_POINT('Ctrl Pts',(-0.772135049318076,-2.32709715219834,
27.7013705670702));
#6750=CARTESIAN_POINT('Ctrl Pts',(-0.694379261299073,-2.35146898859246,
27.7055860631395));
#6751=CARTESIAN_POINT('Ctrl Pts',(-0.615633016713064,-2.37190772137804,
27.7098015592088));
#6752=CARTESIAN_POINT('Ctrl Pts',(-0.536052350768313,-2.39256302976379,
27.7140617240744));
#6753=CARTESIAN_POINT('Ctrl Pts',(-0.455460577743858,-2.40920124798699,
27.7183218889399));
#6754=CARTESIAN_POINT('Ctrl Pts',(-0.374297886007632,-2.4217455156416,27.7225820538055));
#6755=CARTESIAN_POINT('Ctrl Pts',(-0.293869244240767,-2.43417633068528,
27.7268036889745));
#6756=CARTESIAN_POINT('Ctrl Pts',(-0.212880443295209,-2.44258696296556,
27.7310253241435));
#6757=CARTESIAN_POINT('Ctrl Pts',(-0.131764318647519,-2.44695492691046,
27.7352469593124));
#6758=CARTESIAN_POINT('Ctrl Pts',(-0.0495377073466007,-2.45138268865368,
27.7395263890263));
#6759=CARTESIAN_POINT('Ctrl Pts',(0.0328192455463651,-2.4516562533755,27.7438058187402));
#6760=CARTESIAN_POINT('Ctrl Pts',(0.114858375165966,-2.44780673331336,27.7480852484541));
#6761=CARTESIAN_POINT('Ctrl Pts',(0.196897504785545,-2.44395721325122,27.752364678168));
#6762=CARTESIAN_POINT('Ctrl Pts',(0.278618329221147,-2.43598472122155,27.7566441078819));
#6763=CARTESIAN_POINT('Ctrl Pts',(0.359582709140937,-2.42397411811407,27.7609235375958));
#6764=CARTESIAN_POINT('Ctrl Pts',(0.439625187255609,-2.41210027387136,27.765154239536));
#6765=CARTESIAN_POINT('Ctrl Pts',(0.519229428312936,-2.39623519297798,27.7693849414763));
#6766=CARTESIAN_POINT('Ctrl Pts',(0.59796650105694,-2.37642300813927,27.7736156434165));
#6767=CARTESIAN_POINT('Ctrl Pts',(0.676590450292641,-2.35663928795868,27.7778402670022));
#6768=CARTESIAN_POINT('Ctrl Pts',(0.754349258430402,-2.33291983907704,27.7820648905878));
#6769=CARTESIAN_POINT('Ctrl Pts',(0.830821468792822,-2.30536026186645,27.7862895141735));
#6770=CARTESIAN_POINT('Ctrl Pts',(0.907594658645635,-2.27769221561246,27.7905307650418));
#6771=CARTESIAN_POINT('Ctrl Pts',(0.983070631995018,-2.24615381785988,27.7947720159101));
#6772=CARTESIAN_POINT('Ctrl Pts',(1.05683565332173,-2.21089317966021,27.7990132667784));
#6773=CARTESIAN_POINT('Ctrl Pts',(1.13017888436282,-2.17583416269497,27.8032302660653));
#6774=CARTESIAN_POINT('Ctrl Pts',(1.20183025301574,-2.13709556008903,27.8074472653523));
#6775=CARTESIAN_POINT('Ctrl Pts',(1.27140227804613,-2.0948714751457,27.8116642646392));
#6776=CARTESIAN_POINT('Ctrl Pts',(1.34095123842816,-2.05266138841028,27.8158798658986));
#6777=CARTESIAN_POINT('Ctrl Pts',(1.40842182686203,-2.00696835508931,27.8200954671581));
#6778=CARTESIAN_POINT('Ctrl Pts',(1.47345241214717,-1.95803172577405,27.8243110684175));
#6779=CARTESIAN_POINT('Ctrl Pts',(1.53848137475138,-1.90909631755397,27.8285265644868));
#6780=CARTESIAN_POINT('Ctrl Pts',(1.6010700843135,-1.85691775476208,27.8327420605561));
#6781=CARTESIAN_POINT('Ctrl Pts',(1.66088825234669,-1.80177702927325,27.8369575566254));
#6782=CARTESIAN_POINT('Ctrl Pts',(1.72134027355368,-1.74605201434518,27.8412177214909));
#6783=CARTESIAN_POINT('Ctrl Pts',(1.77896232133683,-1.68730200333099,27.8454778863565));
#6784=CARTESIAN_POINT('Ctrl Pts',(1.83345145153445,-1.6258554747782,27.8497380512221));
#6785=CARTESIAN_POINT('Ctrl Pts',(1.88744777224637,-1.56496467967213,27.8539596863911));
#6786=CARTESIAN_POINT('Ctrl Pts',(1.93836737087129,-1.50142635194949,27.85818132156));
#6787=CARTESIAN_POINT('Ctrl Pts',(1.98595700024085,-1.43559222733838,27.862402956729));
#6788=CARTESIAN_POINT('Ctrl Pts',(2.03419813568892,-1.36885682795531,27.8666823864429));
#6789=CARTESIAN_POINT('Ctrl Pts',(2.07901716722112,-1.29976271141826,27.8709618161568));
#6790=CARTESIAN_POINT('Ctrl Pts',(2.12019761091784,-1.22870352024331,27.8752412458707));
#6791=CARTESIAN_POINT('Ctrl Pts',(2.16137805461456,-1.15764432906833,27.8795206755846));
#6792=CARTESIAN_POINT('Ctrl Pts',(2.19891974441495,-1.08462052950557,27.8838001052985));
#6793=CARTESIAN_POINT('Ctrl Pts',(2.23265681392579,-1.01004643518541,27.8880795350124));
#6794=CARTESIAN_POINT('Ctrl Pts',(2.26600973592246,-0.936321479612911,27.8923102369527));
#6795=CARTESIAN_POINT('Ctrl Pts',(2.29576972894447,-0.860804072338553,27.8965409388929));
#6796=CARTESIAN_POINT('Ctrl Pts',(2.32174166943258,-0.783878734512165,27.9007716408332));
#6797=CARTESIAN_POINT('Ctrl Pts',(2.34767629538852,-0.707063917229848,27.9049962644189));
#6798=CARTESIAN_POINT('Ctrl Pts',(2.3698335301912,-0.62884562369093,27.9092208880045));
#6799=CARTESIAN_POINT('Ctrl Pts',(2.38806556893476,-0.549629955941546,27.9134455115902));
#6800=CARTESIAN_POINT('Ctrl Pts',(2.40636936537573,-0.470102510996157,27.9176867624585));
#6801=CARTESIAN_POINT('Ctrl Pts',(2.42071680629514,-0.389570256433736,27.9219280133268));
#6802=CARTESIAN_POINT('Ctrl Pts',(2.43100841586237,-0.308461232582512,27.9261692641951));
#6803=CARTESIAN_POINT('Ctrl Pts',(2.44124117774191,-0.227815992211736,27.930386263482));
#6804=CARTESIAN_POINT('Ctrl Pts',(2.44746430597289,-0.146601026615822,27.934603262769));
#6805=CARTESIAN_POINT('Ctrl Pts',(2.44963120743723,-0.0652472033854291,
27.9388202620559));
#6806=CARTESIAN_POINT('Ctrl Pts',(2.45179739052633,0.0160796492728611,27.9430358633154));
#6807=CARTESIAN_POINT('Ctrl Pts',(2.44991000487725,0.0975448036220795,27.9472514645748));
#6808=CARTESIAN_POINT('Ctrl Pts',(2.44397449488418,0.178714628264212,27.9514670658342));
#6809=CARTESIAN_POINT('Ctrl Pts',(2.43803913299742,0.259882427509452,27.9556825619035));
#6810=CARTESIAN_POINT('Ctrl Pts',(2.42805588260075,0.340754447956536,27.9598980579728));
#6811=CARTESIAN_POINT('Ctrl Pts',(2.41408216762736,0.420900864745565,27.9641135540421));
#6812=CARTESIAN_POINT('Ctrl Pts',(2.39996038252952,0.501896539583101,27.9683737189077));
#6813=CARTESIAN_POINT('Ctrl Pts',(2.38176312807834,0.582150661691083,27.9726338837733));
#6814=CARTESIAN_POINT('Ctrl Pts',(2.35960255752585,0.661230686309594,27.9768940486389));
#6815=CARTESIAN_POINT('Ctrl Pts',(2.33764241115584,0.739595496974264,27.9811156838078));
#6816=CARTESIAN_POINT('Ctrl Pts',(2.31179055803483,0.816806935920526,27.9853373189768));
#6817=CARTESIAN_POINT('Ctrl Pts',(2.28220561160531,0.892461649796356,27.9895589541458));
#6818=CARTESIAN_POINT('Ctrl Pts',(2.25221564474001,0.969152083147142,27.9938383838597));
#6819=CARTESIAN_POINT('Ctrl Pts',(2.218389801083,1.0442423942957,27.9981178135736));
#6820=CARTESIAN_POINT('Ctrl Pts',(2.18094183158237,1.11733745003653,28.0023972432875));
#6821=CARTESIAN_POINT('Ctrl Pts',(2.14349386208176,1.19043250577734,28.0066766730014));
#6822=CARTESIAN_POINT('Ctrl Pts',(2.10242406883352,1.26153191406017,28.0109561027153));
#6823=CARTESIAN_POINT('Ctrl Pts',(2.0579909871091,1.33027190715948,28.0152355324292));
#6824=CARTESIAN_POINT('Ctrl Pts',(2.0140638431598,1.3982291915692,28.0194662343694));
#6825=CARTESIAN_POINT('Ctrl Pts',(1.96668442764717,1.46413614849936,28.0236969363097));
#6826=CARTESIAN_POINT('Ctrl Pts',(1.91607038741418,1.52762054204389,28.0279276382499));
#6827=CARTESIAN_POINT('Ctrl Pts',(1.86552906563014,1.59101372598314,28.0321522618356));
#6828=CARTESIAN_POINT('Ctrl Pts',(1.81176263630591,1.65199089856441,28.0363768854213));
#6829=CARTESIAN_POINT('Ctrl Pts',(1.75503250946487,1.7102079232425,28.040601509007));
#6830=CARTESIAN_POINT('Ctrl Pts',(1.69807910406848,1.76865407861167,28.0448427598753));
#6831=CARTESIAN_POINT('Ctrl Pts',(1.6381388796792,1.82431791414242,28.0490840107436));
#6832=CARTESIAN_POINT('Ctrl Pts',(1.57551785703004,1.87688404867735,28.0533252616119));
#6833=CARTESIAN_POINT('Ctrl Pts',(1.51325490299569,1.92914960870578,28.0575422608988));
#6834=CARTESIAN_POINT('Ctrl Pts',(1.44834208503497,1.97835249506572,28.0617592601858));
#6835=CARTESIAN_POINT('Ctrl Pts',(1.38111643225006,2.02422025742478,28.0659762594728));
#6836=CARTESIAN_POINT('Ctrl Pts',(1.31391306623971,2.0700728136172,28.0701918607322));
#6837=CARTESIAN_POINT('Ctrl Pts',(1.244398771907,2.11259217957174,28.0744074619917));
#6838=CARTESIAN_POINT('Ctrl Pts',(1.17294107577154,2.1515481595279,28.0786230632511));
#6839=CARTESIAN_POINT('Ctrl Pts',(1.10148516269026,2.19050316743169,28.0828385593204));
#6840=CARTESIAN_POINT('Ctrl Pts',(1.02808635306628,2.22589474447314,28.0870540553897));
#6841=CARTESIAN_POINT('Ctrl Pts',(0.953137115381867,2.25753845798505,28.091269551459));
#6842=CARTESIAN_POINT('Ctrl Pts',(0.877393690685013,2.28951747879391,28.0955297163246));
#6843=CARTESIAN_POINT('Ctrl Pts',(0.800067224636503,2.31766853265157,28.0997898811902));
#6844=CARTESIAN_POINT('Ctrl Pts',(0.721582103596555,2.34185172839127,28.1040500460557));
#6845=CARTESIAN_POINT('Ctrl Pts',(0.643806816095354,2.36581620696289,28.1082716812247));
#6846=CARTESIAN_POINT('Ctrl Pts',(0.564894218405332,2.38588425469449,28.1124933163937));
#6847=CARTESIAN_POINT('Ctrl Pts',(0.485269308088415,2.40197084674802,28.1167149515627));
#6848=CARTESIAN_POINT('Ctrl Pts',(0.404554325969565,2.41827766561645,28.1209943812765));
#6849=CARTESIAN_POINT('Ctrl Pts',(0.32310786949343,2.43049311709884,28.1252738109904));
#6850=CARTESIAN_POINT('Ctrl Pts',(0.241377877170622,2.43858298411446,28.1295532407043));
#6851=CARTESIAN_POINT('Ctrl Pts',(0.159647884847813,2.44667285113009,28.1338326704182));
#6852=CARTESIAN_POINT('Ctrl Pts',(0.0776348498558789,2.45063717540778,28.1381121001321));
#6853=CARTESIAN_POINT('Ctrl Pts',(-0.0042154132946402,2.45049637426599,
28.1423915298459));
#6854=CARTESIAN_POINT('Ctrl Pts',(-0.0851336875212073,2.45035717635795,
28.1466222317862));
#6855=CARTESIAN_POINT('Ctrl Pts',(-0.166197234216248,2.44620538357499,28.1508529337264));
#6856=CARTESIAN_POINT('Ctrl Pts',(-0.246975256662254,2.43802245120848,28.1550836356667));
#6857=CARTESIAN_POINT('Ctrl Pts',(-0.327637223316661,2.42985127546419,28.1593082592524));
#6858=CARTESIAN_POINT('Ctrl Pts',(-0.408014021674497,2.41766050912256,28.1635328828381));
#6859=CARTESIAN_POINT('Ctrl Pts',(-0.48767478586299,2.40148361502499,28.1677575064237));
#6860=CARTESIAN_POINT('Ctrl Pts',(-0.567649079058921,2.38524305187275,28.171998757292));
#6861=CARTESIAN_POINT('Ctrl Pts',(-0.646901215105209,2.3649849172612,28.1762400081603));
#6862=CARTESIAN_POINT('Ctrl Pts',(-0.725000351671044,2.34079574932903,28.1804812590286));
#6863=CARTESIAN_POINT('Ctrl Pts',(-0.802652915369348,2.31674489567998,28.1846982583155));
#6864=CARTESIAN_POINT('Ctrl Pts',(-0.879165180861529,2.2888079811939,28.1889152576025));
#6865=CARTESIAN_POINT('Ctrl Pts',(-0.95412561193247,2.25712085778642,28.1931322568895));
#6866=CARTESIAN_POINT('Ctrl Pts',(-1.02906119198054,2.22544423935359,28.1973478581489));
#6867=CARTESIAN_POINT('Ctrl Pts',(-1.10244553123049,2.19002006186729,28.2015634594083));
#6868=CARTESIAN_POINT('Ctrl Pts',(-1.17388610765331,2.15103269530209,28.2057790606678));
#6869=CARTESIAN_POINT('Ctrl Pts',(-1.24532490144929,2.11204630157234,28.2099945567371));
#6870=CARTESIAN_POINT('Ctrl Pts',(-1.31481962114464,2.06949711927496,28.2142100528064));
#6871=CARTESIAN_POINT('Ctrl Pts',(-1.38200271650126,2.02361526520807,28.2184255488757));
#6872=CARTESIAN_POINT('Ctrl Pts',(-1.44989770624718,1.97724723177853,28.2226857137413));
#6873=CARTESIAN_POINT('Ctrl Pts',(-1.5154313813222,1.92747573776811,28.2269458786069));
#6874=CARTESIAN_POINT('Ctrl Pts',(-1.57825635937258,1.87458185046693,28.2312060434724));
#6875=CARTESIAN_POINT('Ctrl Pts',(-1.64051313703158,1.82216634498773,28.2354276786414));
#6876=CARTESIAN_POINT('Ctrl Pts',(-1.70010971435821,1.76668506359559,28.2396493138104));
#6877=CARTESIAN_POINT('Ctrl Pts',(-1.75674450736549,1.70844929273338,28.2438709489794));
#6878=CARTESIAN_POINT('Ctrl Pts',(-1.81415463551125,1.64941626920954,28.2481503786932));
#6879=CARTESIAN_POINT('Ctrl Pts',(-1.86852094463015,1.58755313834589,28.2524298084071));
#6880=CARTESIAN_POINT('Ctrl Pts',(-1.91957214723803,1.52321798228224,28.256709238121));
#6881=CARTESIAN_POINT('Ctrl Pts',(-1.9706233498459,1.4588828262186,28.2609886678349));
#6882=CARTESIAN_POINT('Ctrl Pts',(-2.01835921401441,1.39207608219018,28.2652680975488));
#6883=CARTESIAN_POINT('Ctrl Pts',(-2.06255553650031,1.32318362627866,28.2695475272627));
#6884=CARTESIAN_POINT('Ctrl Pts',(-2.10727116745891,1.25348168138597,28.2738772404387));
#6885=CARTESIAN_POINT('Ctrl Pts',(-2.14852584144257,1.1813923810335,28.2782069536148));
#6886=CARTESIAN_POINT('Ctrl Pts',(-2.18606292576872,1.10728457705303,28.2825366667908));
#6887=CARTESIAN_POINT('Ctrl Pts',(-2.22353816353643,1.03329887399521,28.2868592462786));
#6888=CARTESIAN_POINT('Ctrl Pts',(-2.25730779196065,0.957301663987129,28.2911818257663));
#6889=CARTESIAN_POINT('Ctrl Pts',(-2.28715895920242,0.879689800634359,28.2955044052541));
#6890=CARTESIAN_POINT('Ctrl Pts',(-2.31695826439981,0.802212776561693,28.2998194748911));
#6891=CARTESIAN_POINT('Ctrl Pts',(-2.34285250298353,0.723127087240737,28.3041345445282));
#6892=CARTESIAN_POINT('Ctrl Pts',(-2.36467584532766,0.642851768702489,28.3084496141652));
#6893=CARTESIAN_POINT('Ctrl Pts',(-2.38647684186234,0.562658647333804,28.3127602654267));
#6894=CARTESIAN_POINT('Ctrl Pts',(-2.40421511332852,0.481278736729459,28.3170709166881));
#6895=CARTESIAN_POINT('Ctrl Pts',(-2.41777398446114,0.399148105423142,28.3213815679495));
#6896=CARTESIAN_POINT('Ctrl Pts',(-2.43132082051003,0.317090374656657,28.3256883930038));
#6897=CARTESIAN_POINT('Ctrl Pts',(-2.44069556608515,0.23428367808359,28.3299952180582));
#6898=CARTESIAN_POINT('Ctrl Pts',(-2.44583244848935,0.151175010886655,28.3343020431125));
#6899=CARTESIAN_POINT('Ctrl Pts',(-2.4489615618112,0.100549667103463,28.3369255300043));
#6900=CARTESIAN_POINT('Ctrl Pts',(-2.45051917085278,0.0498124829442886,
28.3395490168962));
#6901=CARTESIAN_POINT('Ctrl Pts',(-2.45049982187577,-0.000934337642672194,
28.342172503788));
#6902=CARTESIAN_POINT('',(-2.45279378259028,-0.00178251821640208,29.142172503788));
#6903=CARTESIAN_POINT('Ctrl Pts',(-2.44679612755061,-0.000946051092217225,
28.3421731833771));
#6904=CARTESIAN_POINT('Ctrl Pts',(-2.44799346344638,-0.352013542706997,
28.3603499638112));
#6905=CARTESIAN_POINT('Ctrl Pts',(-2.21301223344718,-1.52018191572573,28.4209120767176));
#6906=CARTESIAN_POINT('Ctrl Pts',(-0.415304599242627,-2.86753353361047,
28.5238595220962));
#6907=CARTESIAN_POINT('Ctrl Pts',(2.18604956098726,-1.90168709135936,28.651015519513));
#6908=CARTESIAN_POINT('Ctrl Pts',(2.78241085774888,0.808341694590506,28.7781715169296));
#6909=CARTESIAN_POINT('Ctrl Pts',(0.826810839185443,2.77697863022819,28.9053275143464));
#6910=CARTESIAN_POINT('Ctrl Pts',(-1.7628525210818,2.22511821664602,29.0266611766324));
#6911=CARTESIAN_POINT('Ctrl Pts',(-2.44705224933042,0.700008483504726,29.1056095064463));
#6912=CARTESIAN_POINT('Ctrl Pts',(-2.45279378259028,-0.00178251821640208,
29.142172503788));
#6913=CARTESIAN_POINT('',(-2.45241907602745,0.00192082108273114,29.942172503788));
#6914=CARTESIAN_POINT('Ctrl Pts',(-2.45279378259028,-0.00178251821640208,
29.142172503788));
#6915=CARTESIAN_POINT('Ctrl Pts',(-2.45370807116707,-0.113536551002519,
29.1479948389186));
#6916=CARTESIAN_POINT('Ctrl Pts',(-2.39595458088149,-1.0378852598289,29.1962025065213));
#6917=CARTESIAN_POINT('Ctrl Pts',(-1.22083214377427,-2.62769772866914,29.2867955065966));
#6918=CARTESIAN_POINT('Ctrl Pts',(1.54828364844088,-2.44909048842879,29.4139515040134));
#6919=CARTESIAN_POINT('Ctrl Pts',(2.89735036164549,-0.0242354782711104,
29.54110750143));
#6920=CARTESIAN_POINT('Ctrl Pts',(1.58903596980293,2.42284773834526,29.6682634988467));
#6921=CARTESIAN_POINT('Ctrl Pts',(-1.17670456466042,2.6477524136598,29.7954194962635));
#6922=CARTESIAN_POINT('Ctrl Pts',(-2.38767422187209,1.06551615028153,29.8867224979106));
#6923=CARTESIAN_POINT('Ctrl Pts',(-2.45349906928597,0.127352511453818,29.9356401670854));
#6924=CARTESIAN_POINT('Ctrl Pts',(-2.45241907602745,0.00192082108273114,
29.942172503788));
#6925=CARTESIAN_POINT('',(-2.44665768414027,0.000722135787914535,30.742172503788));
#6926=CARTESIAN_POINT('Ctrl Pts',(-2.45241907602745,0.00192082108273114,
29.942172503788));
#6927=CARTESIAN_POINT('Ctrl Pts',(-2.44649148908702,-0.686516114889533,
29.9780254995576));
#6928=CARTESIAN_POINT('Ctrl Pts',(-1.78473050610832,-2.19879978302826,30.0562638277996));
#6929=CARTESIAN_POINT('Ctrl Pts',(0.780241187801395,-2.79042114480829,30.1768874885137));
#6930=CARTESIAN_POINT('Ctrl Pts',(2.76849939206588,-0.854773415978033,30.3040434859304));
#6931=CARTESIAN_POINT('Ctrl Pts',(2.21755554772779,1.86485223792129,30.4311994833472));
#6932=CARTESIAN_POINT('Ctrl Pts',(-0.367277704650069,2.87407960296904,30.558355480764));
#6933=CARTESIAN_POINT('Ctrl Pts',(-2.19982864253972,1.54790246893413,30.6620131542442));
#6934=CARTESIAN_POINT('Ctrl Pts',(-2.44761904790825,0.365558552703536,30.7232854952522));
#6935=CARTESIAN_POINT('Ctrl Pts',(-2.44665768414027,0.000722135787914535,
30.742172503788));
#6936=CARTESIAN_POINT('',(-2.45049898092438,-0.00223483524436902,31.5421725268725));
#6937=CARTESIAN_POINT('Ctrl Pts',(-2.44665768414027,0.000722135787914535,
30.742172503788));
#6938=CARTESIAN_POINT('Ctrl Pts',(-2.44546160074793,-0.453190101942719,
30.7656708277245));
#6939=CARTESIAN_POINT('Ctrl Pts',(-2.10644501446377,-1.72751139562769,30.831554484133));
#6940=CARTESIAN_POINT('Ctrl Pts',(-0.053452762941805,-2.89695862564268,
30.9398234730143));
#6941=CARTESIAN_POINT('Ctrl Pts',(2.40669979930934,-1.61338853117316,31.0669794704308));
#6942=CARTESIAN_POINT('Ctrl Pts',(2.65948432735196,1.1499432982076,31.1941354678477));
#6943=CARTESIAN_POINT('Ctrl Pts',(0.473052841258751,2.85857437999996,31.3212914652642));
#6944=CARTESIAN_POINT('Ctrl Pts',(-1.91761420212668,2.02541820437966,31.4373038105778));
#6945=CARTESIAN_POINT('Ctrl Pts',(-2.44440761753277,0.599329367090551,31.510930823419));
#6946=CARTESIAN_POINT('Ctrl Pts',(-2.44976484792678,-0.00223372122999444,
31.542172503788));
#6947=CARTESIAN_POINT('',(-2.4504999619844,0.000431641585035285,32.3421725038399));
#6948=CARTESIAN_POINT('Ctrl Pts',(-2.45049898092438,-0.00223483524436902,
31.5421725268725));
#6949=CARTESIAN_POINT('Ctrl Pts',(-2.45040110829245,-0.109552269678379,
31.5477443490767));
#6950=CARTESIAN_POINT('Ctrl Pts',(-2.44324902256407,-0.216554533994056,
31.5533161712809));
#6951=CARTESIAN_POINT('Ctrl Pts',(-2.42919252957392,-0.322449847669802,
31.5588879934852));
#6952=CARTESIAN_POINT('Ctrl Pts',(-2.41513603658376,-0.428345161345525,
31.5644598156894));
#6953=CARTESIAN_POINT('Ctrl Pts',(-2.39417533386796,-0.533133880352394,
31.5700316378937));
#6954=CARTESIAN_POINT('Ctrl Pts',(-2.36651425439528,-0.63605073205205,31.5756034600979));
#6955=CARTESIAN_POINT('Ctrl Pts',(-2.34551111066838,-0.714195817832348,
31.5798341620375));
#6956=CARTESIAN_POINT('Ctrl Pts',(-2.3205936439755,-0.791446421958622,31.5840648639771));
#6957=CARTESIAN_POINT('Ctrl Pts',(-2.29185503851243,-0.867381537989583,
31.5882955659167));
#6958=CARTESIAN_POINT('Ctrl Pts',(-2.26315772251778,-0.943207556152907,
31.5925201895017));
#6959=CARTESIAN_POINT('Ctrl Pts',(-2.23065033426261,-1.0177214085918,31.5967448130867));
#6960=CARTESIAN_POINT('Ctrl Pts',(-2.1944763240252,-1.09051543468805,31.6009694366717));
#6961=CARTESIAN_POINT('Ctrl Pts',(-2.15815994003323,-1.16359596368338,31.6052106875402));
#6962=CARTESIAN_POINT('Ctrl Pts',(-2.11814813313033,-1.23494264121655,31.6094519384086));
#6963=CARTESIAN_POINT('Ctrl Pts',(-2.07463562739865,-1.30416151742344,31.6136931892771));
#6964=CARTESIAN_POINT('Ctrl Pts',(-2.03137192730004,-1.37298459830609,31.6179101885634));
#6965=CARTESIAN_POINT('Ctrl Pts',(-1.98464770390385,-1.43970374779104,31.6221271878497));
#6966=CARTESIAN_POINT('Ctrl Pts',(-1.93470034788398,-1.50395638696659,31.626344187136));
#6967=CARTESIAN_POINT('Ctrl Pts',(-1.88476955050527,-1.56818772498667,31.6305597883947));
#6968=CARTESIAN_POINT('Ctrl Pts',(-1.83161802763735,-1.62995380963492,31.6347753896535));
#6969=CARTESIAN_POINT('Ctrl Pts',(-1.77552514303334,-1.68892294568356,31.6389909909123));
#6970=CARTESIAN_POINT('Ctrl Pts',(-1.71943365809156,-1.74789061030008,31.643206486981));
#6971=CARTESIAN_POINT('Ctrl Pts',(-1.66040127865333,-1.80406112886422,31.6474219830496));
#6972=CARTESIAN_POINT('Ctrl Pts',(-1.59874512760668,-1.85713873120828,31.6516374791183));
#6973=CARTESIAN_POINT('Ctrl Pts',(-1.53643564748726,-1.9107787614713,31.6558976439846));
#6974=CARTESIAN_POINT('Ctrl Pts',(-1.47144681661139,-1.96125960980886,31.660157808851));
#6975=CARTESIAN_POINT('Ctrl Pts',(-1.4041397835595,-2.00831813172751,31.6644179737174));
#6976=CARTESIAN_POINT('Ctrl Pts',(-1.33744148743178,-2.05495104790201,31.6686396088857));
#6977=CARTESIAN_POINT('Ctrl Pts',(-1.26846718406831,-2.09822309531822,31.672861244054));
#6978=CARTESIAN_POINT('Ctrl Pts',(-1.19759540765003,-2.13792317204701,31.6770828792224));
#6979=CARTESIAN_POINT('Ctrl Pts',(-1.12575339054285,-2.17816674622629,31.6813623089377));
#6980=CARTESIAN_POINT('Ctrl Pts',(-1.05196199707804,-2.21473958837186,31.6856417386531));
#6981=CARTESIAN_POINT('Ctrl Pts',(-0.976637160732151,-2.24747193670512,
31.6899211683685));
#6982=CARTESIAN_POINT('Ctrl Pts',(-0.901312324386287,-2.28020428503837,
31.6942005980838));
#6983=CARTESIAN_POINT('Ctrl Pts',(-0.824454527417686,-2.30909602823866,
31.6984800277992));
#6984=CARTESIAN_POINT('Ctrl Pts',(-0.746494414108302,-2.33403006401055,
31.7027594575145));
#6985=CARTESIAN_POINT('Ctrl Pts',(-0.669421994530779,-2.35868018809575,
31.706990159454));
#6986=CARTESIAN_POINT('Ctrl Pts',(-0.590982356308357,-2.37955503273655,
31.7112208613934));
#6987=CARTESIAN_POINT('Ctrl Pts',(-0.511579914801198,-2.39650500537178,
31.7154515633328));
#6988=CARTESIAN_POINT('Ctrl Pts',(-0.432291552754534,-2.4134306255602,31.7196761869176));
#6989=CARTESIAN_POINT('Ctrl Pts',(-0.352043585654261,-2.42644247676526,
31.7239008105024));
#6990=CARTESIAN_POINT('Ctrl Pts',(-0.271256422911951,-2.43544045359952,
31.7281254340872));
#6991=CARTESIAN_POINT('Ctrl Pts',(-0.19015129785996,-2.44447384469266,31.7323666849557));
#6992=CARTESIAN_POINT('Ctrl Pts',(-0.108503175726638,-2.4494615534512,31.7366079358243));
#6993=CARTESIAN_POINT('Ctrl Pts',(-0.0267486987488107,-2.4503540064887,
31.7408491866928));
#6994=CARTESIAN_POINT('Ctrl Pts',(0.0545383040101661,-2.4512413564566,31.7450661859788));
#6995=CARTESIAN_POINT('Ctrl Pts',(0.135929978927115,-2.44808015204618,31.7492831852649));
#6996=CARTESIAN_POINT('Ctrl Pts',(0.216992958931321,-2.44087367673426,31.753500184551));
#6997=CARTESIAN_POINT('Ctrl Pts',(0.298029064784172,-2.43366959052657,31.7577157858096));
#6998=CARTESIAN_POINT('Ctrl Pts',(0.378736229252866,-2.42242293775469,31.7619313870681));
#6999=CARTESIAN_POINT('Ctrl Pts',(0.458684326233931,-2.40718901186993,31.7661469883267));
#7000=CARTESIAN_POINT('Ctrl Pts',(0.538630428303458,-2.39195546611097,31.7703624843951));
#7001=CARTESIAN_POINT('Ctrl Pts',(0.617817043906377,-2.37273493317112,31.7745779804635));
#7002=CARTESIAN_POINT('Ctrl Pts',(0.695823807960785,-2.34963390303148,31.778793476532));
#7003=CARTESIAN_POINT('Ctrl Pts',(0.774657157628108,-2.32628808669429,31.7830536413986));
#7004=CARTESIAN_POINT('Ctrl Pts',(0.852285033565486,-2.29897916753167,31.7873138062652));
#7005=CARTESIAN_POINT('Ctrl Pts',(0.928290664940497,-2.26786831438343,31.7915739711318));
#7006=CARTESIAN_POINT('Ctrl Pts',(1.00360888769279,-2.23703883339574,31.7957956062999));
#7007=CARTESIAN_POINT('Ctrl Pts',(1.07733369203311,-2.20247616804236,31.800017241468));
#7008=CARTESIAN_POINT('Ctrl Pts',(1.14908264953657,-2.16438428069833,31.8042388766361));
#7009=CARTESIAN_POINT('Ctrl Pts',(1.2218138564265,-2.12577091214711,31.808518306352));
#7010=CARTESIAN_POINT('Ctrl Pts',(1.29251428319697,-2.08353121294873,31.8127977360678));
#7011=CARTESIAN_POINT('Ctrl Pts',(1.36081601004376,-2.03792297126476,31.8170771657837));
#7012=CARTESIAN_POINT('Ctrl Pts',(1.42911773689055,-1.99231472958079,31.8213565954996));
#7013=CARTESIAN_POINT('Ctrl Pts',(1.49502040911961,-1.94333829060324,31.8256360252155));
#7014=CARTESIAN_POINT('Ctrl Pts',(1.55819241617905,-1.89129232118202,31.8299154549314));
#7015=CARTESIAN_POINT('Ctrl Pts',(1.6206451145155,-1.83983897373917,31.8341461568758));
#7016=CARTESIAN_POINT('Ctrl Pts',(1.68066394662085,-1.78519214591414,31.8383768588202));
#7017=CARTESIAN_POINT('Ctrl Pts',(1.73790418615668,-1.72761086177967,31.8426075607646));
#7018=CARTESIAN_POINT('Ctrl Pts',(1.79506218721859,-1.67011230610637,31.8468321843544));
#7019=CARTESIAN_POINT('Ctrl Pts',(1.84944919910022,-1.60968799436825,31.8510568079442));
#7020=CARTESIAN_POINT('Ctrl Pts',(1.90075344280793,-1.54663719069916,31.8552814315341));
#7021=CARTESIAN_POINT('Ctrl Pts',(1.95225960980531,-1.48333823161887,31.8595226824013));
#7022=CARTESIAN_POINT('Ctrl Pts',(2.00065832399735,-1.41739236331834,31.8637639332686));
#7023=CARTESIAN_POINT('Ctrl Pts',(2.04567150290777,-1.34913985642374,31.8680051841358));
#7024=CARTESIAN_POINT('Ctrl Pts',(2.0904272953607,-1.2812776190322,31.8722221834269));
#7025=CARTESIAN_POINT('Ctrl Pts',(2.13183590600085,-1.21113544243133,31.876439182718));
#7026=CARTESIAN_POINT('Ctrl Pts',(2.16966546536988,-1.13907946096017,31.8806561820091));
#7027=CARTESIAN_POINT('Ctrl Pts',(2.20748248341228,-1.06704736762341,31.8848717832727));
#7028=CARTESIAN_POINT('Ctrl Pts',(2.24172259043297,-0.993103140799315,31.8890873845362));
#7029=CARTESIAN_POINT('Ctrl Pts',(2.272199399449,-0.917638348775607,31.8933029857998));
#7030=CARTESIAN_POINT('Ctrl Pts',(2.30267544798981,-0.842175439793632,31.8975184818732));
#7031=CARTESIAN_POINT('Ctrl Pts',(2.32938821208528,-0.765192472678752,31.9017339779466));
#7032=CARTESIAN_POINT('Ctrl Pts',(2.35219963335275,-0.687100527474102,31.90594947402));
#7033=CARTESIAN_POINT('Ctrl Pts',(2.37525277196634,-0.608181094252511,31.9102096388807));
#7034=CARTESIAN_POINT('Ctrl Pts',(2.39432124431858,-0.528129501324468,31.9144698037414));
#7035=CARTESIAN_POINT('Ctrl Pts',(2.40931490965848,-0.447383410619295,31.918729968602));
#7036=CARTESIAN_POINT('Ctrl Pts',(2.42417296962595,-0.367367601900139,31.922951603775));
#7037=CARTESIAN_POINT('Ctrl Pts',(2.43502963113984,-0.286670281456185,31.927173238948));
#7038=CARTESIAN_POINT('Ctrl Pts',(2.44184932582133,-0.205723406509574,31.931394874121));
#7039=CARTESIAN_POINT('Ctrl Pts',(2.44876238268193,-0.123668362210968,31.9356743038255));
#7040=CARTESIAN_POINT('Ctrl Pts',(2.45152708637817,-0.0413573732052278,
31.93995373353));
#7041=CARTESIAN_POINT('Ctrl Pts',(2.45016097810504,0.0407606596040527,31.9442331632345));
#7042=CARTESIAN_POINT('Ctrl Pts',(2.44879486983191,0.12287869241331,31.948512592939));
#7043=CARTESIAN_POINT('Ctrl Pts',(2.44329804777661,0.204803283923386,31.9527920226435));
#7044=CARTESIAN_POINT('Ctrl Pts',(2.4337420804574,0.286093928301343,31.957071452348));
#7045=CARTESIAN_POINT('Ctrl Pts',(2.42429492225696,0.36645895593286,31.9613021542828));
#7046=CARTESIAN_POINT('Ctrl Pts',(2.4108450974072,0.4465066803362,31.9655328562175));
#7047=CARTESIAN_POINT('Ctrl Pts',(2.39342374342147,0.525807031548982,31.9697635581523));
#7048=CARTESIAN_POINT('Ctrl Pts',(2.37602741912777,0.604993449977305,31.9739881817325));
#7049=CARTESIAN_POINT('Ctrl Pts',(2.35467099705921,0.683434177406247,31.9782128053127));
#7050=CARTESIAN_POINT('Ctrl Pts',(2.32943728494601,0.760705058155504,31.982437428893));
#7051=CARTESIAN_POINT('Ctrl Pts',(2.30410425789335,0.838280061929099,31.9866786797626));
#7052=CARTESIAN_POINT('Ctrl Pts',(2.27486341023248,0.914675519389063,31.9909199306323));
#7053=CARTESIAN_POINT('Ctrl Pts',(2.24185026990548,0.989473404051221,31.9951611815019));
#7054=CARTESIAN_POINT('Ctrl Pts',(2.20902589961482,1.06384359236989,31.9993781807835));
#7055=CARTESIAN_POINT('Ctrl Pts',(2.17247244941019,1.13663399850397,32.0035951800651));
#7056=CARTESIAN_POINT('Ctrl Pts',(2.13237221261915,1.20745144699475,32.0078121793466));
#7057=CARTESIAN_POINT('Ctrl Pts',(2.09228526993348,1.27824541795277,32.0120277806007));
#7058=CARTESIAN_POINT('Ctrl Pts',(2.0486541046455,1.34706732579171,32.0162433818548));
#7059=CARTESIAN_POINT('Ctrl Pts',(2.00170701861743,1.41354846454507,32.0204589831089));
#7060=CARTESIAN_POINT('Ctrl Pts',(1.95476110403985,1.4800279444231,32.0246744791729));
#7061=CARTESIAN_POINT('Ctrl Pts',(1.90449970238342,1.54416639208367,32.0288899752369));
#7062=CARTESIAN_POINT('Ctrl Pts',(1.85119368584224,1.60562517029904,32.0331054713009));
#7063=CARTESIAN_POINT('Ctrl Pts',(1.79732282089863,1.66773518630974,32.0373656361729));
#7064=CARTESIAN_POINT('Ctrl Pts',(1.74034273862756,1.72710802884717,32.0416258010449));
#7065=CARTESIAN_POINT('Ctrl Pts',(1.68057260332205,1.78343095604044,32.0458859659169));
#7066=CARTESIAN_POINT('Ctrl Pts',(1.62134304002219,1.839244488407,32.0501076010807));
#7067=CARTESIAN_POINT('Ctrl Pts',(1.55937408609916,1.89206279345411,32.0543292362446));
#7068=CARTESIAN_POINT('Ctrl Pts',(1.4950096556947,1.94162210004409,32.0585508714084));
#7069=CARTESIAN_POINT('Ctrl Pts',(1.42976407049276,1.991859877965,32.0628303011345));
#7070=CARTESIAN_POINT('Ctrl Pts',(1.36205733028204,2.03874846821665,32.0671097308605));
#7071=CARTESIAN_POINT('Ctrl Pts',(1.29227634889257,2.08205957842058,32.0713891605866));
#7072=CARTESIAN_POINT('Ctrl Pts',(1.22249536750309,2.12537068862452,32.0756685903126));
#7073=CARTESIAN_POINT('Ctrl Pts',(1.15064060594837,2.165104138692,32.0799480200387));
#7074=CARTESIAN_POINT('Ctrl Pts',(1.07712117087287,2.20108160531532,32.0842274497648));
#7075=CARTESIAN_POINT('Ctrl Pts',(1.00443886592718,2.23664941398529,32.0884581517012));
#7076=CARTESIAN_POINT('Ctrl Pts',(0.92985624491494,2.26868015883065,32.0926888536377));
#7077=CARTESIAN_POINT('Ctrl Pts',(0.853751750610977,2.29696717397718,32.0969195555742));
#7078=CARTESIAN_POINT('Ctrl Pts',(0.777756597525942,2.32521354846583,32.1011441791561));
#7079=CARTESIAN_POINT('Ctrl Pts',(0.700244345908673,2.34972671501686,32.1053688027379));
#7080=CARTESIAN_POINT('Ctrl Pts',(0.621616440924413,2.37034665194196,32.1095934263197));
#7081=CARTESIAN_POINT('Ctrl Pts',(0.542679071972787,2.39104774488271,32.113834677189));
#7082=CARTESIAN_POINT('Ctrl Pts',(0.462617675086656,2.40782468790357,32.1180759280582));
#7083=CARTESIAN_POINT('Ctrl Pts',(0.381857085610222,2.42056510265047,32.1223171789275));
#7084=CARTESIAN_POINT('Ctrl Pts',(0.301558287351308,2.433232667364,32.1265341782104));
#7085=CARTESIAN_POINT('Ctrl Pts',(0.220568734805544,2.44190966729532,32.1307511774934));
#7086=CARTESIAN_POINT('Ctrl Pts',(0.139317688964832,2.44653649707939,32.1349681767764));
#7087=CARTESIAN_POINT('Ctrl Pts',(0.0580935796242474,2.45116179296812,32.1391837780318));
#7088=CARTESIAN_POINT('Ctrl Pts',(-0.0233913869178665,2.45173955870469,
32.1433993792872));
#7089=CARTESIAN_POINT('Ctrl Pts',(-0.104703613013471,2.4482621190187,32.1476149805426));
#7090=CARTESIAN_POINT('Ctrl Pts',(-0.18601381015834,2.44478476610384,32.1518304766078));
#7091=CARTESIAN_POINT('Ctrl Pts',(-0.267150810837261,2.4372524299078,32.1560459726731));
#7092=CARTESIAN_POINT('Ctrl Pts',(-0.347683249838471,2.42570950605833,32.1602614687383));
#7093=CARTESIAN_POINT('Ctrl Pts',(-0.429069037475522,2.41404426953036,32.1645216336086));
#7094=CARTESIAN_POINT('Ctrl Pts',(-0.509836893019328,2.39828299700287,32.1687817984789));
#7095=CARTESIAN_POINT('Ctrl Pts',(-0.589551077060534,2.37852470610182,32.1730419633491));
#7096=CARTESIAN_POINT('Ctrl Pts',(-0.668544311532325,2.35894511277497,32.177263598514));
#7097=CARTESIAN_POINT('Ctrl Pts',(-0.746502424638695,2.33544070461732,32.1814852336788));
#7098=CARTESIAN_POINT('Ctrl Pts',(-0.823017449620409,2.30815782121161,32.1857068688437));
#7099=CARTESIAN_POINT('Ctrl Pts',(-0.900579972049529,2.28050143272331,32.1899862985667));
#7100=CARTESIAN_POINT('Ctrl Pts',(-0.976659138231037,2.24896251977049,32.1942657282896));
#7101=CARTESIAN_POINT('Ctrl Pts',(-1.0508535298998,2.21374278286732,32.1985451580126));
#7102=CARTESIAN_POINT('Ctrl Pts',(-1.12504792156853,2.17852304596416,32.2028245877356));
#7103=CARTESIAN_POINT('Ctrl Pts',(-1.19735713771539,2.13962277520903,32.2071040174586));
#7104=CARTESIAN_POINT('Ctrl Pts',(-1.26740975649452,2.09728938373856,32.2113834471815));
#7105=CARTESIAN_POINT('Ctrl Pts',(-1.33666472066413,2.05543802171156,32.2156141491495));
#7106=CARTESIAN_POINT('Ctrl Pts',(-1.40397472540036,2.01007394635426,32.2198448511175));
#7107=CARTESIAN_POINT('Ctrl Pts',(-1.46896112141037,1.96140344493039,32.2240755530855));
#7108=CARTESIAN_POINT('Ctrl Pts',(-1.53385414985265,1.91280286962362,32.228300176699));
#7109=CARTESIAN_POINT('Ctrl Pts',(-1.59642983070718,1.86090557927122,32.2325248003124));
#7110=CARTESIAN_POINT('Ctrl Pts',(-1.65633627736508,1.80596245428425,32.2367494239259));
#7111=CARTESIAN_POINT('Ctrl Pts',(-1.71647850345055,1.75080308448089,32.2409906747873));
#7112=CARTESIAN_POINT('Ctrl Pts',(-1.7739300330097,1.69257409850609,32.2452319256486));
#7113=CARTESIAN_POINT('Ctrl Pts',(-1.82836637221471,1.63157183689668,32.24947317651));
#7114=CARTESIAN_POINT('Ctrl Pts',(-1.8824914434803,1.57091838728581,32.2536901758247));
#7115=CARTESIAN_POINT('Ctrl Pts',(-1.93363539988959,1.50752364173452,32.2579071751395));
#7116=CARTESIAN_POINT('Ctrl Pts',(-1.98151572079514,1.44171623360553,32.2621241744542));
#7117=CARTESIAN_POINT('Ctrl Pts',(-2.02938016832626,1.3759306420728,32.2663397757414));
#7118=CARTESIAN_POINT('Ctrl Pts',(-2.07398285556091,1.30773435208733,32.2705553770286));
#7119=CARTESIAN_POINT('Ctrl Pts',(-2.11508257455249,1.23748775865638,32.2747709783158));
#7120=CARTESIAN_POINT('Ctrl Pts',(-2.15618126799898,1.16724291806102,32.2789864744127));
#7121=CARTESIAN_POINT('Ctrl Pts',(-2.19377693307522,1.09494827769197,32.2832019705097));
#7122=CARTESIAN_POINT('Ctrl Pts',(-2.22767334950147,1.02099054741995,32.2874174666066));
#7123=CARTESIAN_POINT('Ctrl Pts',(-2.26192894312335,0.946249137545359,32.2916776314392));
#7124=CARTESIAN_POINT('Ctrl Pts',(-2.29240620797663,0.869809616353677,32.2959377962719));
#7125=CARTESIAN_POINT('Ctrl Pts',(-2.3189524794021,0.792091944331508,32.3001979611045));
#7126=CARTESIAN_POINT('Ctrl Pts',(-2.34525866195077,0.71507716381088,32.3044195963006));
#7127=CARTESIAN_POINT('Ctrl Pts',(-2.36770459988061,0.636807728104529,32.3086412314967));
#7128=CARTESIAN_POINT('Ctrl Pts',(-2.38619245125746,0.557705868322988,32.3128628666928));
#7129=CARTESIAN_POINT('Ctrl Pts',(-2.40493340249762,0.477521099041088,32.3171422963437));
#7130=CARTESIAN_POINT('Ctrl Pts',(-2.41960698558035,0.396481427974036,32.3214217259946));
#7131=CARTESIAN_POINT('Ctrl Pts',(-2.430165449126,0.315033553568883,32.3257011556455));
#7132=CARTESIAN_POINT('Ctrl Pts',(-2.44072391267165,0.233585679163708,32.3299805852964));
#7133=CARTESIAN_POINT('Ctrl Pts',(-2.44716728347151,0.15173009563451,32.3342600149473));
#7134=CARTESIAN_POINT('Ctrl Pts',(-2.44950248378864,0.0699130310692556,
32.3385394445982));
#7135=CARTESIAN_POINT('Ctrl Pts',(-2.45016331335893,0.0467599271480851,
32.3397504643281));
#7136=CARTESIAN_POINT('Ctrl Pts',(-2.45049588145719,0.0235974094165099,
32.340961484058));
#7137=CARTESIAN_POINT('Ctrl Pts',(-2.45049996198422,0.000431642579436891,
32.3421725037879));
#7138=CARTESIAN_POINT('',(-2.45049918758584,0.00199540500337376,33.1421724763606));
#7139=CARTESIAN_POINT('Ctrl Pts',(-2.4504999619844,0.000431641585035285,
32.3421725038399));
#7140=CARTESIAN_POINT('Ctrl Pts',(-2.45051414927913,-0.0801119538513814,
32.3463830220531));
#7141=CARTESIAN_POINT('Ctrl Pts',(-2.44655306968252,-0.160813628721216,
32.3505935402663));
#7142=CARTESIAN_POINT('Ctrl Pts',(-2.43859602483964,-0.241246093515107,
32.3548040584794));
#7143=CARTESIAN_POINT('Ctrl Pts',(-2.43065032934404,-0.321563835319083,
32.3590085711171));
#7144=CARTESIAN_POINT('Ctrl Pts',(-2.41872003130953,-0.401612665834839,
32.3632130837549));
#7145=CARTESIAN_POINT('Ctrl Pts',(-2.40283644220969,-0.480964948815475,
32.3674175963925));
#7146=CARTESIAN_POINT('Ctrl Pts',(-2.38697086816974,-0.56022723097068,32.3716173403003));
#7147=CARTESIAN_POINT('Ctrl Pts',(-2.3671610036448,-0.638794076840536,32.3758170842081));
#7148=CARTESIAN_POINT('Ctrl Pts',(-2.34348982424493,-0.716244157854338,
32.3800168281158));
#7149=CARTESIAN_POINT('Ctrl Pts',(-2.31983319025196,-0.793646647536738,
32.3842139913755));
#7150=CARTESIAN_POINT('Ctrl Pts',(-2.29232008705754,-0.869933285910213,
32.3884111546352));
#7151=CARTESIAN_POINT('Ctrl Pts',(-2.26108403109816,-0.944695323537124,
32.3926083178948));
#7152=CARTESIAN_POINT('Ctrl Pts',(-2.22985735715304,-1.0194349057521,32.3968042205009));
#7153=CARTESIAN_POINT('Ctrl Pts',(-2.19491013178432,-1.09265036308669,32.401000123107));
#7154=CARTESIAN_POINT('Ctrl Pts',(-2.15642442956955,-1.16395185877923,32.4051960257131));
#7155=CARTESIAN_POINT('Ctrl Pts',(-2.1179381978553,-1.23525433546218,32.4093919860478));
#7156=CARTESIAN_POINT('Ctrl Pts',(-2.07591361738323,-1.30464238545099,32.4135879463826));
#7157=CARTESIAN_POINT('Ctrl Pts',(-2.03057852695273,-1.37175110565965,32.4177839067173));
#7158=CARTESIAN_POINT('Ctrl Pts',(-1.98519789814841,-1.43892723550527,32.4219840818272));
#7159=CARTESIAN_POINT('Ctrl Pts',(-1.93650038245503,-1.50381907315001,32.426184256937));
#7160=CARTESIAN_POINT('Ctrl Pts',(-1.88475658813207,-1.56609158528253,32.4303844320469));
#7161=CARTESIAN_POINT('Ctrl Pts',(-1.83298640188451,-1.62839585951265,32.4345867494562));
#7162=CARTESIAN_POINT('Ctrl Pts',(-1.77816716179821,-1.68807780206639,32.4387890668656));
#7163=CARTESIAN_POINT('Ctrl Pts',(-1.72060740200968,-1.74483822119688,32.4429913842749));
#7164=CARTESIAN_POINT('Ctrl Pts',(-1.66294636868909,-1.80169850745935,32.4472010954526));
#7165=CARTESIAN_POINT('Ctrl Pts',(-1.60253553608518,-1.85562669030327,32.4514108066302));
#7166=CARTESIAN_POINT('Ctrl Pts',(-1.53971740739335,-1.90636317509805,32.4556205178079));
#7167=CARTESIAN_POINT('Ctrl Pts',(-1.48960408142772,-1.94683833814125,32.4589788258769));
#7168=CARTESIAN_POINT('Ctrl Pts',(-1.4379594376405,-1.98528303520078,32.4623371339459));
#7169=CARTESIAN_POINT('Ctrl Pts',(-1.3849695681631,-2.02158589856135,32.4656954420149));
#7170=CARTESIAN_POINT('Ctrl Pts',(-1.31821442288667,-2.06731922346827,32.4699261439442));
#7171=CARTESIAN_POINT('Ctrl Pts',(-1.24906605095292,-2.10982850004489,32.4741568458735));
#7172=CARTESIAN_POINT('Ctrl Pts',(-1.17786891945138,-2.14885435955777,32.4783875478028));
#7173=CARTESIAN_POINT('Ctrl Pts',(-1.10677407864559,-2.1878241496443,32.482612171377));
#7174=CARTESIAN_POINT('Ctrl Pts',(-1.03363672858628,-2.22332024065947,32.4868367949513));
#7175=CARTESIAN_POINT('Ctrl Pts',(-0.958830860651012,-2.2551260786624,32.4910614185255));
#7176=CARTESIAN_POINT('Ctrl Pts',(-0.883730571366394,-2.2870570982587,32.4953026693966));
#7177=CARTESIAN_POINT('Ctrl Pts',(-0.806948993604187,-2.31526848609442,
32.4995439202677));
#7178=CARTESIAN_POINT('Ctrl Pts',(-0.728890171634071,-2.33958743536019,
32.5037851711388));
#7179=CARTESIAN_POINT('Ctrl Pts',(-0.651277692293025,-2.36376732816215,
32.5080021704132));
#7180=CARTESIAN_POINT('Ctrl Pts',(-0.572402984222,-2.38409903603608,32.5122191696877));
#7181=CARTESIAN_POINT('Ctrl Pts',(-0.492682124559706,-2.40046132527465,
32.5164361689621));
#7182=CARTESIAN_POINT('Ctrl Pts',(-0.41298769411338,-2.41681819005496,32.5206517702087));
#7183=CARTESIAN_POINT('Ctrl Pts',(-0.3324481243396,-2.42920815602413,32.5248673714553));
#7184=CARTESIAN_POINT('Ctrl Pts',(-0.251491314947697,-2.43756074150079,
32.5290829727019));
#7185=CARTESIAN_POINT('Ctrl Pts',(-0.17053652564392,-2.44591311855819,32.533298468758));
#7186=CARTESIAN_POINT('Ctrl Pts',(-0.089164980138353,-2.45022826877663,
32.5375139648141));
#7187=CARTESIAN_POINT('Ctrl Pts',(-0.00780992149994874,-2.45048755457484,
32.5417294608702));
#7188=CARTESIAN_POINT('Ctrl Pts',(0.07440720289556,-2.45074958785319,32.5459896257503));
#7189=CARTESIAN_POINT('Ctrl Pts',(0.156607004528232,-2.44686927263466,32.5502497906304));
#7190=CARTESIAN_POINT('Ctrl Pts',(0.238343990183245,-2.43888138135981,32.5545099555106));
#7191=CARTESIAN_POINT('Ctrl Pts',(0.319341731307874,-2.43096573406223,32.5587315906656));
#7192=CARTESIAN_POINT('Ctrl Pts',(0.399884538289744,-2.41901664127913,32.5629532258207));
#7193=CARTESIAN_POINT('Ctrl Pts',(0.479547533490022,-2.40311972509146,32.5671748609757));
#7194=CARTESIAN_POINT('Ctrl Pts',(0.560301122686974,-2.3870051786061,32.5714542907184));
#7195=CARTESIAN_POINT('Ctrl Pts',(0.640150148704368,-2.3668340192763,32.5757337204611));
#7196=CARTESIAN_POINT('Ctrl Pts',(0.718668183780573,-2.34274759451835,32.5800131502037));
#7197=CARTESIAN_POINT('Ctrl Pts',(0.797186218856778,-2.3186611697604,32.5842925799464));
#7198=CARTESIAN_POINT('Ctrl Pts',(0.874372824147898,-2.29065970844424,32.5885720096891));
#7199=CARTESIAN_POINT('Ctrl Pts',(0.949824621131082,-2.25893413783873,32.5928514394317));
#7200=CARTESIAN_POINT('Ctrl Pts',(1.02441728808141,-2.22756980966356,32.5970821415528));
#7201=CARTESIAN_POINT('Ctrl Pts',(1.09759503317657,-2.19244781989971,32.6013128436738));
#7202=CARTESIAN_POINT('Ctrl Pts',(1.16895329161688,-2.15371735657631,32.6055435457948));
#7203=CARTESIAN_POINT('Ctrl Pts',(1.2402090278906,-2.11504253826303,32.609768169562));
#7204=CARTESIAN_POINT('Ctrl Pts',(1.30965006399002,-2.07276976282349,32.6139927933291));
#7205=CARTESIAN_POINT('Ctrl Pts',(1.37689184717846,-2.02709622148863,32.6182174170963));
#7206=CARTESIAN_POINT('Ctrl Pts',(1.44439827710164,-1.98124292059051,32.6224586679193));
#7207=CARTESIAN_POINT('Ctrl Pts',(1.50968766811608,-1.93196221120455,32.6266999187423));
#7208=CARTESIAN_POINT('Ctrl Pts',(1.57239597728727,-1.87950023692758,32.6309411695653));
#7209=CARTESIAN_POINT('Ctrl Pts',(1.63474572209043,-1.82733823876064,32.635158169034));
#7210=CARTESIAN_POINT('Ctrl Pts',(1.69454346178162,-1.77203155916156,32.6393751685028));
#7211=CARTESIAN_POINT('Ctrl Pts',(1.75146199910057,-1.71386438078006,32.6435921679715));
#7212=CARTESIAN_POINT('Ctrl Pts',(1.8083616666763,-1.65571648609368,32.6478077694125));
#7213=CARTESIAN_POINT('Ctrl Pts',(1.86238370238937,-1.59471030795587,32.6520233708534));
#7214=CARTESIAN_POINT('Ctrl Pts',(1.91323717824831,-1.53116744667866,32.6562389722944));
#7215=CARTESIAN_POINT('Ctrl Pts',(1.96408938517551,-1.46762617096768,32.6604544685447));
#7216=CARTESIAN_POINT('Ctrl Pts',(2.01177289970693,-1.40154870174325,32.664669964795));
#7217=CARTESIAN_POINT('Ctrl Pts',(2.05603748921055,-1.33328920079658,32.6688854610452));
#7218=CARTESIAN_POINT('Ctrl Pts',(2.10077111682289,-1.26430640595777,32.6731456256955));
#7219=CARTESIAN_POINT('Ctrl Pts',(2.14201265539818,-1.1930954591219,32.6774057903458));
#7220=CARTESIAN_POINT('Ctrl Pts',(2.1795501448686,-1.12004973818276,32.681665954996));
#7221=CARTESIAN_POINT('Ctrl Pts',(2.216748141986,-1.04766464916198,32.6858875903429));
#7222=CARTESIAN_POINT('Ctrl Pts',(2.25030868242107,-0.973478294132603,32.6901092256897));
#7223=CARTESIAN_POINT('Ctrl Pts',(2.28007371977505,-0.897894249002155,32.6943308610366));
#7224=CARTESIAN_POINT('Ctrl Pts',(2.31024623884924,-0.821275462461399,32.6986102903386));
#7225=CARTESIAN_POINT('Ctrl Pts',(2.33651838975215,-0.743220896275271,32.7028897196405));
#7226=CARTESIAN_POINT('Ctrl Pts',(2.35877813836951,-0.664165599794256,32.7071691489425));
#7227=CARTESIAN_POINT('Ctrl Pts',(2.38103788698687,-0.585110303313242,32.7114485782445));
#7228=CARTESIAN_POINT('Ctrl Pts',(2.39928518814752,-0.505054769411128,32.7157280075465));
#7229=CARTESIAN_POINT('Ctrl Pts',(2.41346217146957,-0.424441511736742,32.7200074368484));
#7230=CARTESIAN_POINT('Ctrl Pts',(2.42747772865952,-0.344746156417734,32.7242381384554));
#7231=CARTESIAN_POINT('Ctrl Pts',(2.43756794910877,-0.264205964768421,32.7284688400623));
#7232=CARTESIAN_POINT('Ctrl Pts',(2.44363922756559,-0.183241849757813,32.7326995416692));
#7233=CARTESIAN_POINT('Ctrl Pts',(2.44970178326558,-0.102394057905686,32.7369241649219));
#7234=CARTESIAN_POINT('Ctrl Pts',(2.45175683020018,-0.0211240121449797,
32.7411487881746));
#7235=CARTESIAN_POINT('Ctrl Pts',(2.4497619569373,0.0601382103387006,32.7453734114273));
#7236=CARTESIAN_POINT('Ctrl Pts',(2.44775923205074,0.141720272885431,32.7496146623788));
#7237=CARTESIAN_POINT('Ctrl Pts',(2.44167455622069,0.22329398305791,32.7538559133304));
#7238=CARTESIAN_POINT('Ctrl Pts',(2.43151777934252,0.304420003845395,32.758097164282));
#7239=CARTESIAN_POINT('Ctrl Pts',(2.42141908016349,0.385082136070123,32.7623141632391));
#7240=CARTESIAN_POINT('Ctrl Pts',(2.40729478146787,0.465301218805409,32.7665311621962));
#7241=CARTESIAN_POINT('Ctrl Pts',(2.38920666345568,0.544648298720361,32.7707481611533));
#7242=CARTESIAN_POINT('Ctrl Pts',(2.37112454204265,0.623969073376095,32.7749637620848));
#7243=CARTESIAN_POINT('Ctrl Pts',(2.34908131415745,0.702417966221634,32.7791793630162));
#7244=CARTESIAN_POINT('Ctrl Pts',(2.32318985579329,0.779576259219809,32.7833949639477));
#7245=CARTESIAN_POINT('Ctrl Pts',(2.2972990434737,0.856732626961591,32.7876104596914));
#7246=CARTESIAN_POINT('Ctrl Pts',(2.26756034056709,0.932598018329473,32.7918259554351));
#7247=CARTESIAN_POINT('Ctrl Pts',(2.23413603232489,1.00677030104567,32.7960414511787));
#7248=CARTESIAN_POINT('Ctrl Pts',(2.20035754329814,1.0817285505826,32.8003016164359));
#7249=CARTESIAN_POINT('Ctrl Pts',(2.1628150591435,1.15495714743976,32.8045617816931));
#7250=CARTESIAN_POINT('Ctrl Pts',(2.12172455773923,1.22606490492398,32.8088219469503));
#7251=CARTESIAN_POINT('Ctrl Pts',(2.08100569301125,1.29652953930807,32.8130435818026));
#7252=CARTESIAN_POINT('Ctrl Pts',(2.03680303897295,1.3649111818143,32.8172652166549));
#7253=CARTESIAN_POINT('Ctrl Pts',(1.98937033689326,1.43085845305858,32.8214868515072));
#7254=CARTESIAN_POINT('Ctrl Pts',(1.94128826509763,1.49770856472556,32.8257662819669));
#7255=CARTESIAN_POINT('Ctrl Pts',(1.88988734343297,1.56205675921975,32.8300457124266));
#7256=CARTESIAN_POINT('Ctrl Pts',(1.83547268665345,1.62357330187127,32.8343251428862));
#7257=CARTESIAN_POINT('Ctrl Pts',(1.78105802987395,1.68508984452277,32.8386045733459));
#7258=CARTESIAN_POINT('Ctrl Pts',(1.72363002791167,1.74377443050535,32.8428840038055));
#7259=CARTESIAN_POINT('Ctrl Pts',(1.66352939611642,1.79933882252802,32.8471634342652));
#7260=CARTESIAN_POINT('Ctrl Pts',(1.60411311074725,1.8542705208175,32.8513941362364));
#7261=CARTESIAN_POINT('Ctrl Pts',(1.54186129872075,1.90635936664191,32.8556248382076));
#7262=CARTESIAN_POINT('Ctrl Pts',(1.47707716683848,1.9552987733859,32.8598555401789));
#7263=CARTESIAN_POINT('Ctrl Pts',(1.41238611197482,2.00416786763299,32.8640801637924));
#7264=CARTESIAN_POINT('Ctrl Pts',(1.34517033094913,2.04989623151562,32.868304787406));
#7265=CARTESIAN_POINT('Ctrl Pts',(1.27576845238626,2.0922153583931,32.8725294110195));
#7266=CARTESIAN_POINT('Ctrl Pts',(1.2060934223406,2.13470104462742,32.8767706618804));
#7267=CARTESIAN_POINT('Ctrl Pts',(1.13421539824392,2.17375027803713,32.8810119127414));
#7268=CARTESIAN_POINT('Ctrl Pts',(1.06050908877006,2.20913347777722,32.8852531636023));
#7269=CARTESIAN_POINT('Ctrl Pts',(0.987224233388338,2.24431435570214,32.8894701629094));
#7270=CARTESIAN_POINT('Ctrl Pts',(0.91213236770277,2.27587080780408,32.8936871622165));
#7271=CARTESIAN_POINT('Ctrl Pts',(0.8356275860296,2.3036225358045,32.8979041615237));
#7272=CARTESIAN_POINT('Ctrl Pts',(0.759148167418059,2.3313650634808,32.9021197628003));
#7273=CARTESIAN_POINT('Ctrl Pts',(0.681257199848004,2.35530521342506,32.906335364077));
#7274=CARTESIAN_POINT('Ctrl Pts',(0.602367836105354,2.37531118803953,32.9105509653537));
#7275=CARTESIAN_POINT('Ctrl Pts',(0.523480440910551,2.39531666343945,32.9147664614373));
#7276=CARTESIAN_POINT('Ctrl Pts',(0.443595150134574,2.41138804543011,32.9189819575209));
#7277=CARTESIAN_POINT('Ctrl Pts',(0.363137922722365,2.42344405734502,32.9231974536046));
#7278=CARTESIAN_POINT('Ctrl Pts',(0.281828144578112,2.43562781865068,32.9274576184443));
#7279=CARTESIAN_POINT('Ctrl Pts',(0.199934713508689,2.44371051915757,32.9317177832841));
#7280=CARTESIAN_POINT('Ctrl Pts',(0.117903455469611,2.44766195075797,32.9359779481239));
#7281=CARTESIAN_POINT('Ctrl Pts',(0.0366141022405083,2.4515776449312,32.9401995833));
#7282=CARTESIAN_POINT('Ctrl Pts',(-0.0448101248036766,2.45143655996908,
32.9444212184761));
#7283=CARTESIAN_POINT('Ctrl Pts',(-0.125936422214181,2.44726178974786,32.9486428536521));
#7284=CARTESIAN_POINT('Ctrl Pts',(-0.208173344593542,2.44302986661575,32.9529222833238));
#7285=CARTESIAN_POINT('Ctrl Pts',(-0.290103626129848,2.4346530294107,32.9572017129954));
#7286=CARTESIAN_POINT('Ctrl Pts',(-0.371284847448981,2.4222092832897,32.961481142667));
#7287=CARTESIAN_POINT('Ctrl Pts',(-0.452466068768091,2.4097655371687,32.9657605723387));
#7288=CARTESIAN_POINT('Ctrl Pts',(-0.532897762471851,2.39325504493315,32.9700400020103));
#7289=CARTESIAN_POINT('Ctrl Pts',(-0.612153123806261,2.37280821033101,32.9743194316819));
#7290=CARTESIAN_POINT('Ctrl Pts',(-0.690506065125478,2.35259418815292,32.97855013477));
#7291=CARTESIAN_POINT('Ctrl Pts',(-0.768004043464895,2.32845701957416,32.982780837858));
#7292=CARTESIAN_POINT('Ctrl Pts',(-0.844225133903018,2.30048563857426,32.987011540946));
#7293=CARTESIAN_POINT('Ctrl Pts',(-0.920336715732164,2.27255444470639,32.9912361656848));
#7294=CARTESIAN_POINT('Ctrl Pts',(-0.995174620260639,2.2408001378618,32.9954607904235));
#7295=CARTESIAN_POINT('Ctrl Pts',(-1.06832976081949,2.20536205012859,32.9996854151623));
#7296=CARTESIAN_POINT('Ctrl Pts',(-1.14177280051215,2.16978449721652,33.003926665743));
#7297=CARTESIAN_POINT('Ctrl Pts',(-1.21351934342128,2.13049422503592,33.0081679163237));
#7298=CARTESIAN_POINT('Ctrl Pts',(-1.28317349627679,2.08768197493124,33.0124091669044));
#7299=CARTESIAN_POINT('Ctrl Pts',(-1.35242938860447,2.04511451180084,33.0166261673488));
#7300=CARTESIAN_POINT('Ctrl Pts',(-1.41961635302222,1.99906548255506,33.0208431677933));
#7301=CARTESIAN_POINT('Ctrl Pts',(-1.48436943494468,1.94976860950268,33.0250601682378));
#7302=CARTESIAN_POINT('Ctrl Pts',(-1.54910104979629,1.90048807944796,33.0292757706538));
#7303=CARTESIAN_POINT('Ctrl Pts',(-1.61140001475318,1.84796212527597,33.0334913730699));
#7304=CARTESIAN_POINT('Ctrl Pts',(-1.67093183406871,1.79246675168489,33.0377069754859));
#7305=CARTESIAN_POINT('Ctrl Pts',(-1.73046216787779,1.73697276287822,33.0419224727095));
#7306=CARTESIAN_POINT('Ctrl Pts',(-1.78722515389434,1.67850981988038,33.046137969933));
#7307=CARTESIAN_POINT('Ctrl Pts',(-1.84092183882263,1.61739204689089,33.0503534671565));
#7308=CARTESIAN_POINT('Ctrl Pts',(-1.89518747934265,1.55562668646202,33.0546136306517));
#7309=CARTESIAN_POINT('Ctrl Pts',(-1.94632112062992,1.49115025466911,33.0588737941468));
#7310=CARTESIAN_POINT('Ctrl Pts',(-1.99405598988234,1.42432122753765,33.063133957642));
#7311=CARTESIAN_POINT('Ctrl Pts',(-2.04135916434991,1.35809657500573,33.0673555939475));
#7312=CARTESIAN_POINT('Ctrl Pts',(-2.08532459180849,1.28956213693925,33.071577230253));
#7313=CARTESIAN_POINT('Ctrl Pts',(-2.12573736355962,1.21909429953822,33.0757988665584));
#7314=CARTESIAN_POINT('Ctrl Pts',(-2.16670335345106,1.14766181447089,33.0800782936485));
#7315=CARTESIAN_POINT('Ctrl Pts',(-2.20401846113595,1.07424303692224,33.0843577207385));
#7316=CARTESIAN_POINT('Ctrl Pts',(-2.23750873923386,0.999252166298438,33.0886371478286));
#7317=CARTESIAN_POINT('Ctrl Pts',(-2.27099901733176,0.924261295674634,33.0929165749186));
#7318=CARTESIAN_POINT('Ctrl Pts',(-2.30066434966464,0.847698813084396,33.0971960020087));
#7319=CARTESIAN_POINT('Ctrl Pts',(-2.32638329711352,0.76999415901112,33.1014754290987));
#7320=CARTESIAN_POINT('Ctrl Pts',(-2.35666864530179,0.678493038713086,33.1065146687381));
#7321=CARTESIAN_POINT('Ctrl Pts',(-2.3815763775295,0.585128820235907,33.1115539083775));
#7322=CARTESIAN_POINT('Ctrl Pts',(-2.40091147374684,0.490483786919389,33.1165931480169));
#7323=CARTESIAN_POINT('Ctrl Pts',(-2.4200315925657,0.396891065047913,33.1215763588362));
#7324=CARTESIAN_POINT('Ctrl Pts',(-2.43370224837572,0.302045925225219,33.1265595696555));
#7325=CARTESIAN_POINT('Ctrl Pts',(-2.44178104468291,0.206532273088859,33.1315427804748));
#7326=CARTESIAN_POINT('Ctrl Pts',(-2.44752534295315,0.138618825851275,33.1350860124367));
#7327=CARTESIAN_POINT('Ctrl Pts',(-2.45044351293495,0.0703678339286369,
33.1386292443987));
#7328=CARTESIAN_POINT('Ctrl Pts',(-2.45049918758584,0.00199540500337376,
33.1421724763606));
#7329=CARTESIAN_POINT('',(-2.44727084717605,-0.00140258346811789,33.942172503788));
#7330=CARTESIAN_POINT('Ctrl Pts',(-2.44847586273047,0.00199322861988113,
33.142172503788));
#7331=CARTESIAN_POINT('Ctrl Pts',(-2.44423584572099,-0.553673306700436,
33.1709921446971));
#7332=CARTESIAN_POINT('Ctrl Pts',(-1.98117856145162,-1.93295879325365,33.2421971180786));
#7333=CARTESIAN_POINT('Ctrl Pts',(0.309238185493155,-2.88090186856504,33.355787423932));
#7334=CARTESIAN_POINT('Ctrl Pts',(2.58956571189241,-1.29976110413427,33.4829434213489));
#7335=CARTESIAN_POINT('Ctrl Pts',(2.49480438216511,1.47349276746318,33.6100994187657));
#7336=CARTESIAN_POINT('Ctrl Pts',(0.111868610958372,2.89528823059717,33.7372554161823));
#7337=CARTESIAN_POINT('Ctrl Pts',(-2.051828672412,1.8213500783052,33.8479464445231));
#7338=CARTESIAN_POINT('Ctrl Pts',(-2.44467637437558,0.498983042526859,33.9162521403917));
#7339=CARTESIAN_POINT('Ctrl Pts',(-2.44727084717605,-0.00140258346811789,
33.942172503788));
#7340=CARTESIAN_POINT('',(-2.45356477742091,-0.00152987545416492,34.7421725037879));
#7341=CARTESIAN_POINT('Ctrl Pts',(-2.44727084717605,-0.00140258346811789,
33.942172503788));
#7342=CARTESIAN_POINT('Ctrl Pts',(-2.44891889175687,-0.31925437173569,33.9586374728639));
#7343=CARTESIAN_POINT('Ctrl Pts',(-2.24355252467318,-1.45329455082822,34.0174877744123));
#7344=CARTESIAN_POINT('Ctrl Pts',(-0.530612517065195,-2.84843073781086,
34.1187234084324));
#7345=CARTESIAN_POINT('Ctrl Pts',(2.10758733248769,-1.98834033015572,34.2458794058493));
#7346=CARTESIAN_POINT('Ctrl Pts',(2.81273209537355,0.695553694092942,34.373035403266));
#7347=CARTESIAN_POINT('Ctrl Pts',(0.938155042953724,2.74122592529684,34.5001914006828));
#7348=CARTESIAN_POINT('Ctrl Pts',(-1.70855734209424,2.28836542993453,34.6232371008568));
#7349=CARTESIAN_POINT('Ctrl Pts',(-2.44866265110221,0.732444988893918,34.7038974685585));
#7350=CARTESIAN_POINT('Ctrl Pts',(-2.45356477742091,-0.00152987545416492,
34.7421725037879));
#7351=CARTESIAN_POINT('',(1.07686354780633,-2.20575423999072,34.9999542666628));
#7352=CARTESIAN_POINT('Ctrl Pts',(-2.45356477742091,-0.00152987545416492,
34.7421725037879));
#7353=CARTESIAN_POINT('Ctrl Pts',(-2.4540912092366,-0.0803503087494975,
34.7462828010307));
#7354=CARTESIAN_POINT('Ctrl Pts',(-2.41487118212295,-0.97139961274513,34.7927784307463));
#7355=CARTESIAN_POINT('Ctrl Pts',(-1.3621803363065,-2.52198142046407,34.8787056850368));
#7356=CARTESIAN_POINT('Ctrl Pts',(0.395824670058481,-2.53385348501788,34.9605226420862));
#7357=CARTESIAN_POINT('Ctrl Pts',(1.07686354780633,-2.20575423999072,34.9999542666628));
#7358=CARTESIAN_POINT('',(-1.07508846035141,-2.20207516956602,35.));
#7359=CARTESIAN_POINT('Origin',(0.,0.,35.));
#7360=CARTESIAN_POINT('',(-2.45049860417889,-0.0026155147360495,34.8578274961857));
#7361=CARTESIAN_POINT('Ctrl Pts',(-1.07508846035141,-2.20207516956602,35.));
#7362=CARTESIAN_POINT('Ctrl Pts',(-1.14997613952614,-2.16551380199059,34.9956699954726));
#7363=CARTESIAN_POINT('Ctrl Pts',(-1.22305004349785,-2.12510242184625,34.9913399909452));
#7364=CARTESIAN_POINT('Ctrl Pts',(-1.29390617536955,-2.08104710646841,34.9870099864178));
#7365=CARTESIAN_POINT('Ctrl Pts',(-1.36471943359506,-2.03701844809195,34.9826826018907));
#7366=CARTESIAN_POINT('Ctrl Pts',(-1.43331722252973,-1.9893504704842,34.9783552173635));
#7367=CARTESIAN_POINT('Ctrl Pts',(-1.49932159809749,-1.93829435212467,34.9740278328364));
#7368=CARTESIAN_POINT('Ctrl Pts',(-1.56531940167207,-1.88724331737451,34.9697008791828));
#7369=CARTESIAN_POINT('Ctrl Pts',(-1.62872395639475,-1.83280506987026,34.9653739255293));
#7370=CARTESIAN_POINT('Ctrl Pts',(-1.68918825280508,-1.77527273864759,34.9610469718757));
#7371=CARTESIAN_POINT('Ctrl Pts',(-1.74965116688525,-1.71774172272471,34.9567201171446));
#7372=CARTESIAN_POINT('Ctrl Pts',(-1.80717364164387,-1.65711706240731,34.9523932624135));
#7373=CARTESIAN_POINT('Ctrl Pts',(-1.86144452495553,-1.59372975454218,34.9480664076824));
#7374=CARTESIAN_POINT('Ctrl Pts',(-1.9157272829466,-1.53032857728865,34.9437386062187));
#7375=CARTESIAN_POINT('Ctrl Pts',(-1.96675675199689,-1.46416387957714,34.9394108047551));
#7376=CARTESIAN_POINT('Ctrl Pts',(-2.01426185774394,-1.39560002093649,34.9350830032914));
#7377=CARTESIAN_POINT('Ctrl Pts',(-2.0617888418391,-1.32700458539598,34.9307532086705));
#7378=CARTESIAN_POINT('Ctrl Pts',(-2.10578798686745,-1.25600814742925,34.9264234140496));
#7379=CARTESIAN_POINT('Ctrl Pts',(-2.14603194121717,-1.18300344770235,34.9220936194286));
#7380=CARTESIAN_POINT('Ctrl Pts',(-2.18633590536483,-1.10988988697137,34.9177573684317));
#7381=CARTESIAN_POINT('Ctrl Pts',(-2.22287328548544,-1.03476246431391,34.9134211174348));
#7382=CARTESIAN_POINT('Ctrl Pts',(-2.25546306018371,-0.95803790851235,34.9090848664379));
#7383=CARTESIAN_POINT('Ctrl Pts',(-2.28807781659817,-0.881254539445122,
34.9047452914845));
#7384=CARTESIAN_POINT('Ctrl Pts',(-2.31673878767929,-0.802872004799493,
34.9004057165312));
#7385=CARTESIAN_POINT('Ctrl Pts',(-2.34131425464778,-0.723324139638024,
34.8960661415778));
#7386=CARTESIAN_POINT('Ctrl Pts',(-2.36593829093927,-0.643619061351729,
34.8917179901763));
#7387=CARTESIAN_POINT('Ctrl Pts',(-2.38646057958798,-0.562744471098961,
34.8873698387749));
#7388=CARTESIAN_POINT('Ctrl Pts',(-2.40280007006069,-0.481146623511296,
34.8830216873734));
#7389=CARTESIAN_POINT('Ctrl Pts',(-2.4155486435967,-0.417481470544106,34.8796291257767));
#7390=CARTESIAN_POINT('Ctrl Pts',(-2.42575192533155,-0.353376289000985,
34.87623656418));
#7391=CARTESIAN_POINT('Ctrl Pts',(-2.43339340293186,-0.289044627294339,
34.8728440025833));
#7392=CARTESIAN_POINT('Ctrl Pts',(-2.4446679019399,-0.194127479847733,34.8678385004595));
#7393=CARTESIAN_POINT('Ctrl Pts',(-2.45039627804784,-0.0984857423509142,
34.8628329983358));
#7394=CARTESIAN_POINT('Ctrl Pts',(-2.45049860417835,-0.00261551523903185,
34.857827496212));
#7395=CARTESIAN_POINT('',(-2.45037983021139,-0.00118544631073139,34.0578275478795));
#7396=CARTESIAN_POINT('Ctrl Pts',(-2.45049860417889,-0.0026155147360495,
34.8578274961857));
#7397=CARTESIAN_POINT('Ctrl Pts',(-2.45058303800099,0.0764912707662882,
34.8536972339056));
#7398=CARTESIAN_POINT('Ctrl Pts',(-2.44683277730122,0.155775958000202,34.8495669716254));
#7399=CARTESIAN_POINT('Ctrl Pts',(-2.43922279362101,0.234824217404693,34.8454367093453));
#7400=CARTESIAN_POINT('Ctrl Pts',(-2.43156502720256,0.314368817201754,34.8412805133378));
#7401=CARTESIAN_POINT('Ctrl Pts',(-2.41999881548176,0.393673515189363,34.8371243173304));
#7402=CARTESIAN_POINT('Ctrl Pts',(-2.40455197476298,0.47231350887248,34.8329681213229));
#7403=CARTESIAN_POINT('Ctrl Pts',(-2.38923734093838,0.550280436165396,34.8288474974933));
#7404=CARTESIAN_POINT('Ctrl Pts',(-2.37010832711614,0.627593503657347,34.8247268736638));
#7405=CARTESIAN_POINT('Ctrl Pts',(-2.34724403790772,0.703843502851779,34.8206062498342));
#7406=CARTESIAN_POINT('Ctrl Pts',(-2.32439107691412,0.780055723641504,34.8164876675862));
#7407=CARTESIAN_POINT('Ctrl Pts',(-2.2978066495509,0.855205454128816,34.8123690853382));
#7408=CARTESIAN_POINT('Ctrl Pts',(-2.26762040953671,0.928896080437713,34.8082505030903));
#7409=CARTESIAN_POINT('Ctrl Pts',(-2.23743897407922,1.00257497786646,34.8041325763715));
#7410=CARTESIAN_POINT('Ctrl Pts',(-2.20365704921906,1.07479478108353,34.8000146496527));
#7411=CARTESIAN_POINT('Ctrl Pts',(-2.16645275089669,1.14517803337829,34.7958967229339));
#7412=CARTESIAN_POINT('Ctrl Pts',(-2.12865095884263,1.21669162689593,34.79171266312));
#7413=CARTESIAN_POINT('Ctrl Pts',(-2.08731611560687,1.28630868826316,34.787528603306));
#7414=CARTESIAN_POINT('Ctrl Pts',(-2.04268302315884,1.35366034029909,34.7833445434921));
#7415=CARTESIAN_POINT('Ctrl Pts',(-1.99869892377223,1.42003265721732,34.779221322523));
#7416=CARTESIAN_POINT('Ctrl Pts',(-1.95151221009395,1.48420465471391,34.7750981015539));
#7417=CARTESIAN_POINT('Ctrl Pts',(-1.90138933877843,1.54585537240058,34.7709748805848));
#7418=CARTESIAN_POINT('Ctrl Pts',(-1.85015710989431,1.60887059073297,34.7667604013484));
#7419=CARTESIAN_POINT('Ctrl Pts',(-1.79585756052814,1.6692511875169,34.7625459221121));
#7420=CARTESIAN_POINT('Ctrl Pts',(-1.73881452791423,1.72669461327543,34.7583314428757));
#7421=CARTESIAN_POINT('Ctrl Pts',(-1.68177149530033,1.78413803903396,34.7541169636393));
#7422=CARTESIAN_POINT('Ctrl Pts',(-1.62198542909039,1.838643993989,34.7499024844029));
#7423=CARTESIAN_POINT('Ctrl Pts',(-1.55981354226621,1.8899555453404,34.7456880051665));
#7424=CARTESIAN_POINT('Ctrl Pts',(-1.49730846359926,1.94154208577809,34.7414509396749));
#7425=CARTESIAN_POINT('Ctrl Pts',(-1.43212601463825,1.99011985422216,34.7372138741832));
#7426=CARTESIAN_POINT('Ctrl Pts',(-1.36458746472523,2.03539954336114,34.7329768086916));
#7427=CARTESIAN_POINT('Ctrl Pts',(-1.29714570934954,2.0806143387977,34.7287458156549));
#7428=CARTESIAN_POINT('Ctrl Pts',(-1.22735494169273,2.12254018738515,34.7245148226181));
#7429=CARTESIAN_POINT('Ctrl Pts',(-1.15556958670635,2.16092785170614,34.7202838295813));
#7430=CARTESIAN_POINT('Ctrl Pts',(-1.08363719609896,2.19939414423847,34.7160441703383));
#7431=CARTESIAN_POINT('Ctrl Pts',(-1.0097024079693,2.23430745339174,34.7118045110954));
#7432=CARTESIAN_POINT('Ctrl Pts',(-0.934151230487142,2.26546059965283,34.7075648518524));
#7433=CARTESIAN_POINT('Ctrl Pts',(-0.858890990334782,2.29649377937613,34.7033415189617));
#7434=CARTESIAN_POINT('Ctrl Pts',(-0.782027212945665,2.32379551416278,34.699118186071));
#7435=CARTESIAN_POINT('Ctrl Pts',(-0.703964597663262,2.34720772306944,34.6948948531803));
#7436=CARTESIAN_POINT('Ctrl Pts',(-0.625928348477688,2.37061202436802,34.6906729467445));
#7437=CARTESIAN_POINT('Ctrl Pts',(-0.546694509114701,2.39012927585087,34.6864510403088));
#7438=CARTESIAN_POINT('Ctrl Pts',(-0.466684066711813,2.4056508956782,34.6822291338731));
#7439=CARTESIAN_POINT('Ctrl Pts',(-0.386676329604949,2.42117199069183,34.6780073701875));
#7440=CARTESIAN_POINT('Ctrl Pts',(-0.305892496809424,2.43269763543591,34.673785606502));
#7441=CARTESIAN_POINT('Ctrl Pts',(-0.224763508495889,2.44017040701026,34.6695638428164));
#7442=CARTESIAN_POINT('Ctrl Pts',(-0.143040926436185,2.44769785436161,34.6653111898942));
#7443=CARTESIAN_POINT('Ctrl Pts',(-0.0609685902450196,2.45111281696221,
34.661058536972));
#7444=CARTESIAN_POINT('Ctrl Pts',(0.0210098607397135,2.45040993218516,34.6568058840498));
#7445=CARTESIAN_POINT('Ctrl Pts',(0.10250814005881,2.44971116440899,34.6525781401544));
#7446=CARTESIAN_POINT('Ctrl Pts',(0.183913167396883,2.4449427434225,34.648350396259));
#7447=CARTESIAN_POINT('Ctrl Pts',(0.2647929469091,2.43615166713142,34.6441226523637));
#7448=CARTESIAN_POINT('Ctrl Pts',(0.346387517802885,2.42728289792864,34.639857544928));
#7449=CARTESIAN_POINT('Ctrl Pts',(0.427447035644566,2.41432009501778,34.6355924374924));
#7450=CARTESIAN_POINT('Ctrl Pts',(0.507539056461515,2.39736404331219,34.6313273300567));
#7451=CARTESIAN_POINT('Ctrl Pts',(0.587631077278442,2.3804079916066,34.6270622226211));
#7452=CARTESIAN_POINT('Ctrl Pts',(0.666755155176612,2.35945887307616,34.6227971151854));
#7453=CARTESIAN_POINT('Ctrl Pts',(0.744496864035004,2.33466799983253,34.6185320077498));
#7454=CARTESIAN_POINT('Ctrl Pts',(0.821746605233401,2.31003400901506,34.6142938909084));
#7455=CARTESIAN_POINT('Ctrl Pts',(0.897911870471557,2.28151736349981,34.6100557740671));
#7456=CARTESIAN_POINT('Ctrl Pts',(0.972575452137889,2.24923258910651,34.6058176572258));
#7457=CARTESIAN_POINT('Ctrl Pts',(1.04713463056508,2.21699295901176,34.6015854666087));
#7458=CARTESIAN_POINT('Ctrl Pts',(1.12019587459647,2.18099584830832,34.5973532759916));
#7459=CARTESIAN_POINT('Ctrl Pts',(1.19135785393066,2.14140531284428,34.5931210853744));
#7460=CARTESIAN_POINT('Ctrl Pts',(1.26264068732286,2.1017475409583,34.5888817072477));
#7461=CARTESIAN_POINT('Ctrl Pts',(1.33201735873376,2.05848428635939,34.584642329121));
#7462=CARTESIAN_POINT('Ctrl Pts',(1.39910536548235,2.01182862746271,34.5804029509943));
#7463=CARTESIAN_POINT('Ctrl Pts',(1.46596394810679,1.96533251919509,34.5761780704754));
#7464=CARTESIAN_POINT('Ctrl Pts',(1.53054910463859,1.91546742589171,34.5719531899565));
#7465=CARTESIAN_POINT('Ctrl Pts',(1.59250914367106,1.86248889320824,34.5677283094376));
#7466=CARTESIAN_POINT('Ctrl Pts',(1.65445015555972,1.80952662956166,34.5635047263261));
#7467=CARTESIAN_POINT('Ctrl Pts',(1.7137672992506,1.753453126208,34.5592811432146));
#7468=CARTESIAN_POINT('Ctrl Pts',(1.77014178628731,1.69456434119203,34.5550575601031));
#7469=CARTESIAN_POINT('Ctrl Pts',(1.82651606798102,1.63567577067734,34.5508339923758));
#7470=CARTESIAN_POINT('Ctrl Pts',(1.87994739496282,1.57397227431585,34.5466104246486));
#7471=CARTESIAN_POINT('Ctrl Pts',(1.93015469194864,1.5097857845233,34.5423868569214));
#7472=CARTESIAN_POINT('Ctrl Pts',(1.98068694512054,1.4451838611549,34.5381359530391));
#7473=CARTESIAN_POINT('Ctrl Pts',(2.02795297969414,1.37806705166445,34.5338850491567));
#7474=CARTESIAN_POINT('Ctrl Pts',(2.07170931678843,1.30880508737245,34.5296341452743));
#7475=CARTESIAN_POINT('Ctrl Pts',(2.11524888578472,1.23988624559162,34.5254043002925));
#7476=CARTESIAN_POINT('Ctrl Pts',(2.15531327053484,1.16884388850728,34.5211744553106));
#7477=CARTESIAN_POINT('Ctrl Pts',(2.19170870188478,1.09606715856399,34.5169446103288));
#7478=CARTESIAN_POINT('Ctrl Pts',(2.22837593318399,1.02274693426516,34.5126831769961));
#7479=CARTESIAN_POINT('Ctrl Pts',(2.26131899304487,0.947666762873221,34.5084217436635));
#7480=CARTESIAN_POINT('Ctrl Pts',(2.29038972998756,0.871243441735719,34.5041603103309));
#7481=CARTESIAN_POINT('Ctrl Pts',(2.31946046693025,0.794820120598217,34.4998988769983));
#7482=CARTESIAN_POINT('Ctrl Pts',(2.34465879486285,0.71705411988034,34.4956374436657));
#7483=CARTESIAN_POINT('Ctrl Pts',(2.36588853855451,0.638374242225055,34.4913760103331));
#7484=CARTESIAN_POINT('Ctrl Pts',(2.38693655874852,0.560367852802606,34.4871510542458));
#7485=CARTESIAN_POINT('Ctrl Pts',(2.40416308639464,0.48116882329869,34.4829260981586));
#7486=CARTESIAN_POINT('Ctrl Pts',(2.41743655939156,0.401186653961825,34.4787011420714));
#7487=CARTESIAN_POINT('Ctrl Pts',(2.43069068481461,0.321321067596898,34.474482344331));
#7488=CARTESIAN_POINT('Ctrl Pts',(2.44000312251213,0.240675064453677,34.4702635465906));
#7489=CARTESIAN_POINT('Ctrl Pts',(2.44529243748287,0.159671992500489,34.4660447488501));
#7490=CARTESIAN_POINT('Ctrl Pts',(2.45061171654949,0.0782100362063449,34.4618020515196));
#7491=CARTESIAN_POINT('Ctrl Pts',(2.45186201475039,-0.00361258704432058,
34.457559354189));
#7492=CARTESIAN_POINT('Ctrl Pts',(2.44901297751089,-0.0853562299030711,
34.4533166568584));
#7493=CARTESIAN_POINT('Ctrl Pts',(2.4461852118981,-0.16648955421863,34.4491056365704));
#7494=CARTESIAN_POINT('Ctrl Pts',(2.43931913293496,-0.24754460051366,34.4448946162824));
#7495=CARTESIAN_POINT('Ctrl Pts',(2.42843724804484,-0.328089594940807,34.4406835959944));
#7496=CARTESIAN_POINT('Ctrl Pts',(2.41755909118116,-0.408606995447198,34.4364740183604));
#7497=CARTESIAN_POINT('Ctrl Pts',(2.40266792258095,-0.488614229126138,34.4322644407264));
#7498=CARTESIAN_POINT('Ctrl Pts',(2.38383806368497,-0.567685067732692,34.4280548630924));
#7499=CARTESIAN_POINT('Ctrl Pts',(2.3650088397648,-0.646753239932174,34.4238454274128));
#7500=CARTESIAN_POINT('Ctrl Pts',(2.34224129866315,-0.724884626246403,34.4196359917331));
#7501=CARTESIAN_POINT('Ctrl Pts',(2.31566046996678,-0.801665040919971,34.4154265560534));
#7502=CARTESIAN_POINT('Ctrl Pts',(2.28871480838569,-0.879499298590517,34.4111593441253));
#7503=CARTESIAN_POINT('Ctrl Pts',(2.25785052840493,-0.955944746182242,34.4068921321972));
#7504=CARTESIAN_POINT('Ctrl Pts',(2.22324886302028,-1.03058951240493,34.4026249202691));
#7505=CARTESIAN_POINT('Ctrl Pts',(2.18906615006527,-1.10433048958102,34.3984093751838));
#7506=CARTESIAN_POINT('Ctrl Pts',(2.15123634040796,-1.17631376498225,34.3941938300985));
#7507=CARTESIAN_POINT('Ctrl Pts',(2.10998025654656,-1.24616755172958,34.3899782850132));
#7508=CARTESIAN_POINT('Ctrl Pts',(2.06796570436551,-1.31730555838578,34.3856852396637));
#7509=CARTESIAN_POINT('Ctrl Pts',(2.02239791527187,-1.38623456927327,34.3813921943143));
#7510=CARTESIAN_POINT('Ctrl Pts',(1.97355470503398,-1.45259494568798,34.3770991489648));
#7511=CARTESIAN_POINT('Ctrl Pts',(1.92471149479608,-1.51895532210268,34.3728061036153));
#7512=CARTESIAN_POINT('Ctrl Pts',(1.87259323456035,-1.58274671710294,34.3685130582658));
#7513=CARTESIAN_POINT('Ctrl Pts',(1.81751758542159,-1.64364840421645,34.3642200129163));
#7514=CARTESIAN_POINT('Ctrl Pts',(1.7632259248842,-1.70368317048112,34.3599880780335));
#7515=CARTESIAN_POINT('Ctrl Pts',(1.7058548403839,-1.7611375266858,34.3557561431507));
#7516=CARTESIAN_POINT('Ctrl Pts',(1.64567922433033,-1.81567897509651,34.3515242082678));
#7517=CARTESIAN_POINT('Ctrl Pts',(1.58558996222947,-1.87014215476706,34.3472983463482));
#7518=CARTESIAN_POINT('Ctrl Pts',(1.52270450323097,-1.92170041925766,34.3430724844286));
#7519=CARTESIAN_POINT('Ctrl Pts',(1.45733640531247,-1.97005605294645,34.3388466225091));
#7520=CARTESIAN_POINT('Ctrl Pts',(1.39173504054954,-2.01858424429624,34.3346056805503));
#7521=CARTESIAN_POINT('Ctrl Pts',(1.32363360310567,-2.06388655353515,34.3303647385916));
#7522=CARTESIAN_POINT('Ctrl Pts',(1.25338465788447,-2.10570110637285,34.3261237966329));
#7523=CARTESIAN_POINT('Ctrl Pts',(1.18351173545728,-2.14729183770064,34.3219055552405));
#7524=CARTESIAN_POINT('Ctrl Pts',(1.11151463869165,-2.18543181395312,34.3176873138482));
#7525=CARTESIAN_POINT('Ctrl Pts',(1.0377700097019,-2.2199062270653,34.3134690724558));
#7526=CARTESIAN_POINT('Ctrl Pts',(0.964049845847686,-2.25436920312504,34.3092522304854));
#7527=CARTESIAN_POINT('Ctrl Pts',(0.888583721765571,-2.28516883433822,34.3050353885149));
#7528=CARTESIAN_POINT('Ctrl Pts',(0.811771585361969,-2.31213692137791,34.3008185465444));
#7529=CARTESIAN_POINT('Ctrl Pts',(0.734961421673215,-2.33910431581421,34.2966018128723));
#7530=CARTESIAN_POINT('Ctrl Pts',(0.656805753260624,-2.36224020879375,34.2923850792002));
#7531=CARTESIAN_POINT('Ctrl Pts',(0.577721790458789,-2.38142557784809,34.2881683455281));
#7532=CARTESIAN_POINT('Ctrl Pts',(0.49785086726638,-2.4008018595096,34.283909651359));
#7533=CARTESIAN_POINT('Ctrl Pts',(0.417033536840315,-2.41614842429626,34.27965095719));
#7534=CARTESIAN_POINT('Ctrl Pts',(0.335710518173299,-2.42739545562478,34.2753922630209));
#7535=CARTESIAN_POINT('Ctrl Pts',(0.255071927144433,-2.43854783012409,34.2711694107087));
#7536=CARTESIAN_POINT('Ctrl Pts',(0.173936601210025,-2.44566943717576,34.2669465583965));
#7537=CARTESIAN_POINT('Ctrl Pts',(0.092737889530107,-2.4487445628006,34.2627237060843));
#7538=CARTESIAN_POINT('Ctrl Pts',(0.0105054052777507,-2.45185883905311,
34.2584470909868));
#7539=CARTESIAN_POINT('Ctrl Pts',(-0.0717915981462766,-2.45082287749668,
34.2541704758894));
#7540=CARTESIAN_POINT('Ctrl Pts',(-0.153706531475772,-2.44567466196583,
34.2498938607919));
#7541=CARTESIAN_POINT('Ctrl Pts',(-0.235621464805245,-2.44052644643498,
34.2456172456944));
#7542=CARTESIAN_POINT('Ctrl Pts',(-0.317153850472105,-2.43126609641305,
34.241340630597));
#7543=CARTESIAN_POINT('Ctrl Pts',(-0.397867904257343,-2.41798498356832,
34.2370640154995));
#7544=CARTESIAN_POINT('Ctrl Pts',(-0.477732110699871,-2.40484370905321,
34.232832429363));
#7545=CARTESIAN_POINT('Ctrl Pts',(-0.557093992558343,-2.38771681174341,
34.2286008432265));
#7546=CARTESIAN_POINT('Ctrl Pts',(-0.63552522338495,-2.36665543339995,34.22436925709));
#7547=CARTESIAN_POINT('Ctrl Pts',(-0.713844152186092,-2.34562421186294,
34.2201437299646));
#7548=CARTESIAN_POINT('Ctrl Pts',(-0.791234631374894,-2.32066981764097,
34.2159182028391));
#7549=CARTESIAN_POINT('Ctrl Pts',(-0.86727665140296,-2.29189473142448,34.2116926757137));
#7550=CARTESIAN_POINT('Ctrl Pts',(-0.943597612318161,-2.26301409109365,
34.2074516483124));
#7551=CARTESIAN_POINT('Ctrl Pts',(-1.01855973416004,-2.23028475108662,34.2032106209111));
#7552=CARTESIAN_POINT('Ctrl Pts',(-1.09175191422655,-2.19386143768987,34.1989695935098));
#7553=CARTESIAN_POINT('Ctrl Pts',(-1.16454570854388,-2.15763637674279,34.194751650062));
#7554=CARTESIAN_POINT('Ctrl Pts',(-1.23558835825757,-2.11775765891632,34.1905337066142));
#7555=CARTESIAN_POINT('Ctrl Pts',(-1.30449542205291,-2.07442569012317,34.1863157631664));
#7556=CARTESIAN_POINT('Ctrl Pts',(-1.37337986274379,-2.03110794779103,34.1820992045254));
#7557=CARTESIAN_POINT('Ctrl Pts',(-1.44012971669603,-1.98433945321482,34.1778826458845));
#7558=CARTESIAN_POINT('Ctrl Pts',(-1.50438712146545,-1.93436543568399,34.1736660872435));
#7559=CARTESIAN_POINT('Ctrl Pts',(-1.56864310554956,-1.88439252304298,34.1694496218277));
#7560=CARTESIAN_POINT('Ctrl Pts',(-1.6304063837682,-1.83121451460029,34.1652331564118));
#7561=CARTESIAN_POINT('Ctrl Pts',(-1.68935110363642,-1.77511777035846,34.161016690996));
#7562=CARTESIAN_POINT('Ctrl Pts',(-1.74889122612015,-1.71845439099957,34.1567576349199));
#7563=CARTESIAN_POINT('Ctrl Pts',(-1.80555516479479,-1.65881329779533,34.1524985788438));
#7564=CARTESIAN_POINT('Ctrl Pts',(-1.85904559641062,-1.59652739421104,34.1482395227677));
#7565=CARTESIAN_POINT('Ctrl Pts',(-1.912078472171,-1.53477428273621,34.144016898554));
#7566=CARTESIAN_POINT('Ctrl Pts',(-1.96199168706069,-1.47042184491263,34.1397942743404));
#7567=CARTESIAN_POINT('Ctrl Pts',(-2.0085375323217,-1.40382592626546,34.1355716501267));
#7568=CARTESIAN_POINT('Ctrl Pts',(-2.05568575838159,-1.33636814545953,34.1312943781194));
#7569=CARTESIAN_POINT('Ctrl Pts',(-2.09937856932165,-1.26660881596614,34.1270171061121));
#7570=CARTESIAN_POINT('Ctrl Pts',(-2.1394061252549,-1.19494421678245,34.1227398341048));
#7571=CARTESIAN_POINT('Ctrl Pts',(-2.17943368118814,-1.12327961759877,34.1184625620975));
#7572=CARTESIAN_POINT('Ctrl Pts',(-2.21579582410861,-1.04971021558846,34.1141852900902));
#7573=CARTESIAN_POINT('Ctrl Pts',(-2.24833350072709,-0.974652101782096,
34.1099080180829));
#7574=CARTESIAN_POINT('Ctrl Pts',(-2.28384506994657,-0.892733794117691,
34.1052398101239));
#7575=CARTESIAN_POINT('Ctrl Pts',(-2.31491648604063,-0.808778775978598,
34.1005716021649));
#7576=CARTESIAN_POINT('Ctrl Pts',(-2.34133381517415,-0.723260821503584,
34.0959033942059));
#7577=CARTESIAN_POINT('Ctrl Pts',(-2.36767361785023,-0.637993835021024,
34.0912488859523));
#7578=CARTESIAN_POINT('Ctrl Pts',(-2.38938645150022,-0.551173331584216,
34.0865943776986));
#7579=CARTESIAN_POINT('Ctrl Pts',(-2.40630644908103,-0.463292049479658,
34.081939869445));
#7580=CARTESIAN_POINT('Ctrl Pts',(-2.42314169952809,-0.375850938050761,
34.0773086742108));
#7581=CARTESIAN_POINT('Ctrl Pts',(-2.43523188078036,-0.287359925256168,
34.0726774789767));
#7582=CARTESIAN_POINT('Ctrl Pts',(-2.44246148854258,-0.198323289067031,
34.0680462837425));
#7583=CARTESIAN_POINT('Ctrl Pts',(-2.44777886596267,-0.132836831930789,
34.0646400390643));
#7584=CARTESIAN_POINT('Ctrl Pts',(-2.45046784559981,-0.0670556257196897,
34.061233794386));
#7585=CARTESIAN_POINT('Ctrl Pts',(-2.45049971322092,-0.0011855396130741,
34.0578275497077));
#7586=CARTESIAN_POINT('',(-2.45049908813345,0.00211401446109679,33.2578274733736));
#7587=CARTESIAN_POINT('Ctrl Pts',(-2.44699180045922,-0.00118280948075616,
34.057827496212));
#7588=CARTESIAN_POINT('Ctrl Pts',(-2.44492511997085,0.482062993109739,34.0328023376967));
#7589=CARTESIAN_POINT('Ctrl Pts',(-2.07248525985984,1.78674845601148,33.9653918467091));
#7590=CARTESIAN_POINT('Ctrl Pts',(0.0507853920667545,2.89698596197385,33.8555960232493));
#7591=CARTESIAN_POINT('Ctrl Pts',(2.46316807672906,1.52579262516589,33.7284400258327));
#7592=CARTESIAN_POINT('Ctrl Pts',(2.61640501014275,-1.24485973594507,33.6012840284158));
#7593=CARTESIAN_POINT('Ctrl Pts',(0.36993009926562,-2.87373621598164,33.4741280309992));
#7594=CARTESIAN_POINT('Ctrl Pts',(-1.95817334103329,-1.96722679795361,33.3596425202646));
#7595=CARTESIAN_POINT('Ctrl Pts',(-2.44423543888734,-0.570546915852272,
33.2875423420022));
#7596=CARTESIAN_POINT('Ctrl Pts',(-2.44892925407896,0.00211222005066472,
33.257827496212));
#7597=CARTESIAN_POINT('',(-2.45089796908517,0.000113383330988791,32.457827496212));
#7598=CARTESIAN_POINT('Ctrl Pts',(-2.45049908813345,0.00211401446109679,
33.2578274733736));
#7599=CARTESIAN_POINT('Ctrl Pts',(-2.45041450413369,0.100161127234811,33.2527431029097));
#7600=CARTESIAN_POINT('Ctrl Pts',(-2.44444165697049,0.197950870004684,33.2476587324459));
#7601=CARTESIAN_POINT('Ctrl Pts',(-2.43269561295387,0.294859805187173,33.242574361982));
#7602=CARTESIAN_POINT('Ctrl Pts',(-2.4207837487679,0.39313681425223,33.2374182149124));
#7603=CARTESIAN_POINT('Ctrl Pts',(-2.40293460772991,0.490507975166501,33.2322620678427));
#7604=CARTESIAN_POINT('Ctrl Pts',(-2.37931704861462,0.586345147649234,33.227105920773));
#7605=CARTESIAN_POINT('Ctrl Pts',(-2.36818669111253,0.631510779987266,33.2246759592372));
#7606=CARTESIAN_POINT('Ctrl Pts',(-2.35577585951501,0.676336028494037,33.2222459977015));
#7607=CARTESIAN_POINT('Ctrl Pts',(-2.34210586539719,0.720756800364789,33.2198160361657));
#7608=CARTESIAN_POINT('Ctrl Pts',(-2.31830558535038,0.79809602972413,33.2155853273186));
#7609=CARTESIAN_POINT('Ctrl Pts',(-2.29062567491792,0.874400559717126,33.2113546184715));
#7610=CARTESIAN_POINT('Ctrl Pts',(-2.25917440202268,0.949253006972044,33.2071239096243));
#7611=CARTESIAN_POINT('Ctrl Pts',(-2.22776831532491,1.0239979133502,33.2028992790573));
#7612=CARTESIAN_POINT('Ctrl Pts',(-2.19260180589857,1.09729445521621,33.1986746484902));
#7613=CARTESIAN_POINT('Ctrl Pts',(-2.15383289516444,1.16874039448782,33.1944500179232));
#7614=CARTESIAN_POINT('Ctrl Pts',(-2.11491147791859,1.24046738294985,33.1902087687909));
#7615=CARTESIAN_POINT('Ctrl Pts',(-2.07235939643465,1.31032872450256,33.1859675196587));
#7616=CARTESIAN_POINT('Ctrl Pts',(-2.02638541823373,1.37793772964155,33.1817262705264));
#7617=CARTESIAN_POINT('Ctrl Pts',(-1.98067422462602,1.44516028562803,33.1775092641283));
#7618=CARTESIAN_POINT('Ctrl Pts',(-1.93158041103865,1.51015579536423,33.1732922577301));
#7619=CARTESIAN_POINT('Ctrl Pts',(-1.87935425682599,1.57257045226916,33.1690752513319));
#7620=CARTESIAN_POINT('Ctrl Pts',(-1.82714541628774,1.63496441787365,33.1648596429282));
#7621=CARTESIAN_POINT('Ctrl Pts',(-1.77180659544445,1.69477887331527,33.1606440345245));
#7622=CARTESIAN_POINT('Ctrl Pts',(-1.71362890871323,1.75169238544394,33.1564284261208));
#7623=CARTESIAN_POINT('Ctrl Pts',(-1.65545267334021,1.80860447775178,33.1522129228839));
#7624=CARTESIAN_POINT('Ctrl Pts',(-1.59443804608623,1.86261544619688,33.1479974196469));
#7625=CARTESIAN_POINT('Ctrl Pts',(-1.53091258389673,1.91344111758544,33.1437819164099));
#7626=CARTESIAN_POINT('Ctrl Pts',(-1.46671422046173,1.96480516612865,33.1395217599382));
#7627=CARTESIAN_POINT('Ctrl Pts',(-1.39995188104122,2.01291571941342,33.1352616034664));
#7628=CARTESIAN_POINT('Ctrl Pts',(-1.33099594219616,2.0575227949788,33.1310014469947));
#7629=CARTESIAN_POINT('Ctrl Pts',(-1.26266340285344,2.10172659811871,33.1267798046737));
#7630=CARTESIAN_POINT('Ctrl Pts',(-1.19217720525324,2.14248983358113,33.1225581623527));
#7631=CARTESIAN_POINT('Ctrl Pts',(-1.11992323246884,2.17961515029065,33.1183365200317));
#7632=CARTESIAN_POINT('Ctrl Pts',(-1.0466804974247,2.21724850981954,33.1140571064846));
#7633=CARTESIAN_POINT('Ctrl Pts',(-0.9716216894346,2.2511434269564,33.1097776929375));
#7634=CARTESIAN_POINT('Ctrl Pts',(-0.895168572881708,2.28114521153848,33.1054982793903));
#7635=CARTESIAN_POINT('Ctrl Pts',(-0.818715456328837,2.31114699612055,33.1012188658432));
#7636=CARTESIAN_POINT('Ctrl Pts',(-0.740868517148116,2.33725555424667,33.0969394522961));
#7637=CARTESIAN_POINT('Ctrl Pts',(-0.662062326808542,2.35936934908904,33.092660038749));
#7638=CARTESIAN_POINT('Ctrl Pts',(-0.584153156669579,2.38123143120935,33.0884293361011));
#7639=CARTESIAN_POINT('Ctrl Pts',(-0.505013440062888,2.39927149929197,33.0841986334532));
#7640=CARTESIAN_POINT('Ctrl Pts',(-0.425052711371263,2.41335460356657,33.0799679308054));
#7641=CARTESIAN_POINT('Ctrl Pts',(-0.34520686361132,2.42741747440699,33.0757433064796));
#7642=CARTESIAN_POINT('Ctrl Pts',(-0.264542800566075,2.43753459225269,33.0715186821538));
#7643=CARTESIAN_POINT('Ctrl Pts',(-0.18348426035662,2.44362103776371,33.067294057828));
#7644=CARTESIAN_POINT('Ctrl Pts',(-0.102106707498751,2.44973143698888,33.0630528071407));
#7645=CARTESIAN_POINT('Ctrl Pts',(-0.0203320227278529,2.4517792415305,33.0588115564533));
#7646=CARTESIAN_POINT('Ctrl Pts',(0.0614016513507029,2.44973061523332,33.054570305766));
#7647=CARTESIAN_POINT('Ctrl Pts',(0.142667989344273,2.44769370255361,33.0503533056647));
#7648=CARTESIAN_POINT('Ctrl Pts',(0.223893314766545,2.44160708876418,33.0461363055634));
#7649=CARTESIAN_POINT('Ctrl Pts',(0.304644658920101,2.4314896425425,33.041919305462));
#7650=CARTESIAN_POINT('Ctrl Pts',(0.385369232744089,2.42137555041198,33.037703703362));
#7651=CARTESIAN_POINT('Ctrl Pts',(0.465619676250428,2.40723333725223,33.0334881012619));
#7652=CARTESIAN_POINT('Ctrl Pts',(0.544968130308082,2.38913373149108,33.0292724991619));
#7653=CARTESIAN_POINT('Ctrl Pts',(0.624314604891742,2.37103457725353,33.0250570022268));
#7654=CARTESIAN_POINT('Ctrl Pts',(0.702758681592593,2.34897833118418,33.0208415052916));
#7655=CARTESIAN_POINT('Ctrl Pts',(0.779884097420945,2.32308653402966,33.0166260083565));
#7656=CARTESIAN_POINT('Ctrl Pts',(0.857826726435443,2.29692038998415,33.0123658444378));
#7657=CARTESIAN_POINT('Ctrl Pts',(0.934422118991902,2.26683706757854,33.0081056805191));
#7658=CARTESIAN_POINT('Ctrl Pts',(1.00925957123512,2.2330126215206,33.0038455166005));
#7659=CARTESIAN_POINT('Ctrl Pts',(1.08342021274699,2.19949407508094,32.999623880512));
#7660=CARTESIAN_POINT('Ctrl Pts',(1.15585419266241,2.16230207003995,32.9954022444236));
#7661=CARTESIAN_POINT('Ctrl Pts',(1.2261866659655,2.12165419194751,32.9911806083352));
#7662=CARTESIAN_POINT('Ctrl Pts',(1.29748194996689,2.08044986801926,32.9869011805014));
#7663=CARTESIAN_POINT('Ctrl Pts',(1.36661733968173,2.03569460568112,32.9826217526676));
#7664=CARTESIAN_POINT('Ctrl Pts',(1.43323442601716,1.98765925904801,32.9783423248337));
#7665=CARTESIAN_POINT('Ctrl Pts',(1.49985151235258,1.93962391241489,32.9740628969999));
#7666=CARTESIAN_POINT('Ctrl Pts',(1.56394995326115,1.88830883921173,32.9697834691661));
#7667=CARTESIAN_POINT('Ctrl Pts',(1.62520909562318,1.83402443972366,32.9655040413323));
#7668=CARTESIAN_POINT('Ctrl Pts',(1.68577070373729,1.78035815577412,32.9612733416941));
#7669=CARTESIAN_POINT('Ctrl Pts',(1.74378516371167,1.72358800022147,32.957042642056));
#7670=CARTESIAN_POINT('Ctrl Pts',(1.79891728872159,1.66398522780058,32.9528119424178));
#7671=CARTESIAN_POINT('Ctrl Pts',(1.85397020348703,1.60446808875905,32.9485873211732));
#7672=CARTESIAN_POINT('Ctrl Pts',(1.90614869472641,1.54212675404099,32.9443626999286));
#7673=CARTESIAN_POINT('Ctrl Pts',(1.95515194892122,1.47727150741817,32.940138078684));
#7674=CARTESIAN_POINT('Ctrl Pts',(2.00434810422372,1.41216095838496,32.9358968272353));
#7675=CARTESIAN_POINT('Ctrl Pts',(2.05034361506433,1.34451697771044,32.9316555757866));
#7676=CARTESIAN_POINT('Ctrl Pts',(2.09287281695147,1.27468961793278,32.9274143243379));
#7677=CARTESIAN_POINT('Ctrl Pts',(2.13515880572762,1.20526158211724,32.9231973274699));
#7678=CARTESIAN_POINT('Ctrl Pts',(2.17401777939715,1.13367547293135,32.9189803306019));
#7679=CARTESIAN_POINT('Ctrl Pts',(2.20923118738444,1.06030552704772,32.914763333734));
#7680=CARTESIAN_POINT('Ctrl Pts',(2.24443292114961,0.986959905337576,32.9105477349175));
#7681=CARTESIAN_POINT('Ctrl Pts',(2.27599128825168,0.911832040272801,32.906332136101));
#7682=CARTESIAN_POINT('Ctrl Pts',(2.3037341059364,0.835319950166052,32.9021165372845));
#7683=CARTESIAN_POINT('Ctrl Pts',(2.3314762312292,0.758809769611306,32.8979010436789));
#7684=CARTESIAN_POINT('Ctrl Pts',(2.35540283892995,0.680915870279583,32.8936855500733));
#7685=CARTESIAN_POINT('Ctrl Pts',(2.37539074539078,0.602054031389063,32.8894700564677));
#7686=CARTESIAN_POINT('Ctrl Pts',(2.39559047565151,0.522356446423122,32.885209888755));
#7687=CARTESIAN_POINT('Ctrl Pts',(2.41176739135415,0.441670749723604,32.8809497210424));
#7688=CARTESIAN_POINT('Ctrl Pts',(2.42384715130507,0.360437563400786,32.8766895533297));
#7689=CARTESIAN_POINT('Ctrl Pts',(2.43581764467612,0.279939165888083,32.8724679206506));
#7690=CARTESIAN_POINT('Ctrl Pts',(2.44376482069037,0.198903617470079,32.8682462879715));
#7691=CARTESIAN_POINT('Ctrl Pts',(2.44766867034687,0.117763874776457,32.8640246552924));
#7692=CARTESIAN_POINT('Ctrl Pts',(2.45162597147196,0.0355131675761901,32.8597452200629));
#7693=CARTESIAN_POINT('Ctrl Pts',(2.45142838660174,-0.0468441141031322,
32.8554657848334));
#7694=CARTESIAN_POINT('Ctrl Pts',(2.44710959160658,-0.128859988619679,32.8511863496039));
#7695=CARTESIAN_POINT('Ctrl Pts',(2.44279079661142,-0.210875863136225,32.8469069143744));
#7696=CARTESIAN_POINT('Ctrl Pts',(2.43435090706428,-0.292549849227604,32.8426274791449));
#7697=CARTESIAN_POINT('Ctrl Pts',(2.42187728965222,-0.373444298211699,32.8383480439155));
#7698=CARTESIAN_POINT('Ctrl Pts',(2.4095457158724,-0.453417559621855,32.8341173408624));
#7699=CARTESIAN_POINT('Ctrl Pts',(2.39322547571729,-0.532929756398903,32.8298866378093));
#7700=CARTESIAN_POINT('Ctrl Pts',(2.3729631552908,-0.61155221660324,32.8256559347562));
#7701=CARTESIAN_POINT('Ctrl Pts',(2.35272994617263,-0.690061718240528,32.8214313100445));
#7702=CARTESIAN_POINT('Ctrl Pts',(2.32856602022196,-0.767683575562253,32.8172066853328));
#7703=CARTESIAN_POINT('Ctrl Pts',(2.30056938760177,-0.843996885556813,32.8129820606211));
#7704=CARTESIAN_POINT('Ctrl Pts',(2.27246257512076,-0.920610524165473,32.8087408100326));
#7705=CARTESIAN_POINT('Ctrl Pts',(2.24049289660263,-0.995904824854882,32.8044995594442));
#7706=CARTESIAN_POINT('Ctrl Pts',(2.20481082769516,-1.06946690649041,32.8002583088558));
#7707=CARTESIAN_POINT('Ctrl Pts',(2.16933277775891,-1.14260838302442,32.796041308419));
#7708=CARTESIAN_POINT('Ctrl Pts',(2.13018487983236,-1.21403697269545,32.7918243079822));
#7709=CARTESIAN_POINT('Ctrl Pts',(2.08756345099631,-1.28336631094337,32.7876073075454));
#7710=CARTESIAN_POINT('Ctrl Pts',(2.04495615202774,-1.35267266511054,32.7833917051297));
#7711=CARTESIAN_POINT('Ctrl Pts',(1.99887785229089,-1.41988075401458,32.779176102714));
#7712=CARTESIAN_POINT('Ctrl Pts',(1.94956996752,-1.48463032157641,32.7749605002983));
#7713=CARTESIAN_POINT('Ctrl Pts',(1.90026331305108,-1.54937827354429,32.770745003068));
#7714=CARTESIAN_POINT('Ctrl Pts',(1.84772751638552,-1.61166745680075,32.7665295058376));
#7715=CARTESIAN_POINT('Ctrl Pts',(1.79224545454304,-1.67116919570396,32.7623140086072));
#7716=CARTESIAN_POINT('Ctrl Pts',(1.73617551964589,-1.73130139908245,32.7580538450981));
#7717=CARTESIAN_POINT('Ctrl Pts',(1.67709683077161,-1.78858637106687,32.7537936815891));
#7718=CARTESIAN_POINT('Ctrl Pts',(1.61533959380088,-1.84272305208873,32.7495335180801));
#7719=CARTESIAN_POINT('Ctrl Pts',(1.55414086405891,-1.89637014307751,32.7453118817499));
#7720=CARTESIAN_POINT('Ctrl Pts',(1.49031224568645,-1.94692541421358,32.7410902454197));
#7721=CARTESIAN_POINT('Ctrl Pts',(1.42420691762321,-1.99413763461658,32.7368686090896));
#7722=CARTESIAN_POINT('Ctrl Pts',(1.3571966613759,-2.04199615192372,32.7325891819911));
#7723=CARTESIAN_POINT('Ctrl Pts',(1.28784730742235,-2.08641913142763,32.7283097548926));
#7724=CARTESIAN_POINT('Ctrl Pts',(1.21655372943403,-2.12719234518182,32.7240303277942));
#7725=CARTESIAN_POINT('Ctrl Pts',(1.14526015144572,-2.16796555893602,32.7197509006957));
#7726=CARTESIAN_POINT('Ctrl Pts',(1.07202281661275,-2.20508884355044,32.7154714735972));
#7727=CARTESIAN_POINT('Ctrl Pts',(0.997256979744859,-2.23839870584982,32.7111920464988));
#7728=CARTESIAN_POINT('Ctrl Pts',(0.923342419706714,-2.27132930517074,32.7069613445572));
#7729=CARTESIAN_POINT('Ctrl Pts',(0.847655992323171,-2.30065677971026,32.7027306426156));
#7730=CARTESIAN_POINT('Ctrl Pts',(0.770583328756321,-2.32618820894674,32.6984999406741));
#7731=CARTESIAN_POINT('Ctrl Pts',(0.693621397341056,-2.35168295656406,32.6942753170839));
#7732=CARTESIAN_POINT('Ctrl Pts',(0.615277622969492,-2.37339234556173,32.6900506934937));
#7733=CARTESIAN_POINT('Ctrl Pts',(0.535958946636366,-2.39117089676176,32.6858260699035));
#7734=CARTESIAN_POINT('Ctrl Pts',(0.456328087785067,-2.40901942079971,32.6815848190359));
#7735=CARTESIAN_POINT('Ctrl Pts',(0.375715069952116,-2.42290590555947,32.6773435681684));
#7736=CARTESIAN_POINT('Ctrl Pts',(0.294548495561631,-2.43273332565704,32.6731023173008));
#7737=CARTESIAN_POINT('Ctrl Pts',(0.213846033475075,-2.44250455234474,32.6688853180014));
#7738=CARTESIAN_POINT('Ctrl Pts',(0.132596794480244,-2.44826295159171,32.664668318702));
#7739=CARTESIAN_POINT('Ctrl Pts',(0.0512319056779359,-2.4499643960353,32.6604513194026));
#7740=CARTESIAN_POINT('Ctrl Pts',(-0.0301060089409373,-2.45166527641402,
32.6562357181278));
#7741=CARTESIAN_POINT('Ctrl Pts',(-0.111559032639499,-2.44931186314919,
32.652020116853));
#7742=CARTESIAN_POINT('Ctrl Pts',(-0.192693572261953,-2.44291208135064,
32.6478045155781));
#7743=CARTESIAN_POINT('Ctrl Pts',(-0.273826087424948,-2.43651245923869,
32.6435890194905));
#7744=CARTESIAN_POINT('Ctrl Pts',(-0.35463967077687,-2.42606670698683,32.6393735234028));
#7745=CARTESIAN_POINT('Ctrl Pts',(-0.434704833013202,-2.41163470661603,
32.6351580273152));
#7746=CARTESIAN_POINT('Ctrl Pts',(-0.515618391701819,-2.39704978008393,
32.6308978624624));
#7747=CARTESIAN_POINT('Ctrl Pts',(-0.595767094165784,-2.37839369335156,
32.6266376976097));
#7748=CARTESIAN_POINT('Ctrl Pts',(-0.67471904436235,-2.35578107242052,32.6223775327569));
#7749=CARTESIAN_POINT('Ctrl Pts',(-0.752956939641188,-2.33337296389402,
32.6181558975625));
#7750=CARTESIAN_POINT('Ctrl Pts',(-0.830019217737815,-2.3070798107042,32.613934262368));
#7751=CARTESIAN_POINT('Ctrl Pts',(-0.905503439327968,-2.2770625312813,32.6097126271735));
#7752=CARTESIAN_POINT('Ctrl Pts',(-0.982021045305181,-2.24663431315832,
32.6054331974916));
#7753=CARTESIAN_POINT('Ctrl Pts',(-1.05691661037709,-2.21237943537851,32.6011537678097));
#7754=CARTESIAN_POINT('Ctrl Pts',(-1.12979623069003,-2.1745139059382,32.5968743381278));
#7755=CARTESIAN_POINT('Ctrl Pts',(-1.20267585100298,-2.13664837649788,32.5925949084459));
#7756=CARTESIAN_POINT('Ctrl Pts',(-1.27353913624145,-2.09517249973101,32.588315478764));
#7757=CARTESIAN_POINT('Ctrl Pts',(-1.34202380372876,-2.05034688777909,32.5840360490821));
#7758=CARTESIAN_POINT('Ctrl Pts',(-1.40963924105352,-2.00609021739311,32.5798109353441));
#7759=CARTESIAN_POINT('Ctrl Pts',(-1.47519193949527,-1.9584009273097,32.5755858216061));
#7760=CARTESIAN_POINT('Ctrl Pts',(-1.53831148274827,-1.90749784588209,32.5713607078681));
#7761=CARTESIAN_POINT('Ctrl Pts',(-1.60134028247577,-1.85666794503897,32.5671416683457));
#7762=CARTESIAN_POINT('Ctrl Pts',(-1.66194251379264,-1.8026337186582,32.5629226288233));
#7763=CARTESIAN_POINT('Ctrl Pts',(-1.71977605472221,-1.74565763298652,32.5587035893009));
#7764=CARTESIAN_POINT('Ctrl Pts',(-1.77754248218487,-1.68874766573987,32.554489445802));
#7765=CARTESIAN_POINT('Ctrl Pts',(-1.83254627374902,-1.62890294921535,32.550275302303));
#7766=CARTESIAN_POINT('Ctrl Pts',(-1.88447894375625,-1.56642566390472,32.546061158804));
#7767=CARTESIAN_POINT('Ctrl Pts',(-1.93637859000849,-1.50398810762327,32.5418496950602));
#7768=CARTESIAN_POINT('Ctrl Pts',(-1.98521069363507,-1.43892166303614,32.5376382313165));
#7769=CARTESIAN_POINT('Ctrl Pts',(-2.0307049877932,-1.37156388934377,32.5334267675727));
#7770=CARTESIAN_POINT('Ctrl Pts',(-2.07618439996395,-1.30422814956921,32.5292166814731));
#7771=CARTESIAN_POINT('Ctrl Pts',(-2.11832790992056,-1.23460295530773,32.5250065953735));
#7772=CARTESIAN_POINT('Ctrl Pts',(-2.15690765419008,-1.16305615569336,32.5207965092739));
#7773=CARTESIAN_POINT('Ctrl Pts',(-2.19548669074459,-1.0915106685487,32.5165865004051));
#7774=CARTESIAN_POINT('Ctrl Pts',(-2.23050187128866,-1.01804405729231,32.5123764915362));
#7775=CARTESIAN_POINT('Ctrl Pts',(-2.26177122541205,-0.943048871426129,
32.5081664826673));
#7776=CARTESIAN_POINT('Ctrl Pts',(-2.29307152271146,-0.867979472666756,
32.5039523077052));
#7777=CARTESIAN_POINT('Ctrl Pts',(-2.32061840868368,-0.791378909078912,
32.4997381327431));
#7778=CARTESIAN_POINT('Ctrl Pts',(-2.34427827865547,-0.71365930402688,32.495523957781));
#7779=CARTESIAN_POINT('Ctrl Pts',(-2.36794930498103,-0.635903051799291,
32.4913077957062));
#7780=CARTESIAN_POINT('Ctrl Pts',(-2.38772955051801,-0.557027160022369,
32.4870916336314));
#7781=CARTESIAN_POINT('Ctrl Pts',(-2.40353614312668,-0.477456028010667,
32.4828754715567));
#7782=CARTESIAN_POINT('Ctrl Pts',(-2.41937149873157,-0.397740101720686,
32.4786516374012));
#7783=CARTESIAN_POINT('Ctrl Pts',(-2.43121868415156,-0.317326869841374,
32.4744278032458));
#7784=CARTESIAN_POINT('Ctrl Pts',(-2.43904654596525,-0.23664783247469,32.4702039690903));
#7785=CARTESIAN_POINT('Ctrl Pts',(-2.44669215229249,-0.157847238743247,
32.4660784781309));
#7786=CARTESIAN_POINT('Ctrl Pts',(-2.45050364776331,-0.0787934942721454,
32.4619529871714));
#7787=CARTESIAN_POINT('Ctrl Pts',(-2.45049999737776,0.00011336492003957,
32.457827496212));
#7788=CARTESIAN_POINT('',(-2.45049903342988,-0.00217650160221668,31.657827496212));
#7789=CARTESIAN_POINT('Ctrl Pts',(-2.45453274682372,0.000113551482912981,
32.457827496212));
#7790=CARTESIAN_POINT('Ctrl Pts',(-2.45453682007855,0.00616397536570763,
32.4575116813631));
#7791=CARTESIAN_POINT('Ctrl Pts',(-2.45451638727492,0.0122143709360244,
32.4571958665142));
#7792=CARTESIAN_POINT('Ctrl Pts',(-2.44842902388592,0.830260198165473,32.414494719193));
#7793=CARTESIAN_POINT('Ctrl Pts',(-1.55054418679137,2.44765985374896,32.3297240542486));
#7794=CARTESIAN_POINT('Ctrl Pts',(1.2184054487905,2.62882374300816,32.2025680568319));
#7795=CARTESIAN_POINT('Ctrl Pts',(2.86986248022965,0.398892763100646,32.075412059415));
#7796=CARTESIAN_POINT('Ctrl Pts',(1.88914963708073,-2.19689319950944,31.9482560619984));
#7797=CARTESIAN_POINT('Ctrl Pts',(-0.824246492121587,-2.777740774871,31.8211000645817));
#7798=CARTESIAN_POINT('Ctrl Pts',(-2.31451204546487,-1.28030818469935,31.7242907365184));
#7799=CARTESIAN_POINT('Ctrl Pts',(-2.45124436907125,-0.234112490484375,
31.6698667409274));
#7800=CARTESIAN_POINT('Ctrl Pts',(-2.44926684387645,-0.00218661161304503,
31.6578280778087));
#7801=CARTESIAN_POINT('',(-2.45028716750641,0.000988674573411882,30.8578274549158));
#7802=CARTESIAN_POINT('Ctrl Pts',(-2.45049903342988,-0.00217650160221668,
31.657827496212));
#7803=CARTESIAN_POINT('Ctrl Pts',(-2.45057066460466,0.0784722442460725,
31.6536433021141));
#7804=CARTESIAN_POINT('Ctrl Pts',(-2.44665665890771,0.159202294317996,31.6494591080163));
#7805=CARTESIAN_POINT('Ctrl Pts',(-2.4387596694926,0.239586152471997,31.6452749139184));
#7806=CARTESIAN_POINT('Ctrl Pts',(-2.43086623907027,0.319933783456974,31.6410926055412));
#7807=CARTESIAN_POINT('Ctrl Pts',(-2.41899343344879,0.399935061913178,31.6369102971641));
#7808=CARTESIAN_POINT('Ctrl Pts',(-2.40319591535467,0.47916556890352,31.6327279887869));
#7809=CARTESIAN_POINT('Ctrl Pts',(-2.3874004824536,0.558385617864842,31.6285462324535));
#7810=CARTESIAN_POINT('Ctrl Pts',(-2.36768145903392,0.636834633535598,31.62436447612));
#7811=CARTESIAN_POINT('Ctrl Pts',(-2.34414471162675,0.714097907119433,31.6201827197866));
#7812=CARTESIAN_POINT('Ctrl Pts',(-2.32060357007508,0.79137560521073,31.6160001827488));
#7813=CARTESIAN_POINT('Ctrl Pts',(-2.29324342983352,0.867466669907059,31.6118176457109));
#7814=CARTESIAN_POINT('Ctrl Pts',(-2.26221968959458,0.941972571793139,31.6076351086731));
#7815=CARTESIAN_POINT('Ctrl Pts',(-2.23116118125689,1.01656197194651,31.6034478842939));
#7816=CARTESIAN_POINT('Ctrl Pts',(-2.19643106527826,1.08956222842802,31.5992606599147));
#7817=CARTESIAN_POINT('Ctrl Pts',(-2.15823215230338,1.16059649610187,31.5950734355355));
#7818=CARTESIAN_POINT('Ctrl Pts',(-2.1200075469549,1.23167854102383,31.5908833948528));
#7819=CARTESIAN_POINT('Ctrl Pts',(-2.07830974907221,1.30079156321528,31.5866933541701));
#7820=CARTESIAN_POINT('Ctrl Pts',(-2.0333852848379,1.36758712095598,31.5825033134874));
#7821=CARTESIAN_POINT('Ctrl Pts',(-1.98838819435972,1.43449066241,31.5783064990585));
#7822=CARTESIAN_POINT('Ctrl Pts',(-1.94015431715274,1.49906889049477,31.5741096846297));
#7823=CARTESIAN_POINT('Ctrl Pts',(-1.88897035835881,1.56100648148616,31.5699128702008));
#7824=CARTESIAN_POINT('Ctrl Pts',(-1.87626709970697,1.57637866560742,31.5688712700499));
#7825=CARTESIAN_POINT('Ctrl Pts',(-1.8633822975951,1.59158837468609,31.567829669899));
#7826=CARTESIAN_POINT('Ctrl Pts',(-1.85032066881284,1.60663115635295,31.5667880697481));
#7827=CARTESIAN_POINT('Ctrl Pts',(-1.79726781722405,1.66773092243555,31.5625573678087));
#7828=CARTESIAN_POINT('Ctrl Pts',(-1.74108556238763,1.72631496655015,31.5583266658693));
#7829=CARTESIAN_POINT('Ctrl Pts',(-1.68204176569144,1.78204538339225,31.55409596393));
#7830=CARTESIAN_POINT('Ctrl Pts',(-1.62308279868498,1.83769573095977,31.5498713403452));
#7831=CARTESIAN_POINT('Ctrl Pts',(-1.56127079031439,1.89050027732401,31.5456467167604));
#7832=CARTESIAN_POINT('Ctrl Pts',(-1.49691297561613,1.94015509520039,31.5414220931756));
#7833=CARTESIAN_POINT('Ctrl Pts',(-1.43230186127517,1.99000534462905,31.5371808423071));
#7834=CARTESIAN_POINT('Ctrl Pts',(-1.36512516917725,2.03668066064791,31.5329395914386));
#7835=CARTESIAN_POINT('Ctrl Pts',(-1.2957302547892,2.07991186275378,31.5286983405701));
#7836=CARTESIAN_POINT('Ctrl Pts',(-1.22673214232098,2.12289586772506,31.524481341284));
#7837=CARTESIAN_POINT('Ctrl Pts',(-1.15554150512805,2.16247479059063,31.5202643419979));
#7838=CARTESIAN_POINT('Ctrl Pts',(-1.08253035737813,2.19842631792716,31.5160473427118));
#7839=CARTESIAN_POINT('Ctrl Pts',(-1.00954341442107,2.23436592654581,31.5118317414533));
#7840=CARTESIAN_POINT('Ctrl Pts',(-0.934737576323989,2.26668032243558,31.5076161401948));
#7841=CARTESIAN_POINT('Ctrl Pts',(-0.858509105248948,2.29519331782851,31.5034005389362));
#7842=CARTESIAN_POINT('Ctrl Pts',(-0.782282536270929,2.32370560174864,31.4991850428678));
#7843=CARTESIAN_POINT('Ctrl Pts',(-0.704633840860683,2.34841651185339,31.4949695467994));
#7844=CARTESIAN_POINT('Ctrl Pts',(-0.625977535286773,2.36919867789012,31.490754050731));
#7845=CARTESIAN_POINT('Ctrl Pts',(-0.546487761341621,2.39020105866935,31.4864938858643));
#7846=CARTESIAN_POINT('Ctrl Pts',(-0.465969360420621,2.40719079973597,31.4822337209977));
#7847=CARTESIAN_POINT('Ctrl Pts',(-0.38486218130251,2.42008912054971,31.4779735561311));
#7848=CARTESIAN_POINT('Ctrl Pts',(-0.304488550124137,2.43287078662632,31.473751920963));
#7849=CARTESIAN_POINT('Ctrl Pts',(-0.223537222083068,2.44163475260481,31.4695302857949));
#7850=CARTESIAN_POINT('Ctrl Pts',(-0.142440930413526,2.44635664434745,31.4653086506268));
#7851=CARTESIAN_POINT('Ctrl Pts',(-0.0602344235502362,2.45114317919335,
31.4610292209109));
#7852=CARTESIAN_POINT('Ctrl Pts',(0.0221205514846858,2.45177612534295,31.456749791195));
#7853=CARTESIAN_POINT('Ctrl Pts',(0.104175698326536,2.44828463906429,31.4524703614791));
#7854=CARTESIAN_POINT('Ctrl Pts',(0.186230845168385,2.44479315278564,31.4481909317632));
#7855=CARTESIAN_POINT('Ctrl Pts',(0.267985681418831,2.43717734479116,31.4439115020473));
#7856=CARTESIAN_POINT('Ctrl Pts',(0.349001701606388,2.42552016323836,31.4396320723314));
#7857=CARTESIAN_POINT('Ctrl Pts',(0.42909523193789,2.41399571631889,31.4354013703917));
#7858=CARTESIAN_POINT('Ctrl Pts',(0.508767946089545,2.39847815840009,31.431170668452));
#7859=CARTESIAN_POINT('Ctrl Pts',(0.587590724305905,2.37900975002409,31.4269399665123));
#7860=CARTESIAN_POINT('Ctrl Pts',(0.666300255878092,2.35956931239418,31.4227153429273));
#7861=CARTESIAN_POINT('Ctrl Pts',(0.744161829072512,2.33618940828933,31.4184907193422));
#7862=CARTESIAN_POINT('Ctrl Pts',(0.820753574049774,2.30896379804546,31.4142660957571));
#7863=CARTESIAN_POINT('Ctrl Pts',(0.897646768995757,2.28163103318122,31.4100248448887));
#7864=CARTESIAN_POINT('Ctrl Pts',(0.973259648983094,2.25042229295735,31.4057835940203));
#7865=CARTESIAN_POINT('Ctrl Pts',(1.04717783611404,2.21548388158242,31.4015423431518));
#7866=CARTESIAN_POINT('Ctrl Pts',(1.1206733571401,2.18074524894693,31.3973253438655));
#7867=CARTESIAN_POINT('Ctrl Pts',(1.1924930886288,2.1423196828641,31.3931083445792));
#7868=CARTESIAN_POINT('Ctrl Pts',(1.26224870601945,2.10039959392308,31.3888913452929));
#7869=CARTESIAN_POINT('Ctrl Pts',(1.33198119789673,2.05849340240872,31.3846757440341));
#7870=CARTESIAN_POINT('Ctrl Pts',(1.39965053627575,2.01309522800402,31.3804601427753));
#7871=CARTESIAN_POINT('Ctrl Pts',(1.46489404893623,1.96444284095802,31.3762445415165));
#7872=CARTESIAN_POINT('Ctrl Pts',(1.53013593360256,1.91579166791474,31.3720290454478));
#7873=CARTESIAN_POINT('Ctrl Pts',(1.59295174073313,1.86388672255796,31.3678135493791));
#7874=CARTESIAN_POINT('Ctrl Pts',(1.65300995881143,1.80900755279524,31.3635980533105));
#7875=CARTESIAN_POINT('Ctrl Pts',(1.71370457373299,1.75354686510682,31.3593378884442));
#7876=CARTESIAN_POINT('Ctrl Pts',(1.77158244245977,1.69504886087445,31.3550777235778));
#7877=CARTESIAN_POINT('Ctrl Pts',(1.82633919032043,1.63384069354993,31.3508175587115));
#7878=CARTESIAN_POINT('Ctrl Pts',(1.8806007082956,1.57318610390998,31.3465959235432));
#7879=CARTESIAN_POINT('Ctrl Pts',(1.93179708661286,1.50987058085758,31.3423742883749));
#7880=CARTESIAN_POINT('Ctrl Pts',(1.9796735456331,1.44424475166797,31.3381526532066));
#7881=CARTESIAN_POINT('Ctrl Pts',(2.02820543747765,1.3777204992563,31.3338732234913));
#7882=CARTESIAN_POINT('Ctrl Pts',(2.07332555080609,1.30882261898734,31.329593793776));
#7883=CARTESIAN_POINT('Ctrl Pts',(2.11481568600755,1.23794380495094,31.3253143640606));
#7884=CARTESIAN_POINT('Ctrl Pts',(2.15630582120902,1.16706499091454,31.3210349343453));
#7885=CARTESIAN_POINT('Ctrl Pts',(2.19416581018964,1.09420570863176,31.31675550463));
#7886=CARTESIAN_POINT('Ctrl Pts',(2.22822798017986,1.01977954399154,31.3124760749147));
#7887=CARTESIAN_POINT('Ctrl Pts',(2.26190230088916,0.946200833710374,31.3082453729738));
#7888=CARTESIAN_POINT('Ctrl Pts',(2.2919915486179,0.870814010198756,31.304014671033));
#7889=CARTESIAN_POINT('Ctrl Pts',(2.31829892371577,0.794002739477832,31.2997839690922));
#7890=CARTESIAN_POINT('Ctrl Pts',(2.34456850235438,0.717301825417503,31.2955593455059));
#7891=CARTESIAN_POINT('Ctrl Pts',(2.36706685020385,0.639180964924323,31.2913347219196));
#7892=CARTESIAN_POINT('Ctrl Pts',(2.38564439164342,0.56004561119637,31.2871100983334));
#7893=CARTESIAN_POINT('Ctrl Pts',(2.40429505060736,0.480598796386542,31.2828688474652));
#7894=CARTESIAN_POINT('Ctrl Pts',(2.41899377644315,0.400129917034853,31.2786275965971));
#7895=CARTESIAN_POINT('Ctrl Pts',(2.42963922641231,0.319066575307708,31.2743863457289));
#7896=CARTESIAN_POINT('Ctrl Pts',(2.44022380542717,0.238466755835059,31.2701693464414));
#7897=CARTESIAN_POINT('Ctrl Pts',(2.44680127509927,0.157279719577928,31.2659523471538));
#7898=CARTESIAN_POINT('Ctrl Pts',(2.44932316256167,0.0759361267046567,31.2617353478663));
#7899=CARTESIAN_POINT('Ctrl Pts',(2.45184421396321,-0.00538049898817242,
31.2575197466062));
#7900=CARTESIAN_POINT('Ctrl Pts',(2.45031233873219,-0.0868531137599519,
31.2533041453462));
#7901=CARTESIAN_POINT('Ctrl Pts',(2.44473108895797,-0.168048066583332,31.2490885440861));
#7902=CARTESIAN_POINT('Ctrl Pts',(2.43914997845033,-0.249240993383016,31.2448730480162));
#7903=CARTESIAN_POINT('Ctrl Pts',(2.42951972727157,-0.330155808118384,31.2406575519463));
#7904=CARTESIAN_POINT('Ctrl Pts',(2.41589588316585,-0.410362439438967,31.2364420558764));
#7905=CARTESIAN_POINT('Ctrl Pts',(2.40212767628792,-0.491418966835655,31.2321818910115));
#7906=CARTESIAN_POINT('Ctrl Pts',(2.38428080292077,-0.571751732836788,31.2279217261466));
#7907=CARTESIAN_POINT('Ctrl Pts',(2.36246552773728,-0.650927707393862,31.2236615612818));
#7908=CARTESIAN_POINT('Ctrl Pts',(2.3408475538161,-0.729387600233239,31.2194399261122));
#7909=CARTESIAN_POINT('Ctrl Pts',(2.3153328771864,-0.806711114717247,31.2152182909426));
#7910=CARTESIAN_POINT('Ctrl Pts',(2.28607834965286,-0.882494209186918,31.210996655773));
#7911=CARTESIAN_POINT('Ctrl Pts',(2.25642332516027,-0.959314780636797,31.2067172260605));
#7912=CARTESIAN_POINT('Ctrl Pts',(2.22292547788918,-1.03455198387522,31.202437796348));
#7913=CARTESIAN_POINT('Ctrl Pts',(2.18579683249517,-1.10780975670649,31.1981583666355));
#7914=CARTESIAN_POINT('Ctrl Pts',(2.14866818710117,-1.18106752953774,31.193878936923));
#7915=CARTESIAN_POINT('Ctrl Pts',(2.10790904396655,-1.25234547859705,31.1895995072104));
#7916=CARTESIAN_POINT('Ctrl Pts',(2.06377634851442,-1.32127871144301,31.1853200774979));
#7917=CARTESIAN_POINT('Ctrl Pts',(2.02014617047353,-1.38942703529204,31.1810893755578));
#7918=CARTESIAN_POINT('Ctrl Pts',(1.97305480665064,-1.45554011598604,31.1768586736177));
#7919=CARTESIAN_POINT('Ctrl Pts',(1.92271827747711,-1.51924477140962,31.1726279716777));
#7920=CARTESIAN_POINT('Ctrl Pts',(1.87245406804555,-1.58285790077212,31.1684033480921));
#7921=CARTESIAN_POINT('Ctrl Pts',(1.81895423894421,-1.64406911529902,31.1641787245067));
#7922=CARTESIAN_POINT('Ctrl Pts',(1.7624786959864,-1.70253314099728,31.1599541009211));
#7923=CARTESIAN_POINT('Ctrl Pts',(1.70578087646207,-1.76122726953682,31.1557128500528));
#7924=CARTESIAN_POINT('Ctrl Pts',(1.64608412507255,-1.81715213841931,31.1514715991845));
#7925=CARTESIAN_POINT('Ctrl Pts',(1.58369308339694,-1.86999103409634,31.1472303483161));
#7926=CARTESIAN_POINT('Ctrl Pts',(1.52165879530242,-1.92252779560879,31.1430133490294));
#7927=CARTESIAN_POINT('Ctrl Pts',(1.45696130381112,-1.97201347592064,31.1387963497426));
#7928=CARTESIAN_POINT('Ctrl Pts',(1.38993644591489,-2.01817415658745,31.1345793504558));
#7929=CARTESIAN_POINT('Ctrl Pts',(1.32293380822533,-2.06431953397878,31.1303637491966));
#7930=CARTESIAN_POINT('Ctrl Pts',(1.25360571905293,-2.10714183715016,31.1261481479373));
#7931=CARTESIAN_POINT('Ctrl Pts',(1.18231869690441,-2.14640926874403,31.121932546678));
#7932=CARTESIAN_POINT('Ctrl Pts',(1.11103345355109,-2.18567572051412,31.1177170506089));
#7933=CARTESIAN_POINT('Ctrl Pts',(1.03778978228109,-2.22138725363831,31.1135015545398));
#7934=CARTESIAN_POINT('Ctrl Pts',(0.96297934302438,-2.25335772457644,31.1092860584707));
#7935=CARTESIAN_POINT('Ctrl Pts',(0.887376187502514,-2.2856669652447,31.1050258936049));
#7936=CARTESIAN_POINT('Ctrl Pts',(0.810173301462727,-2.31415518338303,31.1007657287391));
#7937=CARTESIAN_POINT('Ctrl Pts',(0.731794456776513,-2.33868063724639,31.0965055638733));
#7938=CARTESIAN_POINT('Ctrl Pts',(0.654124484453692,-2.36298427849548,31.0922839287045));
#7939=CARTESIAN_POINT('Ctrl Pts',(0.575300209773864,-2.3833964889251,31.0880622935357));
#7940=CARTESIAN_POINT('Ctrl Pts',(0.495746255226477,-2.39983038992945,31.0838406583669));
#7941=CARTESIAN_POINT('Ctrl Pts',(0.415103200256682,-2.41648927244009,31.0795612286526));
#7942=CARTESIAN_POINT('Ctrl Pts',(0.333710824245474,-2.4290600184796,31.0752817989383));
#7943=CARTESIAN_POINT('Ctrl Pts',(0.252016912124409,-2.43750645660751,31.071002369224));
#7944=CARTESIAN_POINT('Ctrl Pts',(0.170323000003344,-2.44595289473541,31.0667229395097));
#7945=CARTESIAN_POINT('Ctrl Pts',(0.0883280451273653,-2.45027506452806,
31.0624435097955));
#7946=CARTESIAN_POINT('Ctrl Pts',(0.00647794685830275,-2.45049143769255,
31.0581640800812));
#7947=CARTESIAN_POINT('Ctrl Pts',(-0.074440164355392,-2.45070534712159,
31.053933378141));
#7948=CARTESIAN_POINT('Ctrl Pts',(-0.155521056560431,-2.44690733381109,
31.0497026762008));
#7949=CARTESIAN_POINT('Ctrl Pts',(-0.236334018065208,-2.43907697334569,
31.0454719742606));
#7950=CARTESIAN_POINT('Ctrl Pts',(-0.317030873580547,-2.43125786295369,
31.041247350675));
#7951=CARTESIAN_POINT('Ctrl Pts',(-0.397460103947968,-2.41941795583632,
31.0370227270894));
#7952=CARTESIAN_POINT('Ctrl Pts',(-0.477190701374035,-2.40358883433131,
31.0327981035038));
#7953=CARTESIAN_POINT('Ctrl Pts',(-0.557235102658854,-2.38769741253546,
31.0285568526355));
#7954=CARTESIAN_POINT('Ctrl Pts',(-0.636574885292314,-2.36778530622874,
31.0243156017671));
#7955=CARTESIAN_POINT('Ctrl Pts',(-0.714778833416086,-2.34393717264357,
31.0200743508988));
#7956=CARTESIAN_POINT('Ctrl Pts',(-0.792535609355393,-2.32022540329891,
31.015857351612));
#7957=CARTESIAN_POINT('Ctrl Pts',(-0.8691690556904,-2.2926226341564,31.0116403523251));
#7958=CARTESIAN_POINT('Ctrl Pts',(-0.944267047302358,-2.26126292000264,
31.0074233530382));
#7959=CARTESIAN_POINT('Ctrl Pts',(-1.01934014228714,-2.22991360228021,31.0032077517788));
#7960=CARTESIAN_POINT('Ctrl Pts',(-1.09287836460301,-2.19480999197966,30.9989921505195));
#7961=CARTESIAN_POINT('Ctrl Pts',(-1.16448839141628,-2.15613474445748,30.9947765492601));
#7962=CARTESIAN_POINT('Ctrl Pts',(-1.23609663137431,-2.11746046198268,30.9905610531909));
#7963=CARTESIAN_POINT('Ctrl Pts',(-1.30577636281149,-2.07521494143544,30.9863455571217));
#7964=CARTESIAN_POINT('Ctrl Pts',(-1.37315903482018,-2.02962669353054,30.9821300610525));
#7965=CARTESIAN_POINT('Ctrl Pts',(-1.44125571600152,-1.98355537740946,30.9778698961868));
#7966=CARTESIAN_POINT('Ctrl Pts',(-1.50700595679883,-1.93407032895756,30.9736097313212));
#7967=CARTESIAN_POINT('Ctrl Pts',(-1.57006115166227,-1.88145109690392,30.9693495664555));
#7968=CARTESIAN_POINT('Ctrl Pts',(-1.6325460640095,-1.82930776264301,30.9651279312866));
#7969=CARTESIAN_POINT('Ctrl Pts',(-1.69238417959032,-1.77408707324614,30.9609062961177));
#7970=CARTESIAN_POINT('Ctrl Pts',(-1.74927255891719,-1.7160989961594,30.9566846609488));
#7971=CARTESIAN_POINT('Ctrl Pts',(-1.80693974500443,-1.65731705735625,30.9524052312348));
#7972=CARTESIAN_POINT('Ctrl Pts',(-1.86157549088736,-1.59569175573528,30.9481258015207));
#7973=CARTESIAN_POINT('Ctrl Pts',(-1.9129069490887,-1.53157998619992,30.9438463718067));
#7974=CARTESIAN_POINT('Ctrl Pts',(-1.96423840729007,-1.46746821666454,30.9395669420926));
#7975=CARTESIAN_POINT('Ctrl Pts',(-2.01226534397574,-1.40087041543376,30.9352875123785));
#7976=CARTESIAN_POINT('Ctrl Pts',(-2.05676187417565,-1.33217147655152,30.9310080826645));
#7977=CARTESIAN_POINT('Ctrl Pts',(-2.10171929271023,-1.26276096444339,30.9266843272642));
#7978=CARTESIAN_POINT('Ctrl Pts',(-2.14323638783552,-1.19095353206572,30.9223605718639));
#7979=CARTESIAN_POINT('Ctrl Pts',(-2.18105535464682,-1.11711583551861,30.9180368164637));
#7980=CARTESIAN_POINT('Ctrl Pts',(-2.21881263121973,-1.04339858290442,30.9137201139663));
#7981=CARTESIAN_POINT('Ctrl Pts',(-2.25288357200986,-0.967658035310448,
30.909403411469));
#7982=CARTESIAN_POINT('Ctrl Pts',(-2.28305401222222,-0.890289069502711,
30.9050867089717));
#7983=CARTESIAN_POINT('Ctrl Pts',(-2.31317310560313,-0.813051777320532,
30.9007773530359));
#7984=CARTESIAN_POINT('Ctrl Pts',(-2.33940475210986,-0.734191988263348,
30.8964679971001));
#7985=CARTESIAN_POINT('Ctrl Pts',(-2.36158169918636,-0.654126996895925,
30.8921586411643));
#7986=CARTESIAN_POINT('Ctrl Pts',(-2.3837364086968,-0.574142289371331,30.8878536063637));
#7987=CARTESIAN_POINT('Ctrl Pts',(-2.40184438315073,-0.49295520152023,30.8835485715631));
#7988=CARTESIAN_POINT('Ctrl Pts',(-2.41578745660414,-0.411000260966004,
30.8792435367625));
#7989=CARTESIAN_POINT('Ctrl Pts',(-2.42971883039785,-0.329114088959626,
30.8749421143249));
#7990=CARTESIAN_POINT('Ctrl Pts',(-2.43949218192722,-0.246461776575417,
30.8706406918873));
#7991=CARTESIAN_POINT('Ctrl Pts',(-2.44504020385128,-0.163488995198076,
30.8663392694497));
#7992=CARTESIAN_POINT('Ctrl Pts',(-2.44869973006771,-0.108759386545377,
30.8635020117038));
#7993=CARTESIAN_POINT('Ctrl Pts',(-2.4505219261096,-0.0538905871457517,
30.8606647539579));
#7994=CARTESIAN_POINT('Ctrl Pts',(-2.4504998008426,0.000987962737408825,
30.857827496212));
#7995=CARTESIAN_POINT('',(-2.45288797253939,0.00174278626405643,30.057827496212));
#7996=CARTESIAN_POINT('Ctrl Pts',(-2.44683799040888,0.00100022143846595,
30.8578267850394));
#7997=CARTESIAN_POINT('Ctrl Pts',(-2.44809241697276,0.348475602492684,30.8398352184422));
#7998=CARTESIAN_POINT('Ctrl Pts',(-2.21640111872538,1.51294853004426,30.7794583193726));
#7999=CARTESIAN_POINT('Ctrl Pts',(-0.427813795401416,2.86569388547629,30.676696087831));
#8000=CARTESIAN_POINT('Ctrl Pts',(2.17773023598689,1.91120828484089,30.5495400904143));
#8001=CARTESIAN_POINT('Ctrl Pts',(2.78591169168837,-0.796192272567481,30.4223840929975));
#8002=CARTESIAN_POINT('Ctrl Pts',(0.838920950119278,-2.77334414168751,30.2952280955807));
#8003=CARTESIAN_POINT('Ctrl Pts',(-1.75708235892424,-2.23196450228063,30.1737092299857));
#8004=CARTESIAN_POINT('Ctrl Pts',(-2.44721005689546,-0.703532279603159,
30.0945756968627));
#8005=CARTESIAN_POINT('Ctrl Pts',(-2.45288797253939,0.00174278626405643,
30.057827496212));
#8006=CARTESIAN_POINT('',(-2.45231819670878,-0.0019531457292471,29.257827496212));
#8007=CARTESIAN_POINT('Ctrl Pts',(-2.45288797253939,0.00174278626405643,
30.057827496212));
#8008=CARTESIAN_POINT('Ctrl Pts',(-2.45375895828535,0.109931172263209,30.0521903643904));
#8009=CARTESIAN_POINT('Ctrl Pts',(-2.39807262124372,1.0306806169693,30.0041679000973));
#8010=CARTESIAN_POINT('Ctrl Pts',(-1.23228707159884,2.62234525986871,29.9137601033299));
#8011=CARTESIAN_POINT('Ctrl Pts',(1.53758168640185,2.45582341515417,29.7866041059142));
#8012=CARTESIAN_POINT('Ctrl Pts',(2.89721695141521,0.0368785196587262,29.6594481084969));
#8013=CARTESIAN_POINT('Ctrl Pts',(1.59959347208367,-2.41589048030868,29.5322921110805));
#8014=CARTESIAN_POINT('Ctrl Pts',(-1.16513924082463,-2.65286197120667,29.4051361136636));
#8015=CARTESIAN_POINT('Ctrl Pts',(-2.38547217171649,-1.07272642830989,29.3136479087075));
#8016=CARTESIAN_POINT('Ctrl Pts',(-2.45344099196259,-0.130954814691625,
29.2645450362236));
#8017=CARTESIAN_POINT('Ctrl Pts',(-2.45231819670878,-0.0019531457292471,
29.257827496212));
#8018=CARTESIAN_POINT('',(-2.44662742701941,-0.000665902842327259,28.4578274962121));
#8019=CARTESIAN_POINT('Ctrl Pts',(-2.45231819670878,-0.0019531457292471,
29.257827496212));
#8020=CARTESIAN_POINT('Ctrl Pts',(-2.4463565458635,0.683000683748745,29.2221597037514));
#8021=CARTESIAN_POINT('Ctrl Pts',(-1.79037424641765,2.19191624501729,29.1441065788186));
#8022=CARTESIAN_POINT('Ctrl Pts',(0.768057079194582,2.79379927909598,29.0236681214135));
#8023=CARTESIAN_POINT('Ctrl Pts',(2.76474296314598,0.866846258871282,28.8965121239966));
#8024=CARTESIAN_POINT('Ctrl Pts',(2.22567210609608,-1.85515761188246,28.76935612658));
#8025=CARTESIAN_POINT('Ctrl Pts',(-0.354732474020897,-2.87565487509438,
28.6422001291633));
#8026=CARTESIAN_POINT('Ctrl Pts',(-2.19633750317876,-1.55513202065881,28.5383572523739));
#8027=CARTESIAN_POINT('Ctrl Pts',(-2.44752200009088,-0.369091194471079,
28.4768997080569));
#8028=CARTESIAN_POINT('Ctrl Pts',(-2.44662742701941,-0.000665902842327259,
28.4578274962121));
#8029=CARTESIAN_POINT('',(-2.45049897433075,0.00224205350688658,27.6578274763058));
#8030=CARTESIAN_POINT('Ctrl Pts',(-2.44662742701941,-0.000665902842327259,
28.4578274962121));
#8031=CARTESIAN_POINT('Ctrl Pts',(-2.44553393612832,0.449682663744117,28.4345143755846));
#8032=CARTESIAN_POINT('Ctrl Pts',(-2.11046025923188,1.72031868191387,28.368815922485));
#8033=CARTESIAN_POINT('Ctrl Pts',(-0.0660938160396643,2.89669772262467,
28.2607321369129));
#8034=CARTESIAN_POINT('Ctrl Pts',(2.39963642723916,1.62387533568544,28.1335761394963));
#8035=CARTESIAN_POINT('Ctrl Pts',(2.66447699381769,-1.13832703481685,28.0064201420796));
#8036=CARTESIAN_POINT('Ctrl Pts',(0.485522390872327,-2.8564828192631,27.8792641446627));
#8037=CARTESIAN_POINT('Ctrl Pts',(-1.91257976242076,-2.03245344355806,27.7630665960403));
#8038=CARTESIAN_POINT('Ctrl Pts',(-2.44444423210955,-0.60282188315779,27.68925437989));
#8039=CARTESIAN_POINT('Ctrl Pts',(-2.44987016120039,0.00224109493129301,
27.657827496212));
#8040=CARTESIAN_POINT('',(-2.45083979799343,-0.000495560851292726,26.8578274467331));
#8041=CARTESIAN_POINT('Ctrl Pts',(-2.45049897433075,0.00224205350688658,
27.6578274763058));
#8042=CARTESIAN_POINT('Ctrl Pts',(-2.45040243215944,0.107759825969181,27.6523482552264));
#8043=CARTESIAN_POINT('Ctrl Pts',(-2.44348655931152,0.21297287842917,27.646869034147));
#8044=CARTESIAN_POINT('Ctrl Pts',(-2.42989259424758,0.317131251094503,27.6413898130676));
#8045=CARTESIAN_POINT('Ctrl Pts',(-2.41629862918364,0.421289623759814,27.6359105919881));
#8046=CARTESIAN_POINT('Ctrl Pts',(-2.39602674806883,0.524393675050337,27.6304313709087));
#8047=CARTESIAN_POINT('Ctrl Pts',(-2.36926728014889,0.625717831946559,27.6249521498292));
#8048=CARTESIAN_POINT('Ctrl Pts',(-2.34860534094122,0.703953825887892,27.620721447889));
#8049=CARTESIAN_POINT('Ctrl Pts',(-2.32402521275331,0.781312427764519,27.6164907459487));
#8050=CARTESIAN_POINT('Ctrl Pts',(-2.2956182417327,0.857372228512266,27.6122600440085));
#8051=CARTESIAN_POINT('Ctrl Pts',(-2.26725208371305,0.93332275225474,27.6080354204228));
#8052=CARTESIAN_POINT('Ctrl Pts',(-2.23507016376297,1.00797774891626,27.6038107968372));
#8053=CARTESIAN_POINT('Ctrl Pts',(-2.19921415187152,1.08092893578072,27.5995861732515));
#8054=CARTESIAN_POINT('Ctrl Pts',(-2.16321701781103,1.15416724408399,27.5953449223832));
#8055=CARTESIAN_POINT('Ctrl Pts',(-2.1235169299542,1.22568784328453,27.5911036715149));
#8056=CARTESIAN_POINT('Ctrl Pts',(-2.0803068914358,1.29509593754467,27.5868624206466));
#8057=CARTESIAN_POINT('Ctrl Pts',(-2.03734392902704,1.36410715453983,27.5826454213597));
#8058=CARTESIAN_POINT('Ctrl Pts',(-1.99091129526616,1.43102956097969,27.5784284220728));
#8059=CARTESIAN_POINT('Ctrl Pts',(-1.94124479636811,1.49549954549433,27.5742114227858));
#8060=CARTESIAN_POINT('Ctrl Pts',(-1.89159476300097,1.55994815679872,27.5699958215264));
#8061=CARTESIAN_POINT('Ctrl Pts',(-1.83871327709317,1.62194559259938,27.565780220267));
#8062=CARTESIAN_POINT('Ctrl Pts',(-1.78287825230751,1.68115894175683,27.5615646190076));
#8063=CARTESIAN_POINT('Ctrl Pts',(-1.72704462074996,1.74037081338824,27.5573491229383));
#8064=CARTESIAN_POINT('Ctrl Pts',(-1.66825791668813,1.79679839888665,27.553133626869));
#8065=CARTESIAN_POINT('Ctrl Pts',(-1.60683396932768,1.85014454705967,27.5489181307998));
#8066=CARTESIAN_POINT('Ctrl Pts',(-1.54475915342195,1.90405596873513,27.5446579659342));
#8067=CARTESIAN_POINT('Ctrl Pts',(-1.47999122643444,1.95481993054553,27.5403978010686));
#8068=CARTESIAN_POINT('Ctrl Pts',(-1.41289018521353,2.0021717145458,27.536137636203));
#8069=CARTESIAN_POINT('Ctrl Pts',(-1.34639601786848,2.04909524050176,27.531916001034));
#8070=CARTESIAN_POINT('Ctrl Pts',(-1.27761119901213,2.09266786159333,27.5276943658651));
#8071=CARTESIAN_POINT('Ctrl Pts',(-1.20691333802824,2.13267682607786,27.5234727306962));
#8072=CARTESIAN_POINT('Ctrl Pts',(-1.13524761730665,2.17323351669346,27.5191933009822));
#8073=CARTESIAN_POINT('Ctrl Pts',(-1.06161652068226,2.21012801679181,27.5149138712683));
#8074=CARTESIAN_POINT('Ctrl Pts',(-0.986435236875301,2.24318875118675,27.5106344415544));
#8075=CARTESIAN_POINT('Ctrl Pts',(-0.911253953068366,2.27624948558168,27.5063550118404));
#8076=CARTESIAN_POINT('Ctrl Pts',(-0.834522963846833,2.30547634084916,27.5020755821265));
#8077=CARTESIAN_POINT('Ctrl Pts',(-0.756672398388362,2.3307503365906,27.4977961524126));
#8078=CARTESIAN_POINT('Ctrl Pts',(-0.679708279253032,2.35573654970048,27.4935654504723));
#8079=CARTESIAN_POINT('Ctrl Pts',(-0.601360480166206,2.37695348549076,27.4893347485321));
#8080=CARTESIAN_POINT('Ctrl Pts',(-0.522032759855261,2.39424978806262,27.4851040465919));
#8081=CARTESIAN_POINT('Ctrl Pts',(-0.442819011650787,2.41152124060689,27.4808794230062));
#8082=CARTESIAN_POINT('Ctrl Pts',(-0.362628588873525,2.42488314889302,27.4766547994205));
#8083=CARTESIAN_POINT('Ctrl Pts',(-0.281881460098939,2.43423357393092,27.4724301758349));
#8084=CARTESIAN_POINT('Ctrl Pts',(-0.20081652660081,2.44362080039184,27.4681889249666));
#8085=CARTESIAN_POINT('Ctrl Pts',(-0.119190946900974,2.4489647525341,27.4639476740983));
#8086=CARTESIAN_POINT('Ctrl Pts',(-0.0374411427535714,2.4502139520518,27.45970642323));
#8087=CARTESIAN_POINT('Ctrl Pts',(0.0438412139151539,2.45145600861459,27.455489423943));
#8088=CARTESIAN_POINT('Ctrl Pts',(0.125245908568656,2.44865000610601,27.4512724246561));
#8089=CARTESIAN_POINT('Ctrl Pts',(0.206339563933992,2.44179733687207,27.4470554253691));
#8090=CARTESIAN_POINT('Ctrl Pts',(0.287406334978518,2.43494693944789,27.4428398241097));
#8091=CARTESIAN_POINT('Ctrl Pts',(0.368161808464795,2.42405257853439,27.4386242228503));
#8092=CARTESIAN_POINT('Ctrl Pts',(0.44817562109846,2.40916767009957,27.4344086215908));
#8093=CARTESIAN_POINT('Ctrl Pts',(0.528187437180859,2.39428313308167,27.4301931255215));
#8094=CARTESIAN_POINT('Ctrl Pts',(0.607457172187924,2.37540833264341,27.4259776294522));
#8095=CARTESIAN_POINT('Ctrl Pts',(0.685564000345778,2.35264792338971,27.421762133383));
#8096=CARTESIAN_POINT('Ctrl Pts',(0.764498474393691,2.32964633728093,27.4175019685174));
#8097=CARTESIAN_POINT('Ctrl Pts',(0.84224478012513,2.30267642571266,27.4132418036518));
#8098=CARTESIAN_POINT('Ctrl Pts',(0.918385447377913,2.27189753731203,27.4089816387862));
#8099=CARTESIAN_POINT('Ctrl Pts',(0.993837484752943,2.24139701870932,27.4047600036172));
#8100=CARTESIAN_POINT('Ctrl Pts',(1.06771240951862,2.20715639802593,27.4005383684483));
#8101=CARTESIAN_POINT('Ctrl Pts',(1.13962690685303,2.1693779668782,27.3963167332793));
#8102=CARTESIAN_POINT('Ctrl Pts',(1.21252591977968,2.13108234579111,27.3920373035654));
#8103=CARTESIAN_POINT('Ctrl Pts',(1.28340999627475,2.08915156679824,27.3877578738515));
#8104=CARTESIAN_POINT('Ctrl Pts',(1.35191009511807,2.04384181010123,27.3834784441376));
#8105=CARTESIAN_POINT('Ctrl Pts',(1.42041019396138,1.99853205340422,27.3791990144237));
#8106=CARTESIAN_POINT('Ctrl Pts',(1.48652595895594,1.949843662644,27.3749195847098));
#8107=CARTESIAN_POINT('Ctrl Pts',(1.54992447940426,1.89807385476526,27.3706401549958));
#8108=CARTESIAN_POINT('Ctrl Pts',(1.61260111190016,1.84689352437498,27.3664094530556));
#8109=CARTESIAN_POINT('Ctrl Pts',(1.67285783685067,1.79250912326261,27.3621787511153));
#8110=CARTESIAN_POINT('Ctrl Pts',(1.7303488008871,1.73517816873904,27.3579480491751));
#8111=CARTESIAN_POINT('Ctrl Pts',(1.7877571662273,1.67792958302206,27.3537234255894));
#8112=CARTESIAN_POINT('Ctrl Pts',(1.84240733600468,1.61774317723485,27.3494988020037));
#8113=CARTESIAN_POINT('Ctrl Pts',(1.89398622828456,1.55491685213983,27.345274178418));
#8114=CARTESIAN_POINT('Ctrl Pts',(1.94576812487976,1.49184325505919,27.3410329275497));
#8115=CARTESIAN_POINT('Ctrl Pts',(1.99445414866917,1.42610921385212,27.3367916766814));
#8116=CARTESIAN_POINT('Ctrl Pts',(2.03976473497208,1.358053782427,27.3325504258131));
#8117=CARTESIAN_POINT('Ctrl Pts',(2.08481623417947,1.29038749370562,27.3283334265262));
#8118=CARTESIAN_POINT('Ctrl Pts',(2.12653053250318,1.2204266812668,27.3241164272392));
#8119=CARTESIAN_POINT('Ctrl Pts',(2.16467416497904,1.1485364641457,27.3198994279523));
#8120=CARTESIAN_POINT('Ctrl Pts',(2.20280515200626,1.07667008020431,27.3156838266928));
#8121=CARTESIAN_POINT('Ctrl Pts',(2.23736760612117,1.00287597228716,27.3114682254334));
#8122=CARTESIAN_POINT('Ctrl Pts',(2.26817343341489,0.927544891609505,27.3072526241739));
#8123=CARTESIAN_POINT('Ctrl Pts',(2.29897849202367,0.852215690636856,27.3030371281046));
#8124=CARTESIAN_POINT('Ctrl Pts',(2.3260269351577,0.775350024024735,27.2988216320353));
#8125=CARTESIAN_POINT('Ctrl Pts',(2.34917891190414,0.697358365451296,27.294606135966));
#8126=CARTESIAN_POINT('Ctrl Pts',(2.37257621468474,0.618540281363256,27.2903459711004));
#8127=CARTESIAN_POINT('Ctrl Pts',(2.39199382957937,0.538572660311562,27.2860858062349));
#8128=CARTESIAN_POINT('Ctrl Pts',(2.40733970685371,0.457892766710145,27.2818256413693));
#8129=CARTESIAN_POINT('Ctrl Pts',(2.42254679325627,0.377942556564998,27.2776040062003));
#8130=CARTESIAN_POINT('Ctrl Pts',(2.4337554932477,0.297293380137397,27.2733823710314));
#8131=CARTESIAN_POINT('Ctrl Pts',(2.4409283538408,0.216377035325058,27.2691607358624));
#8132=CARTESIAN_POINT('Ctrl Pts',(2.44819941150616,0.134352938862447,27.2648813061485));
#8133=CARTESIAN_POINT('Ctrl Pts',(2.45132327236097,0.0520547978091799,27.2606018764346));
#8134=CARTESIAN_POINT('Ctrl Pts',(2.45031551854859,-0.0300684146565806,
27.2563224467207));
#8135=CARTESIAN_POINT('Ctrl Pts',(2.44930776473621,-0.112191627122318,27.2520430170068));
#8136=CARTESIAN_POINT('Ctrl Pts',(2.44416849232606,-0.194139425473974,27.247763587293));
#8137=CARTESIAN_POINT('Ctrl Pts',(2.43496734690492,-0.275470995763323,27.2434841575791));
#8138=CARTESIAN_POINT('Ctrl Pts',(2.42587097042757,-0.355876483230728,27.2392534556388));
#8139=CARTESIAN_POINT('Ctrl Pts',(2.41277058077393,-0.435982137070138,27.2350227536985));
#8140=CARTESIAN_POINT('Ctrl Pts',(2.39569543844949,-0.515357755537185,27.2307920517583));
#8141=CARTESIAN_POINT('Ctrl Pts',(2.37864482840621,-0.594619333081269,27.2265674281726));
#8142=CARTESIAN_POINT('Ctrl Pts',(2.35763090428507,-0.673152507544719,27.2223428045869));
#8143=CARTESIAN_POINT('Ctrl Pts',(2.33273462212481,-0.750532765933785,27.2181181810012));
#8144=CARTESIAN_POINT('Ctrl Pts',(2.30774035312361,-0.828217577710469,27.213876930133));
#8145=CARTESIAN_POINT('Ctrl Pts',(2.27883315349637,-0.904739907102235,27.2096356792647));
#8146=CARTESIAN_POINT('Ctrl Pts',(2.24614672573727,-0.979681140198043,27.2053944283964));
#8147=CARTESIAN_POINT('Ctrl Pts',(2.21364719981109,-1.05419385739942,27.2011774291094));
#8148=CARTESIAN_POINT('Ctrl Pts',(2.1774117357153,-1.12714308017459,27.1969604298225));
#8149=CARTESIAN_POINT('Ctrl Pts',(2.13762090932816,-1.19813484132757,27.1927434305355));
#8150=CARTESIAN_POINT('Ctrl Pts',(2.09784327447047,-1.26910306715864,27.1885278292761));
#8151=CARTESIAN_POINT('Ctrl Pts',(2.05451284518467,-1.33811471469471,27.1843122280166));
#8152=CARTESIAN_POINT('Ctrl Pts',(2.00785631222409,-1.40480008522988,27.1800966267572));
#8153=CARTESIAN_POINT('Ctrl Pts',(1.96120094346449,-1.47148379179286,27.1758811306879));
#8154=CARTESIAN_POINT('Ctrl Pts',(1.91121990353903,-1.53584095633322,27.1716656346186));
#8155=CARTESIAN_POINT('Ctrl Pts',(1.85818258433968,-1.59753176283187,27.1674501385493));
#8156=CARTESIAN_POINT('Ctrl Pts',(1.80458326409292,-1.65987626560309,27.1631899736837));
#8157=CARTESIAN_POINT('Ctrl Pts',(1.74786281182931,-1.71949718877495,27.1589298088181));
#8158=CARTESIAN_POINT('Ctrl Pts',(1.68833902407782,-1.77608040070711,27.1546696439526));
#8159=CARTESIAN_POINT('Ctrl Pts',(1.6293535801594,-1.83215186390235,27.1504480087836));
#8160=CARTESIAN_POINT('Ctrl Pts',(1.56761570131098,-1.88524008226808,27.1462263736146));
#8161=CARTESIAN_POINT('Ctrl Pts',(1.50346814737254,-1.93507978642644,27.1420047384457));
#8162=CARTESIAN_POINT('Ctrl Pts',(1.43844240795877,-1.98560180037837,27.1377253087318));
#8163=CARTESIAN_POINT('Ctrl Pts',(1.37094092201097,-2.03278539840022,27.1334458790179));
#8164=CARTESIAN_POINT('Ctrl Pts',(1.3013496034633,-2.07640060189885,27.129166449304));
#8165=CARTESIAN_POINT('Ctrl Pts',(1.23175828491566,-2.12001580539746,27.1248870195901));
#8166=CARTESIAN_POINT('Ctrl Pts',(1.1600775939914,-2.1600624322741,27.1206075898763));
#8167=CARTESIAN_POINT('Ctrl Pts',(1.08671585527949,-2.19636037568614,27.1163281601624));
#8168=CARTESIAN_POINT('Ctrl Pts',(1.01418945081432,-2.23224501216529,27.1120974582221));
#8169=CARTESIAN_POINT('Ctrl Pts',(0.939747313560539,-2.26460091096603,27.1078667562818));
#8170=CARTESIAN_POINT('Ctrl Pts',(0.863766980855441,-2.29321975675771,27.1036360543416));
#8171=CARTESIAN_POINT('Ctrl Pts',(0.787895810981903,-2.32179748514266,27.0994114307559));
#8172=CARTESIAN_POINT('Ctrl Pts',(0.710491266285224,-2.3466486613437,27.0951868071702));
#8173=CARTESIAN_POINT('Ctrl Pts',(0.631954089816945,-2.36761151339565,27.0909621835846));
#8174=CARTESIAN_POINT('Ctrl Pts',(0.553107806560379,-2.38865687108585,27.0867209327163));
#8175=CARTESIAN_POINT('Ctrl Pts',(0.473120382119022,-2.40578302118066,27.082479681848));
#8176=CARTESIAN_POINT('Ctrl Pts',(0.392416157402072,-2.41887573252736,27.0782384309797));
#8177=CARTESIAN_POINT('Ctrl Pts',(0.312173401513568,-2.43189357941453,27.0740214316927));
#8178=CARTESIAN_POINT('Ctrl Pts',(0.231222484143448,-2.44092391377583,27.0698044324058));
#8179=CARTESIAN_POINT('Ctrl Pts',(0.149992402095245,-2.44590525763238,27.0655874331188));
#8180=CARTESIAN_POINT('Ctrl Pts',(0.0687892495963295,-2.45088495006446,
27.0613718318594));
#8181=CARTESIAN_POINT('Ctrl Pts',(-0.0126924199730705,-2.45181828918591,
27.0571562305999));
#8182=CARTESIAN_POINT('Ctrl Pts',(-0.0940190465854,-2.44869570769403,27.0529406293405));
#8183=CARTESIAN_POINT('Ctrl Pts',(-0.175343643888364,-2.44557320411862,
27.0487251332712));
#8184=CARTESIAN_POINT('Ctrl Pts',(-0.256512741249791,-2.43839500007911,
27.0445096372019));
#8185=CARTESIAN_POINT('Ctrl Pts',(-0.337094783833534,-2.42720360841694,
27.0402941411326));
#8186=CARTESIAN_POINT('Ctrl Pts',(-0.418530700501074,-2.41589362905216,
27.036033976267));
#8187=CARTESIAN_POINT('Ctrl Pts',(-0.499366564979165,-2.40048495620401,
27.0317738114014));
#8188=CARTESIAN_POINT('Ctrl Pts',(-0.579166209922435,-2.38107470510358,
27.0275136465359));
#8189=CARTESIAN_POINT('Ctrl Pts',(-0.65824413253653,-2.36184000380219,27.0232920113669));
#8190=CARTESIAN_POINT('Ctrl Pts',(-0.736304070494887,-2.33867600803522,
27.0190703761979));
#8191=CARTESIAN_POINT('Ctrl Pts',(-0.812937422334597,-2.31172727573301,
27.0148487410289));
#8192=CARTESIAN_POINT('Ctrl Pts',(-0.890619891286033,-2.28440961299101,
27.0105693113151));
#8193=CARTESIAN_POINT('Ctrl Pts',(-0.96683596043162,-2.25320298979247,27.0062898816012));
#8194=CARTESIAN_POINT('Ctrl Pts',(-1.04118333516336,-2.21830735304604,27.0020104518873));
#8195=CARTESIAN_POINT('Ctrl Pts',(-1.11553070989507,-2.18341171629961,26.9977310221734));
#8196=CARTESIAN_POINT('Ctrl Pts',(-1.18800898794173,-2.14482735435103,26.9934515924595));
#8197=CARTESIAN_POINT('Ctrl Pts',(-1.25824567135078,-2.10280005719208,26.9891721627456));
#8198=CARTESIAN_POINT('Ctrl Pts',(-1.32768260398948,-2.06125130431579,26.9849414608054));
#8199=CARTESIAN_POINT('Ctrl Pts',(-1.39518992430469,-2.01618138430327,26.9807107588651));
#8200=CARTESIAN_POINT('Ctrl Pts',(-1.46038808642811,-1.96779493012327,26.9764800569249));
#8201=CARTESIAN_POINT('Ctrl Pts',(-1.52549257673238,-1.91947799396399,26.9722554333392));
#8202=CARTESIAN_POINT('Ctrl Pts',(-1.58829412754739,-1.86785426188774,26.9680308097535));
#8203=CARTESIAN_POINT('Ctrl Pts',(-1.64843976084093,-1.81317307637156,26.9638061861679));
#8204=CARTESIAN_POINT('Ctrl Pts',(-1.70882211544764,-1.75827667652754,26.9595649352996));
#8205=CARTESIAN_POINT('Ctrl Pts',(-1.76652719414015,-1.70029894822672,26.9553236844313));
#8206=CARTESIAN_POINT('Ctrl Pts',(-1.82122921302229,-1.63953481318153,26.951082433563));
#8207=CARTESIAN_POINT('Ctrl Pts',(-1.87561844435622,-1.57911812902039,26.946865434276));
#8208=CARTESIAN_POINT('Ctrl Pts',(-1.92703855155125,-1.5159471662467,26.9426484349891));
#8209=CARTESIAN_POINT('Ctrl Pts',(-1.9752055825826,-1.45034932224431,26.9384314357021));
#8210=CARTESIAN_POINT('Ctrl Pts',(-2.02335664518941,-1.3847732253623,26.9342158344427));
#8211=CARTESIAN_POINT('Ctrl Pts',(-2.06825649825091,-1.3167722195407,26.9300002331833));
#8212=CARTESIAN_POINT('Ctrl Pts',(-2.10966236345032,-1.24670564378333,26.9257846319239));
#8213=CARTESIAN_POINT('Ctrl Pts',(-2.15106719546648,-1.17664081636793,26.9215691358546));
#8214=CARTESIAN_POINT('Ctrl Pts',(-2.18897797729587,-1.10451092242129,26.9173536397853));
#8215=CARTESIAN_POINT('Ctrl Pts',(-2.22319680302907,-1.03070181187448,26.913138143716));
#8216=CARTESIAN_POINT('Ctrl Pts',(-2.25777822280366,-0.956110595480615,
26.9088779788504));
#8217=CARTESIAN_POINT('Ctrl Pts',(-2.28858875983367,-0.879804796272364,
26.9046178139848));
#8218=CARTESIAN_POINT('Ctrl Pts',(-2.31547391831242,-0.802203704563214,
26.9003576491192));
#8219=CARTESIAN_POINT('Ctrl Pts',(-2.34211592258636,-0.725304451073139,
26.8961360139502));
#8220=CARTESIAN_POINT('Ctrl Pts',(-2.36490319402609,-0.647133709268832,
26.8919143787813));
#8221=CARTESIAN_POINT('Ctrl Pts',(-2.38373604912657,-0.568113279280151,
26.8876927436124));
#8222=CARTESIAN_POINT('Ctrl Pts',(-2.40282672761708,-0.488011052875974,
26.8834133138985));
#8223=CARTESIAN_POINT('Ctrl Pts',(-2.41785380712046,-0.407036183878763,
26.8791338841845));
#8224=CARTESIAN_POINT('Ctrl Pts',(-2.42876758743783,-0.325635158131675,
26.8748544544706));
#8225=CARTESIAN_POINT('Ctrl Pts',(-2.43968136775519,-0.244234132384586,
26.8705750247567));
#8226=CARTESIAN_POINT('Ctrl Pts',(-2.44648187352098,-0.16240744421396,26.8662955950428));
#8227=CARTESIAN_POINT('Ctrl Pts',(-2.44917407971559,-0.080601347689007,
26.8620161653289));
#8228=CARTESIAN_POINT('Ctrl Pts',(-2.45005244916336,-0.0539109790342361,
26.86061994229));
#8229=CARTESIAN_POINT('Ctrl Pts',(-2.4504945386623,-0.0272061736956886,
26.859223719251));
#8230=CARTESIAN_POINT('Ctrl Pts',(-2.45049994971379,-0.000496440046205509,
26.857827496212));
#8231=CARTESIAN_POINT('',(-2.45049921122159,-0.00196616437574762,26.0578274962121));
#8232=CARTESIAN_POINT('Ctrl Pts',(-2.4544163928919,-0.000486308122271454,
26.8578269260125));
#8233=CARTESIAN_POINT('Ctrl Pts',(-2.45223809250971,0.784885029909544,26.8168380066458));
#8234=CARTESIAN_POINT('Ctrl Pts',(-1.61768872140475,2.38635253781045,26.7334637548067));
#8235=CARTESIAN_POINT('Ctrl Pts',(1.11139905977937,2.675821036374,26.6077041704954));
#8236=CARTESIAN_POINT('Ctrl Pts',(2.85144128369585,0.514304087493417,26.4805481730787));
#8237=CARTESIAN_POINT('Ctrl Pts',(1.97620912114127,-2.11892038507884,26.3533921756619));
#8238=CARTESIAN_POINT('Ctrl Pts',(-0.711555225186118,-2.80872128383892,
26.2262361782453));
#8239=CARTESIAN_POINT('Ctrl Pts',(-2.28839663859365,-1.34721059041725,26.1277149111577));
#8240=CARTESIAN_POINT('Ctrl Pts',(-2.45037331171153,-0.267128835091938,
26.0715789765424));
#8241=CARTESIAN_POINT('Ctrl Pts',(-2.44838624420166,-0.00198140266975247,
26.0578283743994));
#8242=CARTESIAN_POINT('',(-2.45049957242558,0.00144759872447857,25.2578274962121));
#8243=CARTESIAN_POINT('Ctrl Pts',(-2.45049921122159,-0.00196616437574762,
26.0578274962121));
#8244=CARTESIAN_POINT('Ctrl Pts',(-2.45056435292045,0.0792222060620601,
26.0536206531643));
#8245=CARTESIAN_POINT('Ctrl Pts',(-2.44659036857391,0.160464817053481,26.0494138101165));
#8246=CARTESIAN_POINT('Ctrl Pts',(-2.43858777176841,0.24132950375277,26.0452069670687));
#8247=CARTESIAN_POINT('Ctrl Pts',(-2.43058695487118,0.322176204824771,26.0410010596915));
#8248=CARTESIAN_POINT('Ctrl Pts',(-2.41855935099294,0.402644684117423,26.0367951523142));
#8249=CARTESIAN_POINT('Ctrl Pts',(-2.40256742063308,0.482306996955797,26.032589244937));
#8250=CARTESIAN_POINT('Ctrl Pts',(-2.38657409952559,0.561976237674043,26.0283829717906));
#8251=CARTESIAN_POINT('Ctrl Pts',(-2.36661586067349,0.640838715264166,26.0241766986442));
#8252=CARTESIAN_POINT('Ctrl Pts',(-2.3428061629636,0.718477231914684,26.0199704254978));
#8253=CARTESIAN_POINT('Ctrl Pts',(-2.31897018853183,0.796201431539173,26.0157595102484));
#8254=CARTESIAN_POINT('Ctrl Pts',(-2.29127440516051,0.872698525716211,26.0115485949989));
#8255=CARTESIAN_POINT('Ctrl Pts',(-2.25988184464622,0.947567569220482,26.0073376797495));
#8256=CARTESIAN_POINT('Ctrl Pts',(-2.22847154773062,1.02247891279138,26.003124385386));
#8257=CARTESIAN_POINT('Ctrl Pts',(-2.19336051763349,1.09575995335672,25.9989110910225));
#8258=CARTESIAN_POINT('Ctrl Pts',(-2.15475843919057,1.16703312666651,25.994697796659));
#8259=CARTESIAN_POINT('Ctrl Pts',(-2.11608554478923,1.23843705143533,25.9904767729583));
#8260=CARTESIAN_POINT('Ctrl Pts',(-2.07390905318347,1.30782535253546,25.9862557492577));
#8261=CARTESIAN_POINT('Ctrl Pts',(-2.02848263731192,1.3748485153369,25.982034725557));
#8262=CARTESIAN_POINT('Ctrl Pts',(-1.9922129450324,1.42836164076776,25.9786645448419));
#8263=CARTESIAN_POINT('Ctrl Pts',(-1.95387236655002,1.4803675466132,25.9752943641268));
#8264=CARTESIAN_POINT('Ctrl Pts',(-1.91360765035828,1.5307044164339,25.9719241834117));
#8265=CARTESIAN_POINT('Ctrl Pts',(-1.86306198906733,1.59389399314142,25.9676934814714));
#8266=CARTESIAN_POINT('Ctrl Pts',(-1.80928801626885,1.65469609701548,25.9634627795312));
#8267=CARTESIAN_POINT('Ctrl Pts',(-1.75253974839819,1.71276229532426,25.9592320775909));
#8268=CARTESIAN_POINT('Ctrl Pts',(-1.69587301217369,1.77074506848346,25.9550074540053));
#8269=CARTESIAN_POINT('Ctrl Pts',(-1.63624079006716,1.82599941297201,25.9507828304196));
#8270=CARTESIAN_POINT('Ctrl Pts',(-1.57393781039758,1.87820925857607,25.9465582068339));
#8271=CARTESIAN_POINT('Ctrl Pts',(-1.51138961852615,1.93062459180315,25.9423169559657));
#8272=CARTESIAN_POINT('Ctrl Pts',(-1.44614989728376,1.97997103907197,25.9380757050974));
#8273=CARTESIAN_POINT('Ctrl Pts',(-1.37855486404961,2.02596563070679,25.9338344542291));
#8274=CARTESIAN_POINT('Ctrl Pts',(-1.31134634095089,2.0716972240858,25.9296174549422));
#8275=CARTESIAN_POINT('Ctrl Pts',(-1.24180975659438,2.11411492555232,25.9254004556552));
#8276=CARTESIAN_POINT('Ctrl Pts',(-1.17030785705621,2.1529815999475,25.9211834563683));
#8277=CARTESIAN_POINT('Ctrl Pts',(-1.09882966196187,2.19183538918989,25.9169678551089));
#8278=CARTESIAN_POINT('Ctrl Pts',(-1.02538785381665,2.22714026723881,25.9127522538495));
#8279=CARTESIAN_POINT('Ctrl Pts',(-0.950371267120706,2.25870420919415,25.90853665259));
#8280=CARTESIAN_POINT('Ctrl Pts',(-0.875356552282358,2.29026736354762,25.9043211565208));
#8281=CARTESIAN_POINT('Ctrl Pts',(-0.798767566102965,2.3180895880393,25.9001056604515));
#8282=CARTESIAN_POINT('Ctrl Pts',(-0.721013351052304,2.34202689941946,25.8958901643822));
#8283=CARTESIAN_POINT('Ctrl Pts',(-0.642435226516857,2.36621785850057,25.8916299995166));
#8284=CARTESIAN_POINT('Ctrl Pts',(-0.562667490052483,2.38644092464468,25.887369834651));
#8285=CARTESIAN_POINT('Ctrl Pts',(-0.482146455556506,2.40259964317701,25.8831096697854));
#8286=CARTESIAN_POINT('Ctrl Pts',(-0.402353667767159,2.41861221935501,25.8788880346165));
#8287=CARTESIAN_POINT('Ctrl Pts',(-0.32182162725187,2.4306336612126,25.8746663994475));
#8288=CARTESIAN_POINT('Ctrl Pts',(-0.240981732254135,2.43862216317325,25.8704447642786));
#8289=CARTESIAN_POINT('Ctrl Pts',(-0.159035132209623,2.44672002840604,25.8661653345647));
#8290=CARTESIAN_POINT('Ctrl Pts',(-0.0767726788353745,2.4506736713357,25.8618859048508));
#8291=CARTESIAN_POINT('Ctrl Pts',(0.00535652038182216,2.45049414561419,
25.8576064751368));
#8292=CARTESIAN_POINT('Ctrl Pts',(0.0874857195990188,2.45031461989267,25.8533270454229));
#8293=CARTESIAN_POINT('Ctrl Pts',(0.169481178188457,2.4460020166882,25.849047615709));
#8294=CARTESIAN_POINT('Ctrl Pts',(0.250901402272095,2.43762153262927,25.8447681859951));
#8295=CARTESIAN_POINT('Ctrl Pts',(0.331394534075678,2.42933647304457,25.8405374840548));
#8296=CARTESIAN_POINT('Ctrl Pts',(0.411628226227733,2.4170445801981,25.8363067821146));
#8297=CARTESIAN_POINT('Ctrl Pts',(0.491172003780412,2.40077077471014,25.8320760801743));
#8298=CARTESIAN_POINT('Ctrl Pts',(0.570601498811814,2.38452035020281,25.8278514565886));
#8299=CARTESIAN_POINT('Ctrl Pts',(0.649342596099335,2.36429946752621,25.823626833003));
#8300=CARTESIAN_POINT('Ctrl Pts',(0.726969987829524,2.34018479757372,25.8194022094173));
#8301=CARTESIAN_POINT('Ctrl Pts',(0.804902905615379,2.31597521705126,25.815160958549));
#8302=CARTESIAN_POINT('Ctrl Pts',(0.881712860331046,2.28784118174851,25.8109197076807));
#8303=CARTESIAN_POINT('Ctrl Pts',(0.956979911020769,2.25591216582177,25.8066784568124));
#8304=CARTESIAN_POINT('Ctrl Pts',(1.03181658278257,2.22416572082771,25.8024614575254));
#8305=CARTESIAN_POINT('Ctrl Pts',(1.10512751493269,2.18866776047779,25.7982444582385));
#8306=CARTESIAN_POINT('Ctrl Pts',(1.17651693927947,2.14959487848024,25.7940274589515));
#8307=CARTESIAN_POINT('Ctrl Pts',(1.24788269647031,2.11053494999785,25.7898118576921));
#8308=CARTESIAN_POINT('Ctrl Pts',(1.31732780324429,2.06790267650847,25.7855962564327));
#8309=CARTESIAN_POINT('Ctrl Pts',(1.38448029361734,2.02192100898756,25.7813806551732));
#8310=CARTESIAN_POINT('Ctrl Pts',(1.45163110836222,1.97594048882807,25.7771651591039));
#8311=CARTESIAN_POINT('Ctrl Pts',(1.51648903733628,1.92661100445138,25.7729496630346));
#8312=CARTESIAN_POINT('Ctrl Pts',(1.57871156510025,1.87419850715411,25.7687341669653));
#8313=CARTESIAN_POINT('Ctrl Pts',(1.64159342343222,1.82123062962955,25.7644740020997));
#8314=CARTESIAN_POINT('Ctrl Pts',(1.70178331591786,1.76511431268473,25.7602138372342));
#8315=CARTESIAN_POINT('Ctrl Pts',(1.75896392205096,1.70616416880765,25.7559536723686));
#8316=CARTESIAN_POINT('Ctrl Pts',(1.81562737650644,1.64774718062555,25.7517320371996));
#8317=CARTESIAN_POINT('Ctrl Pts',(1.86933549493996,1.58654781275082,25.7475104020306));
#8318=CARTESIAN_POINT('Ctrl Pts',(1.919819564879,1.52290613246773,25.7432887668617));
#8319=CARTESIAN_POINT('Ctrl Pts',(1.97099476603426,1.45839319216242,25.7390093371478));
#8320=CARTESIAN_POINT('Ctrl Pts',(2.01885668784557,1.39137096474473,25.7347299074339));
#8321=CARTESIAN_POINT('Ctrl Pts',(2.06317147164031,1.32222302529094,25.73045047772));
#8322=CARTESIAN_POINT('Ctrl Pts',(2.10748625543506,1.25307508583716,25.7261710480061));
#8323=CARTESIAN_POINT('Ctrl Pts',(2.14825371448258,1.18180189271072,25.7218916182921));
#8324=CARTESIAN_POINT('Ctrl Pts',(2.18528963332306,1.10880993343799,25.7176121885782));
#8325=CARTESIAN_POINT('Ctrl Pts',(2.2219038422652,1.03664909791454,25.713381486638));
#8326=CARTESIAN_POINT('Ctrl Pts',(2.25500881229822,0.962537041235193,25.7091507846977));
#8327=CARTESIAN_POINT('Ctrl Pts',(2.28439243138472,0.886849180769873,25.7049200827574));
#8328=CARTESIAN_POINT('Ctrl Pts',(2.31373383429575,0.811270062933873,25.7006954591718));
#8329=CARTESIAN_POINT('Ctrl Pts',(2.33936433793749,0.734120067591182,25.6964708355861));
#8330=CARTESIAN_POINT('Ctrl Pts',(2.36111813725174,0.655798286015512,25.6922462120004));
#8331=CARTESIAN_POINT('Ctrl Pts',(2.38295755521612,0.577168245403439,25.6880049611321));
#8332=CARTESIAN_POINT('Ctrl Pts',(2.40088947279089,0.497357598131797,25.6837637102638));
#8333=CARTESIAN_POINT('Ctrl Pts',(2.41479538533874,0.416789511560387,25.6795224593955));
#8334=CARTESIAN_POINT('Ctrl Pts',(2.42862178352172,0.336682115375852,25.6753054601086));
#8335=CARTESIAN_POINT('Ctrl Pts',(2.43846801344614,0.255826381392194,25.6710884608216));
#8336=CARTESIAN_POINT('Ctrl Pts',(2.4442682740133,0.174650664619582,25.6668714615346));
#8337=CARTESIAN_POINT('Ctrl Pts',(2.45006661166717,0.093501859373048,25.6626558602752));
#8338=CARTESIAN_POINT('Ctrl Pts',(2.45182161049298,0.0120337455071861,25.6584402590158));
#8339=CARTESIAN_POINT('Ctrl Pts',(2.44951933141037,-0.0693202354792845,
25.6542246577563));
#8340=CARTESIAN_POINT('Ctrl Pts',(2.44721710977556,-0.150672186473967,25.650009161687));
#8341=CARTESIAN_POINT('Ctrl Pts',(2.44085782576188,-0.231909545407921,25.6457936656177));
#8342=CARTESIAN_POINT('Ctrl Pts',(2.43047963800632,-0.312600350666281,25.6415781695484));
#8343=CARTESIAN_POINT('Ctrl Pts',(2.41999147952684,-0.394146182493485,25.6373180046828));
#8344=CARTESIAN_POINT('Ctrl Pts',(2.40539878471959,-0.47513332618364,25.6330578398173));
#8345=CARTESIAN_POINT('Ctrl Pts',(2.3867942653195,-0.555124657205891,25.6287976749517));
#8346=CARTESIAN_POINT('Ctrl Pts',(2.36835800853611,-0.634392532255847,25.6245760397827));
#8347=CARTESIAN_POINT('Ctrl Pts',(2.3459823911617,-0.712682099639198,25.6203544046137));
#8348=CARTESIAN_POINT('Ctrl Pts',(2.3198078432079,-0.789583320866838,25.6161327694448));
#8349=CARTESIAN_POINT('Ctrl Pts',(2.29327496346407,-0.867537326360603,25.6118533397309));
#8350=CARTESIAN_POINT('Ctrl Pts',(2.26283853301571,-0.944064225088884,25.607573910017));
#8351=CARTESIAN_POINT('Ctrl Pts',(2.2286944316381,-1.01875972652305,25.6032944803032));
#8352=CARTESIAN_POINT('Ctrl Pts',(2.19455033026049,-1.09345522795721,25.5990150505893));
#8353=CARTESIAN_POINT('Ctrl Pts',(2.15669884222795,-1.16631892693866,25.5947356208754));
#8354=CARTESIAN_POINT('Ctrl Pts',(2.11538198855404,-1.23697586577151,25.5904561911616));
#8355=CARTESIAN_POINT('Ctrl Pts',(2.07453558968995,-1.30682826859142,25.5862254892213));
#8356=CARTESIAN_POINT('Ctrl Pts',(2.03014874344254,-1.37478666664726,25.581994787281));
#8357=CARTESIAN_POINT('Ctrl Pts',(1.98242224482002,-1.44046946973643,25.5777640853408));
#8358=CARTESIAN_POINT('Ctrl Pts',(1.93476431604378,-1.50605790471059,25.5735394617551));
#8359=CARTESIAN_POINT('Ctrl Pts',(1.88377653536067,-1.56937686489839,25.5693148381694));
#8360=CARTESIAN_POINT('Ctrl Pts',(1.82970467293873,-1.63007087570639,25.5650902145838));
#8361=CARTESIAN_POINT('Ctrl Pts',(1.7754199943641,-1.69100376613296,25.5608489637155));
#8362=CARTESIAN_POINT('Ctrl Pts',(1.71802714485775,-1.74929059064225,25.5566077128472));
#8363=CARTESIAN_POINT('Ctrl Pts',(1.65781774574641,-1.80460260774728,25.5523664619789));
#8364=CARTESIAN_POINT('Ctrl Pts',(1.5979526255247,-1.85959834931871,25.5481494626919));
#8365=CARTESIAN_POINT('Ctrl Pts',(1.53530342442255,-1.91165289343347,25.543932463405));
#8366=CARTESIAN_POINT('Ctrl Pts',(1.47019465964294,-1.96047900084581,25.539715464118));
#8367=CARTESIAN_POINT('Ctrl Pts',(1.40510747984327,-2.00928892133535,25.5354998628586));
#8368=CARTESIAN_POINT('Ctrl Pts',(1.33756272737899,-2.05487225175624,25.5312842615991));
#8369=CARTESIAN_POINT('Ctrl Pts',(1.26791727466772,-2.09698260235968,25.5270686603397));
#8370=CARTESIAN_POINT('Ctrl Pts',(1.19827355979029,-2.13909190220116,25.5228531642704));
#8371=CARTESIAN_POINT('Ctrl Pts',(1.12652964741628,-2.17772815482706,25.5186376682011));
#8372=CARTESIAN_POINT('Ctrl Pts',(1.05306937206114,-2.21268957326299,25.5144221721318));
#8373=CARTESIAN_POINT('Ctrl Pts',(0.97883068723278,-2.24802145449907,25.5101620072662));
#8374=CARTESIAN_POINT('Ctrl Pts',(0.902839479066593,-2.27959993556317,25.5059018424006));
#8375=CARTESIAN_POINT('Ctrl Pts',(0.82551345853199,-2.30726630014451,25.501641677535));
#8376=CARTESIAN_POINT('Ctrl Pts',(0.74888678842311,-2.33468244515275,25.497420042366));
#8377=CARTESIAN_POINT('Ctrl Pts',(0.670949821353316,-2.35825687574802,25.4931984071971));
#8378=CARTESIAN_POINT('Ctrl Pts',(0.592123330738969,-2.37788565982357,25.4889767720281));
#8379=CARTESIAN_POINT('Ctrl Pts',(0.512217698755994,-2.39778316362452,25.4846973423142));
#8380=CARTESIAN_POINT('Ctrl Pts',(0.431398488927583,-2.41362607529511,25.4804179126003));
#8381=CARTESIAN_POINT('Ctrl Pts',(0.35011166318798,-2.42536019454838,25.4761384828864));
#8382=CARTESIAN_POINT('Ctrl Pts',(0.2688248374484,-2.43709431380164,25.4718590531725));
#8383=CARTESIAN_POINT('Ctrl Pts',(0.187070890347262,-2.44471966028572,25.4675796234586));
#8384=CARTESIAN_POINT('Ctrl Pts',(0.105296103432033,-2.44823670844999,25.4633001937447));
#8385=CARTESIAN_POINT('Ctrl Pts',(0.0244524460301832,-2.45171370970654,
25.4590694918045));
#8386=CARTESIAN_POINT('Ctrl Pts',(-0.0567156527727147,-2.4511886165742,
25.4548387898642));
#8387=CARTESIAN_POINT('Ctrl Pts',(-0.137778655346964,-2.44662365151054,
25.450608087924));
#8388=CARTESIAN_POINT('Ctrl Pts',(-0.218725192691977,-2.44206524504558,
25.4463834643383));
#8389=CARTESIAN_POINT('Ctrl Pts',(-0.299566473306361,-2.43347852000476,
25.4421588407526));
#8390=CARTESIAN_POINT('Ctrl Pts',(-0.379870566370954,-2.42087765134982,
25.4379342171669));
#8391=CARTESIAN_POINT('Ctrl Pts',(-0.460490720457817,-2.40822718816891,
25.4336929662986));
#8392=CARTESIAN_POINT('Ctrl Pts',(-0.540568975281544,-2.39153089546019,
25.4294517154303));
#8393=CARTESIAN_POINT('Ctrl Pts',(-0.619671051722867,-2.37085597151254,
25.4252104645621));
#8394=CARTESIAN_POINT('Ctrl Pts',(-0.698320820460437,-2.35029926731078,
25.4209934652751));
#8395=CARTESIAN_POINT('Ctrl Pts',(-0.776005089679771,-2.32580942701831,
25.4167764659882));
#8396=CARTESIAN_POINT('Ctrl Pts',(-0.852306663366028,-2.29750377618446,
25.4125594667012));
#8397=CARTESIAN_POINT('Ctrl Pts',(-0.928582941411364,-2.26920750929311,
25.4083438654418));
#8398=CARTESIAN_POINT('Ctrl Pts',(-1.00347699853692,-2.23709810560883,25.4041282641824));
#8399=CARTESIAN_POINT('Ctrl Pts',(-1.07658846575323,-2.20134220997261,25.399912662923));
#8400=CARTESIAN_POINT('Ctrl Pts',(-1.14969810864951,-2.16558720653839,25.3956971668537));
#8401=CARTESIAN_POINT('Ctrl Pts',(-1.22102483277604,-2.12618609735331,25.3914816707844));
#8402=CARTESIAN_POINT('Ctrl Pts',(-1.2901911716623,-2.08335234431544,25.3872661747151));
#8403=CARTESIAN_POINT('Ctrl Pts',(-1.36009042004543,-2.04006471060537,25.3830060098496));
#8404=CARTESIAN_POINT('Ctrl Pts',(-1.42778280589333,-1.99327149439715,25.378745844984));
#8405=CARTESIAN_POINT('Ctrl Pts',(-1.49290873360644,-1.94323795843988,25.3744856801184));
#8406=CARTESIAN_POINT('Ctrl Pts',(-1.55744565072549,-1.89365693477338,25.3702640449494));
#8407=CARTESIAN_POINT('Ctrl Pts',(-1.61946202784756,-1.84089431938574,25.3660424097805));
#8408=CARTESIAN_POINT('Ctrl Pts',(-1.67864267155972,-1.78524761061844,25.3618207746115));
#8409=CARTESIAN_POINT('Ctrl Pts',(-1.73863350332392,-1.72883909366943,25.3575413448976));
#8410=CARTESIAN_POINT('Ctrl Pts',(-1.79571002811989,-1.66946727506207,25.3532619151837));
#8411=CARTESIAN_POINT('Ctrl Pts',(-1.84958522757434,-1.60747775597014,25.3489824854698));
#8412=CARTESIAN_POINT('Ctrl Pts',(-1.90346042702879,-1.5454882368782,25.3447030557559));
#8413=CARTESIAN_POINT('Ctrl Pts',(-1.95413404990601,-1.48088144373573,25.340423626042));
#8414=CARTESIAN_POINT('Ctrl Pts',(-2.00136487298623,-1.41403284798367,25.3361441963281));
#8415=CARTESIAN_POINT('Ctrl Pts',(-2.04854588977562,-1.3472547460402,25.3318692793986));
#8416=CARTESIAN_POINT('Ctrl Pts',(-2.09246741364592,-1.27799073561874,25.3275943624691));
#8417=CARTESIAN_POINT('Ctrl Pts',(-2.13286079451398,-1.20658819869298,25.3233194455395));
#8418=CARTESIAN_POINT('Ctrl Pts',(-2.17319329701699,-1.13529327518346,25.3190509714961));
#8419=CARTESIAN_POINT('Ctrl Pts',(-2.21000799855808,-1.06186661759494,25.3147824974527));
#8420=CARTESIAN_POINT('Ctrl Pts',(-2.24307855145268,-0.986685797005798,
25.3105140234094));
#8421=CARTESIAN_POINT('Ctrl Pts',(-2.27709485655374,-0.909354954093692,
25.3061234794762));
#8422=CARTESIAN_POINT('Ctrl Pts',(-2.30714929978556,-0.830168471242618,
25.3017329355431));
#8423=CARTESIAN_POINT('Ctrl Pts',(-2.33304538151715,-0.749566206403059,
25.29734239161));
#8424=CARTESIAN_POINT('Ctrl Pts',(-2.35816409428234,-0.671383523798304,
25.2930836464809));
#8425=CARTESIAN_POINT('Ctrl Pts',(-2.37937041262085,-0.591869318873139,
25.2888249013517));
#8426=CARTESIAN_POINT('Ctrl Pts',(-2.39653373568158,-0.511445308649984,
25.2845661562226));
#8427=CARTESIAN_POINT('Ctrl Pts',(-2.41449380944562,-0.427287878827297,
25.2801097128875));
#8428=CARTESIAN_POINT('Ctrl Pts',(-2.42802622608005,-0.342134607467247,
25.2756532695524));
#8429=CARTESIAN_POINT('Ctrl Pts',(-2.43704040685765,-0.256484512871788,
25.2711968262173));
#8430=CARTESIAN_POINT('Ctrl Pts',(-2.44605458763526,-0.17083441827633,25.2667403828823));
#8431=CARTESIAN_POINT('Ctrl Pts',(-2.45055045587722,-0.0846880646955054,
25.2622839395472));
#8432=CARTESIAN_POINT('Ctrl Pts',(-2.45049957242558,0.00144759872447857,
25.2578274962121));
#8433=CARTESIAN_POINT('',(-2.45049965096235,0.00130791185359291,24.4578274962121));
#8434=CARTESIAN_POINT('Ctrl Pts',(-2.44733420835662,0.00146391743851001,
25.2578265539622));
#8435=CARTESIAN_POINT('Ctrl Pts',(-2.44901787875617,0.315713360581297,25.2415471022785));
#8436=CARTESIAN_POINT('Ctrl Pts',(-2.24674587549421,1.44605613207129,25.1828823181227));
#8437=CARTESIAN_POINT('Ctrl Pts',(-0.543033478857258,2.84610975361437,25.0818322014945));
#8438=CARTESIAN_POINT('Ctrl Pts',(2.09888342822537,1.99747701951716,24.9546762040779));
#8439=CARTESIAN_POINT('Ctrl Pts',(2.81575418359161,-0.683194310844983,24.8275202066611));
#8440=CARTESIAN_POINT('Ctrl Pts',(0.950081915167995,-2.73725600615837,24.7003642092443));
#8441=CARTESIAN_POINT('Ctrl Pts',(-1.70248630229997,-2.29486360804804,24.5771336791462));
#8442=CARTESIAN_POINT('Ctrl Pts',(-2.44889894900063,-0.73622003660141,24.49628848152));
#8443=CARTESIAN_POINT('Ctrl Pts',(-2.45367044800944,0.00128812415959639,
24.4578286163662));
#8444=CARTESIAN_POINT('',(-2.45049903536358,-0.00217432338460381,23.6578274961682));
#8445=CARTESIAN_POINT('Ctrl Pts',(-2.45049965096235,0.00130791185359291,
24.4578274962121));
#8446=CARTESIAN_POINT('Ctrl Pts',(-2.45045953015351,0.0764781366572466,
24.4539024022783));
#8447=CARTESIAN_POINT('Ctrl Pts',(-2.44696089914348,0.151553924908564,24.4499773083446));
#8448=CARTESIAN_POINT('Ctrl Pts',(-2.44002780973264,0.226306291851005,24.4460522144109));
#8449=CARTESIAN_POINT('Ctrl Pts',(-2.43255490964,0.306878881752235,24.4418215124709));
#8450=CARTESIAN_POINT('Ctrl Pts',(-2.4210727636996,0.387232452363853,24.4375908105308));
#8451=CARTESIAN_POINT('Ctrl Pts',(-2.405601950112,0.466936299314313,24.4333601085908));
#8452=CARTESIAN_POINT('Ctrl Pts',(-2.39015336382661,0.546525633767834,24.4291354850053));
#8453=CARTESIAN_POINT('Ctrl Pts',(-2.37072757908059,0.625466645825196,24.4249108614199));
#8454=CARTESIAN_POINT('Ctrl Pts',(-2.34739697382438,0.70333327610751,24.4206862378344));
#8455=CARTESIAN_POINT('Ctrl Pts',(-2.32397454392048,0.78150637404527,24.4164449869661));
#8456=CARTESIAN_POINT('Ctrl Pts',(-2.29661653420305,0.858596142434194,24.4122037360978));
#8457=CARTESIAN_POINT('Ctrl Pts',(-2.26544817732281,0.934181355982198,24.4079624852294));
#8458=CARTESIAN_POINT('Ctrl Pts',(-2.23445804190903,1.0093343713347,24.4037454859427));
#8459=CARTESIAN_POINT('Ctrl Pts',(-2.1997011954864,1.08299955705959,24.3995284866559));
#8460=CARTESIAN_POINT('Ctrl Pts',(-2.16135023163334,1.15477938421956,24.3953114873691));
#8461=CARTESIAN_POINT('Ctrl Pts',(-2.12301198196381,1.22653541479649,24.3910958861099));
#8462=CARTESIAN_POINT('Ctrl Pts',(-2.0810822000198,1.29640691816708,24.3868802848506));
#8463=CARTESIAN_POINT('Ctrl Pts',(-2.03578007432459,1.36401969889843,24.3826646835914));
#8464=CARTESIAN_POINT('Ctrl Pts',(-1.99047907903441,1.43163079251628,24.3784491875222));
#8465=CARTESIAN_POINT('Ctrl Pts',(-1.94180616706901,1.49698288980419,24.3742336914531));
#8466=CARTESIAN_POINT('Ctrl Pts',(-1.8900238220821,1.55973081073696,24.370018195384));
#8467=CARTESIAN_POINT('Ctrl Pts',(-1.837692774166,1.62314362948432,24.3657580305182));
#8468=CARTESIAN_POINT('Ctrl Pts',(-1.78218629962538,1.6838963699139,24.3614978656523));
#8469=CARTESIAN_POINT('Ctrl Pts',(-1.72381579491089,1.74166855492534,24.3572377007865));
#8470=CARTESIAN_POINT('Ctrl Pts',(-1.66597320353632,1.79891823790784,24.3530160656177));
#8471=CARTESIAN_POINT('Ctrl Pts',(-1.60531857067758,1.85324079423695,24.3487944304489));
#8472=CARTESIAN_POINT('Ctrl Pts',(-1.54218923647797,1.9043640956738,24.3445727952801));
#8473=CARTESIAN_POINT('Ctrl Pts',(-1.47819565630826,1.95618727946813,24.3402933655658));
#8474=CARTESIAN_POINT('Ctrl Pts',(-1.41165950364437,2.00472265746796,24.3360139358514));
#8475=CARTESIAN_POINT('Ctrl Pts',(-1.34296197569482,2.04973251470475,24.3317345061371));
#8476=CARTESIAN_POINT('Ctrl Pts',(-1.27426444774527,2.09474237194155,24.3274550764227));
#8477=CARTESIAN_POINT('Ctrl Pts',(-1.20340600096711,2.13622651707175,24.3231756467084));
#8478=CARTESIAN_POINT('Ctrl Pts',(-1.13079124448403,2.17399664475322,24.3188962169941));
#8479=CARTESIAN_POINT('Ctrl Pts',(-1.05900331673324,2.21133670245578,24.3146655150538));
#8480=CARTESIAN_POINT('Ctrl Pts',(-0.985228877900467,2.24518737691167,24.3104348131135));
#8481=CARTESIAN_POINT('Ctrl Pts',(-0.909841187207912,2.27533278094878,24.3062041111732));
#8482=CARTESIAN_POINT('Ctrl Pts',(-0.834561807883372,2.30543487433503,24.3019794875874));
#8483=CARTESIAN_POINT('Ctrl Pts',(-0.757674208128448,2.33184209876887,24.2977548640017));
#8484=CARTESIAN_POINT('Ctrl Pts',(-0.679575786851029,2.35438463296162,24.293530240416));
#8485=CARTESIAN_POINT('Ctrl Pts',(-0.601169985639642,2.37701589010879,24.2892889895477));
#8486=CARTESIAN_POINT('Ctrl Pts',(-0.521544232362832,2.39575175146896,24.2850477386795));
#8487=CARTESIAN_POINT('Ctrl Pts',(-0.441120477794435,2.41046945097224,24.2808064878112));
#8488=CARTESIAN_POINT('Ctrl Pts',(-0.361156588318291,2.42510299429211,24.2765894885242));
#8489=CARTESIAN_POINT('Ctrl Pts',(-0.280404260832229,2.4357641184079,24.2723724892372));
#8490=CARTESIAN_POINT('Ctrl Pts',(-0.199291164988927,2.44238270579313,24.2681554899502));
#8491=CARTESIAN_POINT('Ctrl Pts',(-0.118204959911378,2.44899909897185,24.2639398886908));
#8492=CARTESIAN_POINT('Ctrl Pts',(-0.0367586871396675,2.45157557901672,
24.2597242874313));
#8493=CARTESIAN_POINT('Ctrl Pts',(0.0446143744377594,2.4500938364874,24.2555086861719));
#8494=CARTESIAN_POINT('Ctrl Pts',(0.125985405547148,2.44861213093137,24.2512931901025));
#8495=CARTESIAN_POINT('Ctrl Pts',(0.207282764130744,2.44307241368911,24.2470776940332));
#8496=CARTESIAN_POINT('Ctrl Pts',(0.288074125725909,2.43350848531236,24.2428621979639));
#8497=CARTESIAN_POINT('Ctrl Pts',(0.369721579417327,2.42384321437459,24.2386020330984));
#8498=CARTESIAN_POINT('Ctrl Pts',(0.450851765843265,2.41006798170026,24.2343418682328));
#8499=CARTESIAN_POINT('Ctrl Pts',(0.531026647743397,2.39227108609923,24.2300817033673));
#8500=CARTESIAN_POINT('Ctrl Pts',(0.610476413605104,2.37463514881993,24.2258600681983));
#8501=CARTESIAN_POINT('Ctrl Pts',(0.688987648284235,2.35305018546115,24.2216384330294));
#8502=CARTESIAN_POINT('Ctrl Pts',(0.766148917966809,2.32765248383393,24.2174167978604));
#8503=CARTESIAN_POINT('Ctrl Pts',(0.844366531999536,2.30190708550952,24.2131373681466));
#8504=CARTESIAN_POINT('Ctrl Pts',(0.921196477445402,2.2722439432278,24.2088579384328));
#8505=CARTESIAN_POINT('Ctrl Pts',(0.996232508971911,2.23885484970945,24.2045785087189));
#8506=CARTESIAN_POINT('Ctrl Pts',(1.07126854049844,2.2054657561911,24.2002990790051));
#8507=CARTESIAN_POINT('Ctrl Pts',(1.14451025010084,2.16835099161015,24.1960196492913));
#8508=CARTESIAN_POINT('Ctrl Pts',(1.21558025847346,2.12774878338811,24.1917402195775));
#8509=CARTESIAN_POINT('Ctrl Pts',(1.28584102741354,2.08760889265687,24.1875095176372));
#8510=CARTESIAN_POINT('Ctrl Pts',(1.35424359177118,2.04390963436234,24.183278815697));
#8511=CARTESIAN_POINT('Ctrl Pts',(1.4204043558176,1.99684794513112,24.1790481137567));
#8512=CARTESIAN_POINT('Ctrl Pts',(1.48647006505069,1.94985387059797,24.174823490171));
#8513=CARTESIAN_POINT('Ctrl Pts',(1.55029999500818,1.89950722681738,24.1705988665853));
#8514=CARTESIAN_POINT('Ctrl Pts',(1.61153621068755,1.84605018665333,24.1663742429996));
#8515=CARTESIAN_POINT('Ctrl Pts',(1.67301343999609,1.79238275015581,24.1621329921313));
#8516=CARTESIAN_POINT('Ctrl Pts',(1.73187608249187,1.73558061635585,24.157891741263));
#8517=CARTESIAN_POINT('Ctrl Pts',(1.78779247253049,1.67593207653632,24.1536504903947));
#8518=CARTESIAN_POINT('Ctrl Pts',(1.84338913121596,1.61662460859814,24.1494334911077));
#8519=CARTESIAN_POINT('Ctrl Pts',(1.89607281824978,1.55450354065553,24.1452164918207));
#8520=CARTESIAN_POINT('Ctrl Pts',(1.94555303637773,1.48989047672687,24.1409994925337));
#8521=CARTESIAN_POINT('Ctrl Pts',(1.99501685073089,1.42529883344243,24.1367838912743));
#8522=CARTESIAN_POINT('Ctrl Pts',(2.04127902263956,1.35821720370604,24.1325682900148));
#8523=CARTESIAN_POINT('Ctrl Pts',(2.08408957598101,1.2889999570548,24.1283526887553));
#8524=CARTESIAN_POINT('Ctrl Pts',(2.12689906108861,1.21978443755261,24.124137192686));
#8525=CARTESIAN_POINT('Ctrl Pts',(2.16625685516426,1.14843380318076,24.1199216966167));
#8526=CARTESIAN_POINT('Ctrl Pts',(2.20195731069058,1.07532983400272,24.1157062005473));
#8527=CARTESIAN_POINT('Ctrl Pts',(2.238036060099,1.00145123089103,24.1114460356818));
#8528=CARTESIAN_POINT('Ctrl Pts',(2.27037927363274,0.925782342151553,24.1071858708162));
#8529=CARTESIAN_POINT('Ctrl Pts',(2.29882403061856,0.848739256927979,24.1029257059506));
#8530=CARTESIAN_POINT('Ctrl Pts',(2.32701152811091,0.772392963211155,24.0987040707816));
#8531=CARTESIAN_POINT('Ctrl Pts',(2.35137072031782,0.694697697145301,24.0944824356126));
#8532=CARTESIAN_POINT('Ctrl Pts',(2.37179343710082,0.616073162640177,24.0902608004436));
#8533=CARTESIAN_POINT('Ctrl Pts',(2.3924957426151,0.536372251564608,24.0859813707298));
#8534=CARTESIAN_POINT('Ctrl Pts',(2.4091528752121,0.455716920303052,24.081701941016));
#8535=CARTESIAN_POINT('Ctrl Pts',(2.42170614002903,0.37455256152604,24.0774225113021));
#8536=CARTESIAN_POINT('Ctrl Pts',(2.43425940484595,0.293388202749006,24.0731430815883));
#8537=CARTESIAN_POINT('Ctrl Pts',(2.4427088165426,0.211715311179143,24.0688636518745));
#8538=CARTESIAN_POINT('Ctrl Pts',(2.44705034898911,0.129980150454861,24.0645842221606));
#8539=CARTESIAN_POINT('Ctrl Pts',(2.45134244652859,0.0491756680387825,24.0603535202204));
#8540=CARTESIAN_POINT('Ctrl Pts',(2.45163592503804,-0.0319935986599718,
24.0561228182801));
#8541=CARTESIAN_POINT('Ctrl Pts',(2.44788867719605,-0.113098514823987,24.0518921163399));
#8542=CARTESIAN_POINT('Ctrl Pts',(2.44414681311811,-0.194086905540078,24.0476674927542));
#8543=CARTESIAN_POINT('Ctrl Pts',(2.43637577383816,-0.275010668717048,24.0434428691686));
#8544=CARTESIAN_POINT('Ctrl Pts',(2.42458537776282,-0.355437752551335,24.0392182455829));
#8545=CARTESIAN_POINT('Ctrl Pts',(2.41274857702114,-0.436181381475851,24.0349769947146));
#8546=CARTESIAN_POINT('Ctrl Pts',(2.396860687666,-0.51642393912257,24.0307357438463));
#8547=CARTESIAN_POINT('Ctrl Pts',(2.37698452505334,-0.595730490790041,24.026494492978));
#8548=CARTESIAN_POINT('Ctrl Pts',(2.35722201484881,-0.674583565558943,24.0222774936911));
#8549=CARTESIAN_POINT('Ctrl Pts',(2.33351683191325,-0.752510853870986,24.0180604944042));
#8550=CARTESIAN_POINT('Ctrl Pts',(2.30598208858976,-0.82909399774887,24.0138434951172));
#8551=CARTESIAN_POINT('Ctrl Pts',(2.27845647363606,-0.905651752639155,24.0096278938578));
#8552=CARTESIAN_POINT('Ctrl Pts',(2.24710397669315,-0.980865810720861,24.0054122925984));
#8553=CARTESIAN_POINT('Ctrl Pts',(2.21208719658111,-1.05433414282281,24.001196691339));
#8554=CARTESIAN_POINT('Ctrl Pts',(2.17707129022818,-1.12780064170013,23.9969811952697));
#8555=CARTESIAN_POINT('Ctrl Pts',(2.13839148357112,-1.19952108185924,23.9927656992004));
#8556=CARTESIAN_POINT('Ctrl Pts',(2.09625742106833,-1.26911586335367,23.9885502031312));
#8557=CARTESIAN_POINT('Ctrl Pts',(2.05367689204647,-1.33944809426537,23.9842900382656));
#8558=CARTESIAN_POINT('Ctrl Pts',(2.00756870353918,-1.40760892713529,23.9800298734));
#8559=CARTESIAN_POINT('Ctrl Pts',(1.95819447844173,-1.47323610959015,23.9757697085344));
#8560=CARTESIAN_POINT('Ctrl Pts',(1.90926680270934,-1.53826974801272,23.9715480733654));
#8561=CARTESIAN_POINT('Ctrl Pts',(1.85713227849281,-1.6008150595765,23.9673264381965));
#8562=CARTESIAN_POINT('Ctrl Pts',(1.80208521041733,-1.66055386675505,23.9631048030276));
#8563=CARTESIAN_POINT('Ctrl Pts',(1.74628454329194,-1.72111050329138,23.9588253733136));
#8564=CARTESIAN_POINT('Ctrl Pts',(1.68749133567652,-1.77878286466063,23.9545459435997));
#8565=CARTESIAN_POINT('Ctrl Pts',(1.6260482767155,-1.83328046184716,23.9502665138858));
#8566=CARTESIAN_POINT('Ctrl Pts',(1.56460521775449,-1.88777805903369,23.9459870841718));
#8567=CARTESIAN_POINT('Ctrl Pts',(1.50051273132664,-1.93910063651416,23.9417076544579));
#8568=CARTESIAN_POINT('Ctrl Pts',(1.43414383714884,-1.9870031968691,23.937428224744));
#8569=CARTESIAN_POINT('Ctrl Pts',(1.36853065311727,-2.03436031419173,23.9331975228037));
#8570=CARTESIAN_POINT('Ctrl Pts',(1.30044587424346,-2.07855306101518,23.9289668208635));
#8571=CARTESIAN_POINT('Ctrl Pts',(1.23022750145088,-2.1193136966183,23.9247361189232));
#8572=CARTESIAN_POINT('Ctrl Pts',(1.16011001313893,-2.16001577040363,23.9205114953375));
#8573=CARTESIAN_POINT('Ctrl Pts',(1.08786541773088,-2.19729529471097,23.9162868717519));
#8574=CARTESIAN_POINT('Ctrl Pts',(1.01386228183258,-2.23092660647481,23.9120622481662));
#8575=CARTESIAN_POINT('Ctrl Pts',(0.939567884232503,-2.26469028442799,23.9078209972979));
#8576=CARTESIAN_POINT('Ctrl Pts',(0.863501458712462,-2.29477669322726,23.9035797464296));
#8577=CARTESIAN_POINT('Ctrl Pts',(0.786062688872571,-2.32100316655588,23.8993384955613));
#8578=CARTESIAN_POINT('Ctrl Pts',(0.709066715906454,-2.34707967623679,23.8951214962744));
#8579=CARTESIAN_POINT('Ctrl Pts',(0.630714495145392,-2.36934012240321,23.8909044969874));
#8580=CARTESIAN_POINT('Ctrl Pts',(0.551419004568647,-2.38765310114357,23.8866874977005));
#8581=CARTESIAN_POINT('Ctrl Pts',(0.472149802181747,-2.40596000873086,23.882471896441));
#8582=CARTESIAN_POINT('Ctrl Pts',(0.391938403751396,-2.42032194312577,23.8782562951816));
#8583=CARTESIAN_POINT('Ctrl Pts',(0.311210851255149,-2.43065794715362,23.8740406939222));
#8584=CARTESIAN_POINT('Ctrl Pts',(0.230485313119844,-2.44099369327147,23.8698251978529));
#8585=CARTESIAN_POINT('Ctrl Pts',(0.149244107958652,-2.44730365077036,23.8656097017836));
#8586=CARTESIAN_POINT('Ctrl Pts',(0.0679198912756184,-2.44955855989791,
23.8613942057143));
#8587=CARTESIAN_POINT('Ctrl Pts',(-0.0142660638146256,-2.45183736279141,
23.8571340408487));
#8588=CARTESIAN_POINT('Ctrl Pts',(-0.0965363163014231,-2.44997463881074,
23.8528738759831));
#8589=CARTESIAN_POINT('Ctrl Pts',(-0.178444654041903,-2.44399422164699,
23.8486137111175));
#8590=CARTESIAN_POINT('Ctrl Pts',(-0.259612198056423,-2.43806789245078,
23.8443920759486));
#8591=CARTESIAN_POINT('Ctrl Pts',(-0.340423888303748,-2.42809817162713,
23.8401704407796));
#8592=CARTESIAN_POINT('Ctrl Pts',(-0.420452874624337,-2.41416023292161,
23.8359488056106));
#8593=CARTESIAN_POINT('Ctrl Pts',(-0.501577464582075,-2.40003148264841,
23.8316693758967));
#8594=CARTESIAN_POINT('Ctrl Pts',(-0.581897275366923,-2.38182515070145,
23.8273899461828));
#8595=CARTESIAN_POINT('Ctrl Pts',(-0.660982540191198,-2.35967208136266,
23.8231105164689));
#8596=CARTESIAN_POINT('Ctrl Pts',(-0.740067805015472,-2.33751901202387,
23.818831086755));
#8597=CARTESIAN_POINT('Ctrl Pts',(-0.81791807955301,-2.31141942332912,23.8145516570412));
#8598=CARTESIAN_POINT('Ctrl Pts',(-0.894125423086613,-2.28155428990638,
23.8102722273273));
#8599=CARTESIAN_POINT('Ctrl Pts',(-0.969465030862561,-2.25202921615474,
23.806041525387));
#8600=CARTESIAN_POINT('Ctrl Pts',(-1.04348232106292,-2.21871290277078,23.8018108234467));
#8601=CARTESIAN_POINT('Ctrl Pts',(-1.11576919095807,-2.18174456857552,23.7975801215065));
#8602=CARTESIAN_POINT('Ctrl Pts',(-1.18795220451145,-2.14482934770438,23.7933554979208));
#8603=CARTESIAN_POINT('Ctrl Pts',(-1.2584093248238,-2.10427273670745,23.7891308743351));
#8604=CARTESIAN_POINT('Ctrl Pts',(-1.32675127764851,-2.06026243407437,23.7849062507494));
#8605=CARTESIAN_POINT('Ctrl Pts',(-1.39536221087843,-2.01607891559734,23.7806649998811));
#8606=CARTESIAN_POINT('Ctrl Pts',(-1.46184084931113,-1.96841463423306,23.7764237490129));
#8607=CARTESIAN_POINT('Ctrl Pts',(-1.52581722143069,-1.91750672926734,23.7721824981446));
#8608=CARTESIAN_POINT('Ctrl Pts',(-1.58942777501225,-1.86688991700897,23.7679654988576));
#8609=CARTESIAN_POINT('Ctrl Pts',(-1.65056423310858,-1.81306676722035,23.7637484995706));
#8610=CARTESIAN_POINT('Ctrl Pts',(-1.70889252572217,-1.75631335061,23.7595315002837));
#8611=CARTESIAN_POINT('Ctrl Pts',(-1.7672014812307,-1.69957874899885,23.7553158990242));
#8612=CARTESIAN_POINT('Ctrl Pts',(-1.82270378694922,-1.63991613375571,23.7511002977648));
#8613=CARTESIAN_POINT('Ctrl Pts',(-1.87510071335033,-1.57763987170491,23.7468846965054));
#8614=CARTESIAN_POINT('Ctrl Pts',(-1.92749633231279,-1.5153651636077,23.7426692004361));
#8615=CARTESIAN_POINT('Ctrl Pts',(-1.9767864274444,-1.45047729492946,23.7384537043668));
#8616=CARTESIAN_POINT('Ctrl Pts',(-2.0227121535729,-1.38332418246356,23.7342382082975));
#8617=CARTESIAN_POINT('Ctrl Pts',(-2.06912452394709,-1.31545949331686,23.7299780434319));
#8618=CARTESIAN_POINT('Ctrl Pts',(-2.11210051405413,-1.24528165878774,23.7257178785663));
#8619=CARTESIAN_POINT('Ctrl Pts',(-2.15141857770893,-1.17317873893491,23.7214577137007));
#8620=CARTESIAN_POINT('Ctrl Pts',(-2.19038104173034,-1.10172793084654,23.7172360785318));
#8621=CARTESIAN_POINT('Ctrl Pts',(-2.22575133037728,-1.02838716936309,23.7130144433628));
#8622=CARTESIAN_POINT('Ctrl Pts',(-2.25736154480884,-0.95355603192378,23.7087928081938));
#8623=CARTESIAN_POINT('Ctrl Pts',(-2.28940450576756,-0.877700449841104,
23.7045133784799));
#8624=CARTESIAN_POINT('Ctrl Pts',(-2.31758349228035,-0.800313840879351,
23.700233948766));
#8625=CARTESIAN_POINT('Ctrl Pts',(-2.34177583183151,-0.721828375342686,
23.6959545190522));
#8626=CARTESIAN_POINT('Ctrl Pts',(-2.36596817138266,-0.64334290980602,23.6916750893383));
#8627=CARTESIAN_POINT('Ctrl Pts',(-2.38617380672403,-0.563759079312216,
23.6873956596243));
#8628=CARTESIAN_POINT('Ctrl Pts',(-2.40232402969862,-0.483517844895685,
23.6831162299104));
#8629=CARTESIAN_POINT('Ctrl Pts',(-2.42528233781748,-0.369451123558754,
23.6770328175576));
#8630=CARTESIAN_POINT('Ctrl Pts',(-2.44012249745692,-0.253699812642377,
23.6709494052048));
#8631=CARTESIAN_POINT('Ctrl Pts',(-2.44665526989246,-0.137216035168911,
23.664865992852));
#8632=CARTESIAN_POINT('Ctrl Pts',(-2.44917473836235,-0.0922921980852357,
23.6625198273054));
#8633=CARTESIAN_POINT('Ctrl Pts',(-2.45045903119537,-0.0472596765065585,
23.6601736617587));
#8634=CARTESIAN_POINT('Ctrl Pts',(-2.45049903536283,-0.00217432422771299,
23.6578274962121));
#8635=CARTESIAN_POINT('',(-2.45049999653667,-0.000130283473732951,22.8578274962385));
#8636=CARTESIAN_POINT('Ctrl Pts',(-2.45049903536358,-0.00217432338460544,
23.6578274961682));
#8637=CARTESIAN_POINT('Ctrl Pts',(-2.45057140723685,0.0793899953797731,
23.6535830268485));
#8638=CARTESIAN_POINT('Ctrl Pts',(-2.44656693668155,0.161087169591102,23.6493385575287));
#8639=CARTESIAN_POINT('Ctrl Pts',(-2.43847466509949,0.242469704639374,23.6450940882089));
#8640=CARTESIAN_POINT('Ctrl Pts',(-2.43054759010129,0.32219088704529,23.6409362659851));
#8641=CARTESIAN_POINT('Ctrl Pts',(-2.41869807736882,0.401609652003178,23.6367784437612));
#8642=CARTESIAN_POINT('Ctrl Pts',(-2.40296835781629,0.48030544587134,23.6326206215373));
#8643=CARTESIAN_POINT('Ctrl Pts',(-2.38724644125954,0.558962201348212,23.6284648618721));
#8644=CARTESIAN_POINT('Ctrl Pts',(-2.36764823011024,0.636896227555752,23.6243091022069));
#8645=CARTESIAN_POINT('Ctrl Pts',(-2.34426744405512,0.713694893314566,23.6201533425417));
#8646=CARTESIAN_POINT('Ctrl Pts',(-2.32089060445998,0.790480596170412,23.6159982843302));
#8647=CARTESIAN_POINT('Ctrl Pts',(-2.29373259783618,0.866130860354779,23.6118432261187));
#8648=CARTESIAN_POINT('Ctrl Pts',(-2.26293718669771,0.94024759455191,23.6076881679072));
#8649=CARTESIAN_POINT('Ctrl Pts',(-2.23098851599881,1.01713993164378,23.6033775066228));
#8650=CARTESIAN_POINT('Ctrl Pts',(-2.1951248041455,1.09238108773871,23.5990668453383));
#8651=CARTESIAN_POINT('Ctrl Pts',(-2.15556071890065,1.1655506154314,23.5947561840539));
#8652=CARTESIAN_POINT('Ctrl Pts',(-2.11737709415898,1.23616712964251,23.5905959293214));
#8653=CARTESIAN_POINT('Ctrl Pts',(-2.07574736520934,1.30485380286194,23.586435674589));
#8654=CARTESIAN_POINT('Ctrl Pts',(-2.03090962191127,1.37126086417874,23.5822754198566));
#8655=CARTESIAN_POINT('Ctrl Pts',(-1.98604163029131,1.4377127248547,23.5781123585439));
#8656=CARTESIAN_POINT('Ctrl Pts',(-1.93796161023225,1.50188153438619,23.5739492972312));
#8657=CARTESIAN_POINT('Ctrl Pts',(-1.88694812386953,1.56345035988523,23.5697862359186));
#8658=CARTESIAN_POINT('Ctrl Pts',(-1.83585604644476,1.62511403793661,23.5656167610193));
#8659=CARTESIAN_POINT('Ctrl Pts',(-1.78182181869754,1.68416939772165,23.5614472861201));
#8660=CARTESIAN_POINT('Ctrl Pts',(-1.72516030602709,1.74033679743563,23.5572778112209));
#8661=CARTESIAN_POINT('Ctrl Pts',(-1.71919184832368,1.7462532076002,23.5568386183118));
#8662=CARTESIAN_POINT('Ctrl Pts',(-1.71319426844774,1.75213761220009,23.5563994254028));
#8663=CARTESIAN_POINT('Ctrl Pts',(-1.70716795431091,1.75798971150968,23.5559602324937));
#8664=CARTESIAN_POINT('Ctrl Pts',(-1.64911706508791,1.81436240649869,23.5517295305535));
#8665=CARTESIAN_POINT('Ctrl Pts',(-1.58816176517418,1.86796266208168,23.5474988286132));
#8666=CARTESIAN_POINT('Ctrl Pts',(-1.52459764933914,1.91847654602019,23.5432681266729));
#8667=CARTESIAN_POINT('Ctrl Pts',(-1.46112485764856,1.96891785540664,23.5390435030873));
#8668=CARTESIAN_POINT('Ctrl Pts',(-1.39505105507288,2.01628131296052,23.5348188795016));
#8669=CARTESIAN_POINT('Ctrl Pts',(-1.32670818167451,2.0602901860364,23.5305942559159));
#8670=CARTESIAN_POINT('Ctrl Pts',(-1.2580963242478,2.10447226932974,23.5263530050476));
#8671=CARTESIAN_POINT('Ctrl Pts',(-1.1871978369066,2.14527297494325,23.5221117541793));
#8672=CARTESIAN_POINT('Ctrl Pts',(-1.11438168379101,2.18245359923896,23.5178705033111));
#8673=CARTESIAN_POINT('Ctrl Pts',(-1.04198189530796,2.21942162377061,23.5136535040241));
#8674=CARTESIAN_POINT('Ctrl Pts',(-0.9676867304183,2.25281064046416,23.5094365047371));
#8675=CARTESIAN_POINT('Ctrl Pts',(-0.891885741999468,2.2824307378797,23.5052195054502));
#8676=CARTESIAN_POINT('Ctrl Pts',(-0.816109883266569,2.31204101558496,23.5010039041907));
#8677=CARTESIAN_POINT('Ctrl Pts',(-0.738829625178347,2.3378846861362,23.4967883029313));
#8678=CARTESIAN_POINT('Ctrl Pts',(-0.660454763102909,2.35981985666166,23.4925727016719));
#8679=CARTESIAN_POINT('Ctrl Pts',(-0.582081856682689,2.38175447984798,23.4883572056026));
#8680=CARTESIAN_POINT('Ctrl Pts',(-0.502614848724108,2.39978067261914,23.4841417095333));
#8681=CARTESIAN_POINT('Ctrl Pts',(-0.422477576214879,2.4138067336876,23.4799262134639));
#8682=CARTESIAN_POINT('Ctrl Pts',(-0.341491142553382,2.42798141955705,23.4756660485984));
#8683=CARTESIAN_POINT('Ctrl Pts',(-0.259820629507715,2.43807059611962,23.4714058837328));
#8684=CARTESIAN_POINT('Ctrl Pts',(-0.177910987857276,2.44403312792598,23.4671457188672));
#8685=CARTESIAN_POINT('Ctrl Pts',(-0.0967421517253367,2.4499417335232,23.4629240836983));
#8686=CARTESIAN_POINT('Ctrl Pts',(-0.0153389665478567,2.45179808934017,
23.4587024485293));
#8687=CARTESIAN_POINT('Ctrl Pts',(0.06586532795961,2.44961466532448,23.4544808133603));
#8688=CARTESIAN_POINT('Ctrl Pts',(0.148181316173007,2.44740135004811,23.4502013836464));
#8689=CARTESIAN_POINT('Ctrl Pts',(0.230292433649477,2.44103684580901,23.4459219539326));
#8690=CARTESIAN_POINT('Ctrl Pts',(0.311754480614958,2.43058828142828,23.4416425242187));
#8691=CARTESIAN_POINT('Ctrl Pts',(0.393216527580415,2.42013971704755,23.4373630945048));
#8692=CARTESIAN_POINT('Ctrl Pts',(0.474029032783694,2.40560724381203,23.4330836647909));
#8693=CARTESIAN_POINT('Ctrl Pts',(0.553762120999265,2.38711075640541,23.428804235077));
#8694=CARTESIAN_POINT('Ctrl Pts',(0.632587327526426,2.36882487945665,23.4245735331368));
#8695=CARTESIAN_POINT('Ctrl Pts',(0.710654067120783,2.34659606583175,23.4203428311965));
#8696=CARTESIAN_POINT('Ctrl Pts',(0.787538360381237,2.320502872424,23.4161121292563));
#8697=CARTESIAN_POINT('Ctrl Pts',(0.86431219206763,2.29444716775541,23.4118875056706));
#8698=CARTESIAN_POINT('Ctrl Pts',(0.939906514776988,2.26453825817395,23.4076628820849));
#8699=CARTESIAN_POINT('Ctrl Pts',(1.01390894717371,2.23090539845174,23.4034382584993));
#8700=CARTESIAN_POINT('Ctrl Pts',(1.08820263850347,2.19714016644769,23.399197007631));
#8701=CARTESIAN_POINT('Ctrl Pts',(1.1608914196349,2.15962171520747,23.3949557567627));
#8702=CARTESIAN_POINT('Ctrl Pts',(1.23157483713222,2.11853101713021,23.3907145058944));
#8703=CARTESIAN_POINT('Ctrl Pts',(1.30185408503381,2.07767527671937,23.3864975066075));
#8704=CARTESIAN_POINT('Ctrl Pts',(1.37015043441059,2.03328826709363,23.3822805073205));
#8705=CARTESIAN_POINT('Ctrl Pts',(1.43609330724811,1.98559468746197,23.3780635080335));
#8706=CARTESIAN_POINT('Ctrl Pts',(1.50201431858061,1.93791691929538,23.3738479067741));
#8707=CARTESIAN_POINT('Ctrl Pts',(1.56558302624488,1.88693503031906,23.3696323055147));
#8708=CARTESIAN_POINT('Ctrl Pts',(1.62645826467462,1.83291673658997,23.3654167042552));
#8709=CARTESIAN_POINT('Ctrl Pts',(1.68733198410993,1.77889979075683,23.361201208186));
#8710=CARTESIAN_POINT('Ctrl Pts',(1.7455120208046,1.72184690029657,23.3569857121167));
#8711=CARTESIAN_POINT('Ctrl Pts',(1.80069180584515,1.66206476118175,23.3527702160474));
#8712=CARTESIAN_POINT('Ctrl Pts',(1.856456294213,1.60164915066742,23.3485100511818));
#8713=CARTESIAN_POINT('Ctrl Pts',(1.90915622857819,1.53844645212694,23.3442498863162));
#8714=CARTESIAN_POINT('Ctrl Pts',(1.9585161223792,1.47280849005591,23.3399897214506));
#8715=CARTESIAN_POINT('Ctrl Pts',(2.00742959643023,1.40776416950959,23.3357680862816));
#8716=CARTESIAN_POINT('Ctrl Pts',(2.05306299034284,1.34032888220443,23.3315464511127));
#8717=CARTESIAN_POINT('Ctrl Pts',(2.0951922272049,1.27087362906788,23.3273248159437));
#8718=CARTESIAN_POINT('Ctrl Pts',(2.13789821690709,1.20046752760149,23.3230453862298));
#8719=CARTESIAN_POINT('Ctrl Pts',(2.17700314381538,1.1279861698671,23.3187659565159));
#8720=CARTESIAN_POINT('Ctrl Pts',(2.21232295197123,1.05383936450548,23.314486526802));
#8721=CARTESIAN_POINT('Ctrl Pts',(2.24764276012706,0.979692559143882,23.3102070970881));
#8722=CARTESIAN_POINT('Ctrl Pts',(2.27917732158504,0.903880784271508,23.3059276673742));
#8723=CARTESIAN_POINT('Ctrl Pts',(2.30679469916284,0.826830373120286,23.3016482376603));
#8724=CARTESIAN_POINT('Ctrl Pts',(2.33409761116615,0.750657297325703,23.29741753572));
#8725=CARTESIAN_POINT('Ctrl Pts',(2.35767482651362,0.672987155684556,23.2931868337798));
#8726=CARTESIAN_POINT('Ctrl Pts',(2.37736284503384,0.594218943700571,23.2889561318395));
#8727=CARTESIAN_POINT('Ctrl Pts',(2.39702257728873,0.515563899963611,23.2847315082538));
#8728=CARTESIAN_POINT('Ctrl Pts',(2.4128040983922,0.435814366485919,23.2805068846682));
#8729=CARTESIAN_POINT('Ctrl Pts',(2.42459281212596,0.355387036042603,23.2762822610825));
#8730=CARTESIAN_POINT('Ctrl Pts',(2.43642792390465,0.274643159538683,23.2720410102142));
#8731=CARTESIAN_POINT('Ctrl Pts',(2.4442385709811,0.193216586000986,23.2677997593459));
#8732=CARTESIAN_POINT('Ctrl Pts',(2.44796009702725,0.111541980269029,23.2635585084776));
#8733=CARTESIAN_POINT('Ctrl Pts',(2.45166034329194,0.0303343920291857,23.2593415091907));
#8734=CARTESIAN_POINT('Ctrl Pts',(2.45131808364673,-0.0511179303445025,
23.2551245099037));
#8735=CARTESIAN_POINT('Ctrl Pts',(2.44692160031491,-0.132381765784869,23.2509075106168));
#8736=CARTESIAN_POINT('Ctrl Pts',(2.4425265745135,-0.213618660485914,23.2466919093573));
#8737=CARTESIAN_POINT('Ctrl Pts',(2.4340800192119,-0.294666728329954,23.2424763080979));
#8738=CARTESIAN_POINT('Ctrl Pts',(2.42162230761982,-0.375094187155815,23.2382607068385));
#8739=CARTESIAN_POINT('Ctrl Pts',(2.4091649068798,-0.455519639108869,23.2340452107692));
#8740=CARTESIAN_POINT('Ctrl Pts',(2.39269662110869,-0.535324053419385,23.2298297146999));
#8741=CARTESIAN_POINT('Ctrl Pts',(2.37230932721114,-0.614083631134233,23.2256142186306));
#8742=CARTESIAN_POINT('Ctrl Pts',(2.35170600277696,-0.693677771490152,23.221354053765));
#8743=CARTESIAN_POINT('Ctrl Pts',(2.32710022727633,-0.772204327488093,23.2170938888994));
#8744=CARTESIAN_POINT('Ctrl Pts',(2.29863864811276,-0.84924119977917,23.2128337240338));
#8745=CARTESIAN_POINT('Ctrl Pts',(2.27043448058587,-0.925581336753225,23.2086120888649));
#8746=CARTESIAN_POINT('Ctrl Pts',(2.2384442155249,-1.00045821940249,23.2043904536959));
#8747=CARTESIAN_POINT('Ctrl Pts',(2.20285845685593,-1.07348258908019,23.200168818527));
#8748=CARTESIAN_POINT('Ctrl Pts',(2.16678552612065,-1.14750666859682,23.1958893888131));
#8749=CARTESIAN_POINT('Ctrl Pts',(2.12701815000943,-1.21962669580652,23.1916099590992));
#8750=CARTESIAN_POINT('Ctrl Pts',(2.08380122814361,-1.28946604902462,23.1873305293853));
#8751=CARTESIAN_POINT('Ctrl Pts',(2.04058430627781,-1.3593054022427,23.1830510996714));
#8752=CARTESIAN_POINT('Ctrl Pts',(1.99391817136626,-1.42686371504018,23.1787716699575));
#8753=CARTESIAN_POINT('Ctrl Pts',(1.94408983392752,-1.49179923837616,23.1744922402436));
#8754=CARTESIAN_POINT('Ctrl Pts',(1.89482886740259,-1.55599537265948,23.1702615383033));
#8755=CARTESIAN_POINT('Ctrl Pts',(1.84229209519892,-1.61786962863514,23.1660308363631));
#8756=CARTESIAN_POINT('Ctrl Pts',(1.78672645485823,-1.67706852141161,23.1618001344228));
#8757=CARTESIAN_POINT('Ctrl Pts',(1.7312406470534,-1.7361823616682,23.1575755108371));
#8758=CARTESIAN_POINT('Ctrl Pts',(1.67273492930474,-1.79262813643478,23.1533508872514));
#8759=CARTESIAN_POINT('Ctrl Pts',(1.61149759544756,-1.84608389567396,23.1491262636657));
#8760=CARTESIAN_POINT('Ctrl Pts',(1.55001924355995,-1.89975004620543,23.1448850127975));
#8761=CARTESIAN_POINT('Ctrl Pts',(1.48578801613983,-1.95040221802397,23.1406437619292));
#8762=CARTESIAN_POINT('Ctrl Pts',(1.41913435521906,-1.99775071814203,23.1364025110609));
#8763=CARTESIAN_POINT('Ctrl Pts',(1.35286182164231,-2.04482847832105,23.1321855117739));
#8764=CARTESIAN_POINT('Ctrl Pts',(1.28419486541242,-2.08863997320375,23.127968512487));
#8765=CARTESIAN_POINT('Ctrl Pts',(1.21349137625761,-2.12894079996331,23.1237515132));
#8766=CARTESIAN_POINT('Ctrl Pts',(1.14281132685615,-2.16922826611719,23.1195359119406));
#8767=CARTESIAN_POINT('Ctrl Pts',(1.07009648898759,-2.2060071452667,23.1153203106811));
#8768=CARTESIAN_POINT('Ctrl Pts',(0.995731745286284,-2.23907760951449,23.1111047094217));
#8769=CARTESIAN_POINT('Ctrl Pts',(0.921368857177361,-2.2721472485688,23.1068892133524));
#8770=CARTESIAN_POINT('Ctrl Pts',(0.845356570467875,-2.30150846872244,23.1026737172831));
#8771=CARTESIAN_POINT('Ctrl Pts',(0.768100940560529,-2.32700906640048,23.0984582212138));
#8772=CARTESIAN_POINT('Ctrl Pts',(0.690026684342956,-2.35277987687998,23.0941980563482));
#8773=CARTESIAN_POINT('Ctrl Pts',(0.610683033283608,-2.37460759369635,23.0899378914826));
#8774=CARTESIAN_POINT('Ctrl Pts',(0.530504267227015,-2.39238698216947,23.085677726617));
#8775=CARTESIAN_POINT('Ctrl Pts',(0.451050652338985,-2.41000557065823,23.0814560914481));
#8776=CARTESIAN_POINT('Ctrl Pts',(0.370777441475839,-2.42364874593649,23.0772344562791));
#8777=CARTESIAN_POINT('Ctrl Pts',(0.290115101996816,-2.43326601044633,23.0730128211101));
#8778=CARTESIAN_POINT('Ctrl Pts',(0.208348488222393,-2.44301493612616,23.0687333913963));
#8779=CARTESIAN_POINT('Ctrl Pts',(0.126182504256642,-2.44862685258757,23.0644539616824));
#8780=CARTESIAN_POINT('Ctrl Pts',(0.044066389170475,-2.45010375358789,23.0601745319685));
#8781=CARTESIAN_POINT('Ctrl Pts',(-0.0380497259157154,-2.45158065458821,
23.0558951022546));
#8782=CARTESIAN_POINT('Ctrl Pts',(-0.120115483911881,-2.44892262146589,
23.0516156725407));
#8783=CARTESIAN_POINT('Ctrl Pts',(-0.201688165846101,-2.44218593349434,
23.0473362428268));
#8784=CARTESIAN_POINT('Ctrl Pts',(-0.282332019538064,-2.43552595289466,
23.0431055408866));
#8785=CARTESIAN_POINT('Ctrl Pts',(-0.362797296576456,-2.42485472160483,
23.0388748389463));
#8786=CARTESIAN_POINT('Ctrl Pts',(-0.442653106969058,-2.41018847331296,
23.0346441370061));
#8787=CARTESIAN_POINT('Ctrl Pts',(-0.522394186534937,-2.39554329638437,
23.0304195134204));
#8788=CARTESIAN_POINT('Ctrl Pts',(-0.601527084987009,-2.37691458518828,
23.0261948898347));
#8789=CARTESIAN_POINT('Ctrl Pts',(-0.679625034711575,-2.35437041737134,
23.021970266249));
#8790=CARTESIAN_POINT('Ctrl Pts',(-0.75803036251502,-2.33173752017011,23.0177290153807));
#8791=CARTESIAN_POINT('Ctrl Pts',(-0.835392104466457,-2.30515831837483,
23.0134877645124));
#8792=CARTESIAN_POINT('Ctrl Pts',(-0.911287793776614,-2.27475379039441,
23.0092465136442));
#8793=CARTESIAN_POINT('Ctrl Pts',(-0.986749509586992,-2.2445231162855,23.0050295143572));
#8794=CARTESIAN_POINT('Ctrl Pts',(-1.06076145706714,-2.21051091859256,23.0008125150703));
#8795=CARTESIAN_POINT('Ctrl Pts',(-1.13292438696317,-2.17288577321131,22.9965955157833));
#8796=CARTESIAN_POINT('Ctrl Pts',(-1.20506339326933,-2.13527310138883,22.9923799145239));
#8797=CARTESIAN_POINT('Ctrl Pts',(-1.2753541872375,-2.09405007528642,22.9881643132644));
#8798=CARTESIAN_POINT('Ctrl Pts',(-1.34342038204196,-2.04943209868349,22.983948712005));
#8799=CARTESIAN_POINT('Ctrl Pts',(-1.41148487841883,-2.00481523541447,22.9797332159357));
#8800=CARTESIAN_POINT('Ctrl Pts',(-1.47732449764834,-1.95680384593917,22.9755177198664));
#8801=CARTESIAN_POINT('Ctrl Pts',(-1.54059143022449,-1.90565691957363,22.9713022237972));
#8802=CARTESIAN_POINT('Ctrl Pts',(-1.60452876022909,-1.85396802339049,22.9670420589316));
#8803=CARTESIAN_POINT('Ctrl Pts',(-1.66583816997758,-1.79907703632353,22.962781894066));
#8804=CARTESIAN_POINT('Ctrl Pts',(-1.72419605836845,-1.74129210711664,22.9585217292004));
#8805=CARTESIAN_POINT('Ctrl Pts',(-1.78202614752932,-1.68402979519393,22.9543000940314));
#8806=CARTESIAN_POINT('Ctrl Pts',(-1.83695761709659,-1.62392606598259,22.9500784588624));
#8807=CARTESIAN_POINT('Ctrl Pts',(-1.88871495074073,-1.56131549817724,22.9458568236935));
#8808=CARTESIAN_POINT('Ctrl Pts',(-1.94118084668974,-1.49784778636717,22.9415773939796));
#8809=CARTESIAN_POINT('Ctrl Pts',(-1.99038474476822,-1.4318044752645,22.9372979642657));
#8810=CARTESIAN_POINT('Ctrl Pts',(-2.03608509788774,-1.36356434544157,22.9330185345518));
#8811=CARTESIAN_POINT('Ctrl Pts',(-2.08178545100725,-1.29532421561863,22.9287391048379));
#8812=CARTESIAN_POINT('Ctrl Pts',(-2.12398206323083,-1.22488772157964,22.9244596751239));
#8813=CARTESIAN_POINT('Ctrl Pts',(-2.16248255848491,-1.15265755289616,22.92018024541));
#8814=CARTESIAN_POINT('Ctrl Pts',(-2.20267916262551,-1.07724534122413,22.9157122888027));
#8815=CARTESIAN_POINT('Ctrl Pts',(-2.23898476198766,-0.99962042806452,22.9112443321953));
#8816=CARTESIAN_POINT('Ctrl Pts',(-2.27116419083332,-0.920197515904305,
22.9067763755879));
#8817=CARTESIAN_POINT('Ctrl Pts',(-2.30324859241746,-0.841009143079146,
22.9023216130519));
#8818=CARTESIAN_POINT('Ctrl Pts',(-2.33123095314875,-0.760033706883554,
22.8978668505159));
#8819=CARTESIAN_POINT('Ctrl Pts',(-2.35492280758172,-0.677708506905027,
22.8934120879799));
#8820=CARTESIAN_POINT('Ctrl Pts',(-2.37857232061475,-0.595530436152999,
22.8889652868673));
#8821=CARTESIAN_POINT('Ctrl Pts',(-2.39794647646271,-0.512007771438047,
22.8845184857546));
#8822=CARTESIAN_POINT('Ctrl Pts',(-2.4129051813671,-0.42759658058948,22.8800716846419));
#8823=CARTESIAN_POINT('Ctrl Pts',(-2.42782859230941,-0.343384551726377,
22.8756353754288));
#8824=CARTESIAN_POINT('Ctrl Pts',(-2.4383572374736,-0.258288553180677,22.8711990662157));
#8825=CARTESIAN_POINT('Ctrl Pts',(-2.44440142582957,-0.172777080083969,
22.8667627570026));
#8826=CARTESIAN_POINT('Ctrl Pts',(-2.44845933346359,-0.115366946739541,
22.8637843367479));
#8827=CARTESIAN_POINT('Ctrl Pts',(-2.45049693206645,-0.0577698600959872,
22.8608059164932));
#8828=CARTESIAN_POINT('Ctrl Pts',(-2.45049999653667,-0.000130283473727266,
22.8578274962385));
#8829=CARTESIAN_POINT('',(-2.45049898498603,0.00223037720034039,22.0578274962121));
#8830=CARTESIAN_POINT('Ctrl Pts',(-2.4504999965367,-0.000130282961934726,
22.8578274962121));
#8831=CARTESIAN_POINT('Ctrl Pts',(-2.45050452194915,0.084988469602718,22.8534291395352));
#8832=CARTESIAN_POINT('Ctrl Pts',(-2.44606980392823,0.170029198438209,22.8490307828582));
#8833=CARTESIAN_POINT('Ctrl Pts',(-2.43724598391114,0.254523601870292,22.8446324261812));
#8834=CARTESIAN_POINT('Ctrl Pts',(-2.42839970581659,0.339233057496683,22.840222874961));
#8835=CARTESIAN_POINT('Ctrl Pts',(-2.41514204232535,0.42339300592857,22.8358133237408));
#8836=CARTESIAN_POINT('Ctrl Pts',(-2.39757477354423,0.506542649008293,22.8314037725206));
#8837=CARTESIAN_POINT('Ctrl Pts',(-2.37998497661336,0.589798922642478,22.826988566521));
#8838=CARTESIAN_POINT('Ctrl Pts',(-2.35807465958574,0.672041917853691,22.8225733605213));
#8839=CARTESIAN_POINT('Ctrl Pts',(-2.33199555061119,0.752826010396555,22.8181581545217));
#8840=CARTESIAN_POINT('Ctrl Pts',(-2.30584599539508,0.833828321119468,22.8137310219386));
#8841=CARTESIAN_POINT('Ctrl Pts',(-2.27550527632207,0.913363470995812,22.8093038893556));
#8842=CARTESIAN_POINT('Ctrl Pts',(-2.24117371120737,0.991004866886629,22.8048767567725));
#8843=CARTESIAN_POINT('Ctrl Pts',(-2.21053573284011,1.06029315595121,22.8009259205128));
#8844=CARTESIAN_POINT('Ctrl Pts',(-2.17672019184988,1.12807340583439,22.7969750842531));
#8845=CARTESIAN_POINT('Ctrl Pts',(-2.1398991839799,1.19406102540956,22.7930242479933));
#8846=CARTESIAN_POINT('Ctrl Pts',(-2.10046988365024,1.26472301487648,22.7887935460531));
#8847=CARTESIAN_POINT('Ctrl Pts',(-2.05746265756872,1.33356278892397,22.7845628441128));
#8848=CARTESIAN_POINT('Ctrl Pts',(-2.01107056395171,1.40019478530916,22.7803321421725));
#8849=CARTESIAN_POINT('Ctrl Pts',(-1.96474512300802,1.46673104984992,22.7761075185868));
#8850=CARTESIAN_POINT('Ctrl Pts',(-1.91504473643611,1.53106545800698,22.7718828950011));
#8851=CARTESIAN_POINT('Ctrl Pts',(-1.86220795516667,1.59283765077109,22.7676582714155));
#8852=CARTESIAN_POINT('Ctrl Pts',(-1.80916321877987,1.65485296666434,22.7634170205472));
#8853=CARTESIAN_POINT('Ctrl Pts',(-1.75295757752181,1.71428544075555,22.7591757696789));
#8854=CARTESIAN_POINT('Ctrl Pts',(-1.69387596331198,1.77080051697359,22.7549345188106));
#8855=CARTESIAN_POINT('Ctrl Pts',(-1.63513217928856,1.82699243853532,22.7507175195236));
#8856=CARTESIAN_POINT('Ctrl Pts',(-1.57354556228278,1.88029991050268,22.7465005202367));
#8857=CARTESIAN_POINT('Ctrl Pts',(-1.50943477042091,1.93042920715689,22.7422835209497));
#8858=CARTESIAN_POINT('Ctrl Pts',(-1.44534523268907,1.9805418848526,22.7380679196903));
#8859=CARTESIAN_POINT('Ctrl Pts',(-1.37873354795214,2.02747819333838,22.7338523184308));
#8860=CARTESIAN_POINT('Ctrl Pts',(-1.30995154682697,2.0709845955404,22.7296367171714));
#8861=CARTESIAN_POINT('Ctrl Pts',(-1.24117126199038,2.11448991214531,22.7254212211021));
#8862=CARTESIAN_POINT('Ctrl Pts',(-1.17022116205443,2.15456524494254,22.7212057250328));
#8863=CARTESIAN_POINT('Ctrl Pts',(-1.09748093380322,2.19100110678621,22.7169902289634));
#8864=CARTESIAN_POINT('Ctrl Pts',(-1.02396992593742,2.22782305512183,22.7127300640979));
#8865=CARTESIAN_POINT('Ctrl Pts',(-0.948631052227707,2.26092771178783,22.7084698992323));
#8866=CARTESIAN_POINT('Ctrl Pts',(-0.871878737675352,2.29014796831769,22.7042097343668));
#8867=CARTESIAN_POINT('Ctrl Pts',(-0.795820584848088,2.31910395159665,22.6999880991978));
#8868=CARTESIAN_POINT('Ctrl Pts',(-0.718374921475555,2.34424542806036,22.6957664640288));
#8869=CARTESIAN_POINT('Ctrl Pts',(-0.639960339276593,2.36546000053964,22.6915448288598));
#8870=CARTESIAN_POINT('Ctrl Pts',(-0.560472254771274,2.38696500232232,22.687265399146));
#8871=CARTESIAN_POINT('Ctrl Pts',(-0.479989004804867,2.40443466179886,22.6829859694321));
#8872=CARTESIAN_POINT('Ctrl Pts',(-0.398955367487334,2.41780579549993,22.6787065397183));
#8873=CARTESIAN_POINT('Ctrl Pts',(-0.317921730169778,2.431176929201,22.6744271100044));
#8874=CARTESIAN_POINT('Ctrl Pts',(-0.236338200346401,2.4404495467966,22.6701476802905));
#8875=CARTESIAN_POINT('Ctrl Pts',(-0.154650978361124,2.44561512198709,22.6658682505767));
#8876=CARTESIAN_POINT('Ctrl Pts',(-0.0738938888293157,2.45072187929874,
22.6616375486364));
#8877=CARTESIAN_POINT('Ctrl Pts',(0.00726829076783438,2.45183389960285,
22.6574068466961));
#8878=CARTESIAN_POINT('Ctrl Pts',(0.0884068720686381,2.44890475008136,22.6531761447559));
#8879=CARTESIAN_POINT('Ctrl Pts',(0.169428879553817,2.44597980894175,22.6489515211702));
#8880=CARTESIAN_POINT('Ctrl Pts',(0.250426895264045,2.43902524574514,22.6447268975845));
#8881=CARTESIAN_POINT('Ctrl Pts',(0.330968790351451,2.42804652134453,22.6405022739989));
#8882=CARTESIAN_POINT('Ctrl Pts',(0.411827682403187,2.41702458685676,22.6362610231306));
#8883=CARTESIAN_POINT('Ctrl Pts',(0.492226382121897,2.40194671666979,22.6320197722623));
#8884=CARTESIAN_POINT('Ctrl Pts',(0.571729343457272,2.38287133681823,22.627778521394));
#8885=CARTESIAN_POINT('Ctrl Pts',(0.650777704819028,2.36390503047831,22.623561522107));
#8886=CARTESIAN_POINT('Ctrl Pts',(0.728940086938699,2.34098691574088,22.6193445228201));
#8887=CARTESIAN_POINT('Ctrl Pts',(0.805797012423965,2.31422588023914,22.6151275235331));
#8888=CARTESIAN_POINT('Ctrl Pts',(0.882628458157017,2.28747371660613,22.6109119222737));
#8889=CARTESIAN_POINT('Ctrl Pts',(0.958154867847997,2.25688131498546,22.6066963210142));
#8890=CARTESIAN_POINT('Ctrl Pts',(1.0319725930308,2.22260721163981,22.6024807197548));
#8891=CARTESIAN_POINT('Ctrl Pts',(1.10578847627069,2.18833396352156,22.5982652236855));
#8892=CARTESIAN_POINT('Ctrl Pts',(1.17789533841985,2.15037939316835,22.5940497276162));
#8893=CARTESIAN_POINT('Ctrl Pts',(1.24791148466156,2.10894930627784,22.5898342315469));
#8894=CARTESIAN_POINT('Ctrl Pts',(1.31866954524065,2.06708021242804,22.5855740666813));
#8895=CARTESIAN_POINT('Ctrl Pts',(1.38729189310486,2.0216617408722,22.5813139018157));
#8896=CARTESIAN_POINT('Ctrl Pts',(1.45341365594862,1.97295184804446,22.5770537369501));
#8897=CARTESIAN_POINT('Ctrl Pts',(1.51893740168683,1.92468249624087,22.5728321017811));
#8898=CARTESIAN_POINT('Ctrl Pts',(1.5820052867698,1.87318136532992,22.5686104666122));
#8899=CARTESIAN_POINT('Ctrl Pts',(1.64229618191657,1.81873953628942,22.5643888314432));
#8900=CARTESIAN_POINT('Ctrl Pts',(1.7034124645515,1.76355239397379,22.5601094017293));
#8901=CARTESIAN_POINT('Ctrl Pts',(1.76167479715434,1.70534377668101,22.5558299720154));
#8902=CARTESIAN_POINT('Ctrl Pts',(1.81678924961015,1.64445342667434,22.5515505423015));
#8903=CARTESIAN_POINT('Ctrl Pts',(1.87190370206598,1.58356307666765,22.5472711125876));
#8904=CARTESIAN_POINT('Ctrl Pts',(1.9238700145898,1.51999141522742,22.5429916828737));
#8905=CARTESIAN_POINT('Ctrl Pts',(1.97243944047894,1.45410897240995,22.5387122531598));
#8906=CARTESIAN_POINT('Ctrl Pts',(2.02045583006456,1.38897670075419,22.5344815512196));
#8907=CARTESIAN_POINT('Ctrl Pts',(2.06533293501886,1.32134104863914,22.5302508492793));
#8908=CARTESIAN_POINT('Ctrl Pts',(2.10679961964328,1.25153729975216,22.5260201473391));
#8909=CARTESIAN_POINT('Ctrl Pts',(2.14820672805173,1.18183383964535,22.5217955237534));
#8910=CARTESIAN_POINT('Ctrl Pts',(2.18621291196964,1.10996886568542,22.5175709001677));
#8911=CARTESIAN_POINT('Ctrl Pts',(2.22058880297282,1.03630865002264,22.513346276582));
#8912=CARTESIAN_POINT('Ctrl Pts',(2.25509999068188,0.962358522324323,22.5091050257138));
#8913=CARTESIAN_POINT('Ctrl Pts',(2.2859519663582,0.886599373156029,22.5048637748455));
#8914=CARTESIAN_POINT('Ctrl Pts',(2.3129580423386,0.80942902368347,22.5006225239772));
#8915=CARTESIAN_POINT('Ctrl Pts',(2.33980969688332,0.732699936250112,22.4964055246902));
#8916=CARTESIAN_POINT('Ctrl Pts',(2.36285915913093,0.654576186648453,22.4921885254033));
#8917=CARTESIAN_POINT('Ctrl Pts',(2.38197086714868,0.575469406706372,22.4879715261163));
#8918=CARTESIAN_POINT('Ctrl Pts',(2.40107623921712,0.496388852392389,22.4837559248569));
#8919=CARTESIAN_POINT('Ctrl Pts',(2.41624634033402,0.416326366608874,22.4795403235974));
#8920=CARTESIAN_POINT('Ctrl Pts',(2.42739592099354,0.335707153251063,22.475324722338));
#8921=CARTESIAN_POINT('Ctrl Pts',(2.43854522344221,0.255089951550876,22.4711092262687));
#8922=CARTESIAN_POINT('Ctrl Pts',(2.4456741422628,0.173916510721103,22.4668937301994));
#8923=CARTESIAN_POINT('Ctrl Pts',(2.44874905604841,0.0926191691931757,22.4626782341301));
#8924=CARTESIAN_POINT('Ctrl Pts',(2.45185655264164,0.0104603740362012,22.4584180692645));
#8925=CARTESIAN_POINT('Ctrl Pts',(2.45082358306201,-0.0718244797263049,
22.454157904399));
#8926=CARTESIAN_POINT('Ctrl Pts',(2.44566947993346,-0.153788962289195,22.4498977395334));
#8927=CARTESIAN_POINT('Ctrl Pts',(2.44056199143983,-0.235012143342264,22.4456761043644));
#8928=CARTESIAN_POINT('Ctrl Pts',(2.43140772829698,-0.315920264567787,22.4414544691955));
#8929=CARTESIAN_POINT('Ctrl Pts',(2.41827755582982,-0.396085739417284,22.4372328340265));
#8930=CARTESIAN_POINT('Ctrl Pts',(2.40496763018356,-0.477348686443557,22.4329534043126));
#8931=CARTESIAN_POINT('Ctrl Pts',(2.38757221436306,-0.557848015856419,22.4286739745987));
#8932=CARTESIAN_POINT('Ctrl Pts',(2.36621781198578,-0.637152663214418,22.4243945448848));
#8933=CARTESIAN_POINT('Ctrl Pts',(2.34486340960851,-0.716457310572394,22.4201151151709));
#8934=CARTESIAN_POINT('Ctrl Pts',(2.31955023421842,-0.794566829373144,22.415835685457));
#8935=CARTESIAN_POINT('Ctrl Pts',(2.29045513733628,-0.871071474593132,22.4115562557431));
#8936=CARTESIAN_POINT('Ctrl Pts',(2.26169133209575,-0.94670499882634,22.4073255538029));
#8937=CARTESIAN_POINT('Ctrl Pts',(2.22912314501233,-1.02105450572569,22.4030948518626));
#8938=CARTESIAN_POINT('Ctrl Pts',(2.19288567228929,-1.09371050935262,22.3988641499224));
#8939=CARTESIAN_POINT('Ctrl Pts',(2.15670026284348,-1.16626212629428,22.3946395263367));
#8940=CARTESIAN_POINT('Ctrl Pts',(2.11685624355647,-1.23712465959164,22.390414902751));
#8941=CARTESIAN_POINT('Ctrl Pts',(2.07353737771202,-1.30590696193532,22.3861902791654));
#8942=CARTESIAN_POINT('Ctrl Pts',(2.03004801738204,-1.37495997781279,22.3819490282971));
#8943=CARTESIAN_POINT('Ctrl Pts',(1.98305656789864,-1.44191590929972,22.3777077774288));
#8944=CARTESIAN_POINT('Ctrl Pts',(1.93279642548731,-1.50640241224697,22.3734665265605));
#8945=CARTESIAN_POINT('Ctrl Pts',(1.8828236718605,-1.57052017971494,22.3692495272735));
#8946=CARTESIAN_POINT('Ctrl Pts',(1.82961979357148,-1.63219631202487,22.3650325279866));
#8947=CARTESIAN_POINT('Ctrl Pts',(1.77345747833994,-1.69109397211395,22.3608155286996));
#8948=CARTESIAN_POINT('Ctrl Pts',(1.7173137821445,-1.74997210634027,22.3565999274402));
#8949=CARTESIAN_POINT('Ctrl Pts',(1.6582139173668,-1.80607326123896,22.3523843261808));
#8950=CARTESIAN_POINT('Ctrl Pts',(1.59646922228821,-1.85909555222062,22.3481687249213));
#8951=CARTESIAN_POINT('Ctrl Pts',(1.53472606789922,-1.91211652015918,22.343953228852));
#8952=CARTESIAN_POINT('Ctrl Pts',(1.47033856795391,-1.96205847477121,22.3397377327827));
#8953=CARTESIAN_POINT('Ctrl Pts',(1.403652011213,-2.00865907545748,22.3355222367134));
#8954=CARTESIAN_POINT('Ctrl Pts',(1.33625882157064,-2.05575347158441,22.3312620718478));
#8955=CARTESIAN_POINT('Ctrl Pts',(1.26651794977151,-2.09943498925007,22.3270019069823));
#8956=CARTESIAN_POINT('Ctrl Pts',(1.19481520194442,-2.13947818011835,22.3227417421167));
#8957=CARTESIAN_POINT('Ctrl Pts',(1.12376094665424,-2.17915921317233,22.3185201069477));
#8958=CARTESIAN_POINT('Ctrl Pts',(1.05078060854926,-2.21526731287303,22.3142984717787));
#8959=CARTESIAN_POINT('Ctrl Pts',(0.976272051563283,-2.24763055935276,22.3100768366098));
#8960=CARTESIAN_POINT('Ctrl Pts',(0.900743466087549,-2.28043686143263,22.3057974068959));
#8961=CARTESIAN_POINT('Ctrl Pts',(0.823644965086106,-2.3093948252912,22.301517977182));
#8962=CARTESIAN_POINT('Ctrl Pts',(0.745407459788122,-2.33437742640136,22.2972385474681));
#8963=CARTESIAN_POINT('Ctrl Pts',(0.667169954490138,-2.35936002751151,22.2929591177542));
#8964=CARTESIAN_POINT('Ctrl Pts',(0.587793935911065,-2.38036720367027,22.2886796880403));
#8965=CARTESIAN_POINT('Ctrl Pts',(0.507719649770369,-2.3973258033144,22.2844002583264));
#8966=CARTESIAN_POINT('Ctrl Pts',(0.428557130372018,-2.41409130367664,22.2801695563861));
#8967=CARTESIAN_POINT('Ctrl Pts',(0.348414420808609,-2.42696305918838,22.2759388544458));
#8968=CARTESIAN_POINT('Ctrl Pts',(0.267708942148447,-2.43583295246077,22.2717081525056));
#8969=CARTESIAN_POINT('Ctrl Pts',(0.187119415054472,-2.44469010213714,22.2674835289199));
#8970=CARTESIAN_POINT('Ctrl Pts',(0.105969183031884,-2.44955675817102,22.2632589053342));
#8971=CARTESIAN_POINT('Ctrl Pts',(0.0246865977424086,-2.4503756491387,22.2590342817485));
#8972=CARTESIAN_POINT('Ctrl Pts',(-0.0569158997213511,-2.45119776309921,
22.2547930308803));
#8973=CARTESIAN_POINT('Ctrl Pts',(-0.138651330262343,-2.44794008292565,
22.250551780012));
#8974=CARTESIAN_POINT('Ctrl Pts',(-0.220080279254641,-2.44059724671712,
22.2463105291437));
#8975=CARTESIAN_POINT('Ctrl Pts',(-0.301043615426415,-2.43329639703451,
22.2420935298567));
#8976=CARTESIAN_POINT('Ctrl Pts',(-0.381703497640066,-2.42195702478502,
22.2378765305698));
#8977=CARTESIAN_POINT('Ctrl Pts',(-0.461629091239207,-2.40662602664429,
22.2336595312828));
#8978=CARTESIAN_POINT('Ctrl Pts',(-0.541528187755521,-2.39130011106484,
22.2294439300234));
#8979=CARTESIAN_POINT('Ctrl Pts',(-0.620693022701401,-2.37198528500518,
22.2252283287639));
#8980=CARTESIAN_POINT('Ctrl Pts',(-0.698701222103427,-2.34877986457462,
22.2210127275045));
#8981=CARTESIAN_POINT('Ctrl Pts',(-0.776707474999328,-2.32557502317926,
22.2167972314352));
#8982=CARTESIAN_POINT('Ctrl Pts',(-0.853556704287774,-2.29847991407358,
22.2125817353659));
#8983=CARTESIAN_POINT('Ctrl Pts',(-0.928841401710857,-2.26764280707254,
22.2083662392966));
#8984=CARTESIAN_POINT('Ctrl Pts',(-1.00492384078945,-2.23647893984489,22.2041060744311));
#8985=CARTESIAN_POINT('Ctrl Pts',(-1.07940793955795,-2.20149346835282,22.1998459095655));
#8986=CARTESIAN_POINT('Ctrl Pts',(-1.15189527062315,-2.16288870160164,22.1955857446999));
#8987=CARTESIAN_POINT('Ctrl Pts',(-1.22372701323972,-2.1246330832985,22.1913641095309));
#8988=CARTESIAN_POINT('Ctrl Pts',(-1.29359758931343,-2.08282366793479,22.187142474362));
#8989=CARTESIAN_POINT('Ctrl Pts',(-1.36114704767515,-2.03770188315298,22.182920839193));
#8990=CARTESIAN_POINT('Ctrl Pts',(-1.42962126387374,-1.99196237729536,22.1786414094791));
#8991=CARTESIAN_POINT('Ctrl Pts',(-1.49570993162519,-1.94281941724681,22.1743619797652));
#8992=CARTESIAN_POINT('Ctrl Pts',(-1.55907295365847,-1.89056652228126,22.1700825500513));
#8993=CARTESIAN_POINT('Ctrl Pts',(-1.62243597569174,-1.83831362731572,22.1658031203375));
#8994=CARTESIAN_POINT('Ctrl Pts',(-1.68307303386764,-1.78295117658067,22.1615236906235));
#8995=CARTESIAN_POINT('Ctrl Pts',(-1.74068427121121,-1.72480970485381,22.1572442609096));
#8996=CARTESIAN_POINT('Ctrl Pts',(-1.7968404183609,-1.66813671547985,22.1530729169877));
#8997=CARTESIAN_POINT('Ctrl Pts',(-1.85034552545501,-1.60859737264155,22.1489015730657));
#8998=CARTESIAN_POINT('Ctrl Pts',(-1.90088679305711,-1.54647329429935,22.1447302291437));
#8999=CARTESIAN_POINT('Ctrl Pts',(-1.95136270988548,-1.48442954351477,22.1405642788449));
#9000=CARTESIAN_POINT('Ctrl Pts',(-1.9988820873696,-1.41980805190629,22.1363983285462));
#9001=CARTESIAN_POINT('Ctrl Pts',(-2.04316834329864,-1.35292770351644,22.1322323782474));
#9002=CARTESIAN_POINT('Ctrl Pts',(-2.08741180346071,-1.286111984564,22.1280704536905));
#9003=CARTESIAN_POINT('Ctrl Pts',(-2.12842807668247,-1.21704213571679,22.1239085291337));
#9004=CARTESIAN_POINT('Ctrl Pts',(-2.16598137453372,-1.14606934134589,22.1197466045769));
#9005=CARTESIAN_POINT('Ctrl Pts',(-2.20351064303067,-1.07514196057431,22.1155873431246));
#9006=CARTESIAN_POINT('Ctrl Pts',(-2.23758111056645,-1.00231447313506,22.1114280816724));
#9007=CARTESIAN_POINT('Ctrl Pts',(-2.26800165933677,-0.927964828668443,
22.1072688202201));
#9008=CARTESIAN_POINT('Ctrl Pts',(-2.29842423865581,-0.853610221419062,
22.1031092811403));
#9009=CARTESIAN_POINT('Ctrl Pts',(-2.32519621322486,-0.777733690127223,
22.0989497420605));
#9010=CARTESIAN_POINT('Ctrl Pts',(-2.34817408744077,-0.700734404087374,
22.0947902029807));
#9011=CARTESIAN_POINT('Ctrl Pts',(-2.37115120639363,-0.62373764894816,22.0906308006213));
#9012=CARTESIAN_POINT('Ctrl Pts',(-2.39033434371215,-0.545618674233663,
22.086471398262));
#9013=CARTESIAN_POINT('Ctrl Pts',(-2.40563014694972,-0.466791009003669,
22.0823119959027));
#9014=CARTESIAN_POINT('Ctrl Pts',(-2.42094168019324,-0.387882278423694,
22.0781483160678));
#9015=CARTESIAN_POINT('Ctrl Pts',(-2.43235781015019,-0.308263874393964,
22.073984636233));
#9016=CARTESIAN_POINT('Ctrl Pts',(-2.43983664962305,-0.228357993414225,
22.0698209563982));
#9017=CARTESIAN_POINT('Ctrl Pts',(-2.44701757026806,-0.151635155269717,
22.0658231363361));
#9018=CARTESIAN_POINT('Ctrl Pts',(-2.45056895731558,-0.0746477053578802,
22.0618253162741));
#9019=CARTESIAN_POINT('Ctrl Pts',(-2.45049898498603,0.00223037720034039,
22.0578274962121));
#9020=CARTESIAN_POINT('',(-2.45061844109802,-0.00106435975836244,21.2578274962121));
#9021=CARTESIAN_POINT('Ctrl Pts',(-2.45086617389337,0.00223071140564801,
22.0578274962121));
#9022=CARTESIAN_POINT('Ctrl Pts',(-2.45251442784572,0.180067490317817,22.0485810853057));
#9023=CARTESIAN_POINT('Ctrl Pts',(-2.35363098083641,1.17128616743177,21.996949341927));
#9024=CARTESIAN_POINT('Ctrl Pts',(-1.00509393446104,2.71753790621056,21.9029322660762));
#9025=CARTESIAN_POINT('Ctrl Pts',(1.7406206758319,2.31634750235136,21.7757762686594));
#9026=CARTESIAN_POINT('Ctrl Pts',(2.88987924261423,-0.209341949658435,21.6486202712428));
#9027=CARTESIAN_POINT('Ctrl Pts',(1.38860903771261,-2.54302792536034,21.5214642738259));
#9028=CARTESIAN_POINT('Ctrl Pts',(-1.38626047639343,-2.54430893964709,21.3943082764093));
#9029=CARTESIAN_POINT('Ctrl Pts',(-2.42529371805448,-0.93243122202057,21.306429350538));
#9030=CARTESIAN_POINT('Ctrl Pts',(-2.45429856883823,-0.060650494243286,
21.2609357571389));
#9031=CARTESIAN_POINT('Ctrl Pts',(-2.45397390661175,-0.00106581711394382,
21.2578274962121));
#9032=CARTESIAN_POINT('',(-2.45049945194367,-0.00163890932682275,20.457827496242));
#9033=CARTESIAN_POINT('Ctrl Pts',(-2.45049976887328,-0.00106430821629522,
21.2578274962121));
#9034=CARTESIAN_POINT('Ctrl Pts',(-2.45053457116059,0.0790656726311988,
21.2536415436539));
#9035=CARTESIAN_POINT('Ctrl Pts',(-2.44663482555755,0.159355808442185,21.2494555910958));
#9036=CARTESIAN_POINT('Ctrl Pts',(-2.43877965671865,0.239382614187571,21.2452696385376));
#9037=CARTESIAN_POINT('Ctrl Pts',(-2.43054835629895,0.323241369260646,21.2408832486642));
#9038=CARTESIAN_POINT('Ctrl Pts',(-2.41797325303175,0.406810428677306,21.2364968587908));
#9039=CARTESIAN_POINT('Ctrl Pts',(-2.40109181530039,0.48960018841653,21.2321104689173));
#9040=CARTESIAN_POINT('Ctrl Pts',(-2.38502088583582,0.56841506250072,21.2279346775315));
#9041=CARTESIAN_POINT('Ctrl Pts',(-2.36504768720049,0.646523207223542,21.2237588861456));
#9042=CARTESIAN_POINT('Ctrl Pts',(-2.3412575617958,0.723507622167163,21.2195830947598));
#9043=CARTESIAN_POINT('Ctrl Pts',(-2.31747992244979,0.80045163245106,21.2154094950049));
#9044=CARTESIAN_POINT('Ctrl Pts',(-2.28988947121437,0.876272629653963,21.21123589525));
#9045=CARTESIAN_POINT('Ctrl Pts',(-2.25862197796156,0.950566678707497,21.2070622954951));
#9046=CARTESIAN_POINT('Ctrl Pts',(-2.22736082903793,1.02484565313069,21.2028895425843));
#9047=CARTESIAN_POINT('Ctrl Pts',(-2.1924243042169,1.09759785649143,21.1987167896735));
#9048=CARTESIAN_POINT('Ctrl Pts',(-2.15399652100067,1.1684388034968,21.1945440367627));
#9049=CARTESIAN_POINT('Ctrl Pts',(-2.11556416357238,1.23928818298218,21.1903707871525));
#9050=CARTESIAN_POINT('Ctrl Pts',(-2.07363995182196,1.30822543773707,21.1861975375423));
#9051=CARTESIAN_POINT('Ctrl Pts',(-2.02845344465825,1.37489158585471,21.1820242879321));
#9052=CARTESIAN_POINT('Ctrl Pts',(-1.98321910359144,1.44162830596983,21.1778466205691));
#9053=CARTESIAN_POINT('Ctrl Pts',(-1.93471584461374,1.50608872883422,21.1736689532061));
#9054=CARTESIAN_POINT('Ctrl Pts',(-1.88321550237887,1.56794439365683,21.1694912858431));
#9055=CARTESIAN_POINT('Ctrl Pts',(-1.8316833021961,1.62983832219696,21.1653110341884));
#9056=CARTESIAN_POINT('Ctrl Pts',(-1.77715065342666,1.68912393887092,21.1611307825337));
#9057=CARTESIAN_POINT('Ctrl Pts',(-1.71992671606892,1.74550919257172,21.1569505308789));
#9058=CARTESIAN_POINT('Ctrl Pts',(-1.66261026310704,1.8019856059524,21.1527635208898));
#9059=CARTESIAN_POINT('Ctrl Pts',(-1.60259419652624,1.85555198760815,21.1485765109006));
#9060=CARTESIAN_POINT('Ctrl Pts',(-1.5402206393873,1.90595661860531,21.1443895009114));
#9061=CARTESIAN_POINT('Ctrl Pts',(-1.51840549222494,1.92358563470292,21.1429250944662));
#9062=CARTESIAN_POINT('Ctrl Pts',(-1.49630221864538,1.94082828205214,21.141460688021));
#9063=CARTESIAN_POINT('Ctrl Pts',(-1.47392622329026,1.95767508496617,21.1399962815758));
#9064=CARTESIAN_POINT('Ctrl Pts',(-1.40928148802951,2.00634586349842,21.1357655796355));
#9065=CARTESIAN_POINT('Ctrl Pts',(-1.34210184128882,2.05190276253568,21.1315348776953));
#9066=CARTESIAN_POINT('Ctrl Pts',(-1.27271981542071,2.09407127897678,21.127304175755));
#9067=CARTESIAN_POINT('Ctrl Pts',(-1.20343747243289,2.13617921086268,21.1230795521694));
#9068=CARTESIAN_POINT('Ctrl Pts',(-1.13195942866314,2.17490818912302,21.1188549285837));
#9069=CARTESIAN_POINT('Ctrl Pts',(-1.05864962455588,2.21002516330192,21.114630304998));
#9070=CARTESIAN_POINT('Ctrl Pts',(-0.985051287563485,2.24528035094355,21.1103890541297));
#9071=CARTESIAN_POINT('Ctrl Pts',(-0.909607119530442,2.27689475581923,21.1061478032615));
#9072=CARTESIAN_POINT('Ctrl Pts',(-0.832713038729248,2.30467768790569,21.1019065523932));
#9073=CARTESIAN_POINT('Ctrl Pts',(-0.756258640255835,2.33230175647332,21.0976895531062));
#9074=CARTESIAN_POINT('Ctrl Pts',(-0.678371307079352,2.35613789064809,21.0934725538192));
#9075=CARTESIAN_POINT('Ctrl Pts',(-0.599461283012908,2.37604638426284,21.0892555545323));
#9076=CARTESIAN_POINT('Ctrl Pts',(-0.520577419345773,2.39594827777642,21.0850399532728));
#9077=CARTESIAN_POINT('Ctrl Pts',(-0.440671988646477,2.41192500280039,21.0808243520134));
#9078=CARTESIAN_POINT('Ctrl Pts',(-0.360169313484261,2.42388702616774,21.076608750754));
#9079=CARTESIAN_POINT('Ctrl Pts',(-0.279668647071809,2.43584875105169,21.0723932546847));
#9080=CARTESIAN_POINT('Ctrl Pts',(-0.198571225996181,2.44379590617561,21.0681777586154));
#9081=CARTESIAN_POINT('Ctrl Pts',(-0.117309027646915,2.4476905118974,21.0639622625461));
#9082=CARTESIAN_POINT('Ctrl Pts',(-0.0351857480572538,2.45162638615479,
21.0597020976805));
#9083=CARTESIAN_POINT('Ctrl Pts',(0.0471053385266302,2.45142327603031,21.0554419328149));
#9084=CARTESIAN_POINT('Ctrl Pts',(0.129117630039666,2.44709601111459,21.0511817679493));
#9085=CARTESIAN_POINT('Ctrl Pts',(0.210388187650214,2.4428078827604,21.0469601327804));
#9086=CARTESIAN_POINT('Ctrl Pts',(0.291384511414774,2.43447000829635,21.0427384976114));
#9087=CARTESIAN_POINT('Ctrl Pts',(0.371678321881904,2.42214893741963,21.0385168624424));
#9088=CARTESIAN_POINT('Ctrl Pts',(0.453071361451193,2.40965919003349,21.0342374327285));
#9089=CARTESIAN_POINT('Ctrl Pts',(0.533742022627232,2.39307645947121,21.0299580030146));
#9090=CARTESIAN_POINT('Ctrl Pts',(0.613257987154518,2.37252289582023,21.0256785733008));
#9091=CARTESIAN_POINT('Ctrl Pts',(0.692773951681803,2.35196933216924,21.0213991435869));
#9092=CARTESIAN_POINT('Ctrl Pts',(0.771134770927176,2.32744514445989,21.017119713873));
#9093=CARTESIAN_POINT('Ctrl Pts',(0.847928937232249,2.29912304311974,21.0128402841591));
#9094=CARTESIAN_POINT('Ctrl Pts',(0.923848685915814,2.27112343169884,21.0086095822188));
#9095=CARTESIAN_POINT('Ctrl Pts',(0.998522848093135,2.23930668313396,21.0043788802785));
#9096=CARTESIAN_POINT('Ctrl Pts',(1.0715405962618,2.20380375727126,21.0001481783383));
#9097=CARTESIAN_POINT('Ctrl Pts',(1.14445343801784,2.16835183934407,20.9959235547526));
#9098=CARTESIAN_POINT('Ctrl Pts',(1.21571417750784,2.12922446394462,20.9916989311669));
#9099=CARTESIAN_POINT('Ctrl Pts',(1.28492983413974,2.08660144046188,20.9874743075812));
#9100=CARTESIAN_POINT('Ctrl Pts',(1.35441790990188,2.04381066119166,20.9832330567129));
#9101=CARTESIAN_POINT('Ctrl Pts',(1.4218443249558,1.99749682266795,20.9789918058446));
#9102=CARTESIAN_POINT('Ctrl Pts',(1.48683440038694,1.94788955431924,20.9747505549763));
#9103=CARTESIAN_POINT('Ctrl Pts',(1.55145286089868,1.8985659416042,20.9705335556894));
#9104=CARTESIAN_POINT('Ctrl Pts',(1.61366239489633,1.84598674570367,20.9663165564024));
#9105=CARTESIAN_POINT('Ctrl Pts',(1.6731234325085,1.79042124361586,20.9620995571155));
#9106=CARTESIAN_POINT('Ctrl Pts',(1.73256475748587,1.73487416270761,20.957883955856));
#9107=CARTESIAN_POINT('Ctrl Pts',(1.78925905601964,1.67634305891218,20.9536683545966));
#9108=CARTESIAN_POINT('Ctrl Pts',(1.84290131916034,1.61513621030459,20.9494527533371));
#9109=CARTESIAN_POINT('Ctrl Pts',(1.89654224378802,1.55393088896597,20.9452372572678));
#9110=CARTESIAN_POINT('Ctrl Pts',(1.94713097873232,1.49005030602837,20.9410217611985));
#9111=CARTESIAN_POINT('Ctrl Pts',(1.99440171464731,1.42383708710367,20.9368062651292));
#9112=CARTESIAN_POINT('Ctrl Pts',(2.04217334697813,1.35692225092259,20.9325461002637));
#9113=CARTESIAN_POINT('Ctrl Pts',(2.08655594974683,1.28762543457208,20.9282859353981));
#9114=CARTESIAN_POINT('Ctrl Pts',(2.12732019539462,1.21633015101419,20.9240257705325));
#9115=CARTESIAN_POINT('Ctrl Pts',(2.16771576187937,1.14567967481268,20.9198041353635));
#9116=CARTESIAN_POINT('Ctrl Pts',(2.20455800040299,1.07306718226124,20.9155825001946));
#9117=CARTESIAN_POINT('Ctrl Pts',(2.23767098755545,0.998888783325058,20.9113608650256));
#9118=CARTESIAN_POINT('Ctrl Pts',(2.27123729432136,0.923694875791697,20.9070814353117));
#9119=CARTESIAN_POINT('Ctrl Pts',(2.30097129047062,0.846892323748042,20.9028020055978));
#9120=CARTESIAN_POINT('Ctrl Pts',(2.32674161238323,0.768910735524134,20.898522575884));
#9121=CARTESIAN_POINT('Ctrl Pts',(2.35251193429585,0.690929147300226,20.8942431461701));
#9122=CARTESIAN_POINT('Ctrl Pts',(2.37431851482032,0.611769013259261,20.8899637164562));
#9123=CARTESIAN_POINT('Ctrl Pts',(2.39208376642678,0.531869819032303,20.8856842867423));
#9124=CARTESIAN_POINT('Ctrl Pts',(2.40964673379992,0.452880397861552,20.8814535848021));
#9125=CARTESIAN_POINT('Ctrl Pts',(2.42332603911261,0.37287156964722,20.8772228828618));
#9126=CARTESIAN_POINT('Ctrl Pts',(2.43300936096408,0.292259643914732,20.8729921809216));
#9127=CARTESIAN_POINT('Ctrl Pts',(2.44267877054647,0.211763535338661,20.8687675573359));
#9128=CARTESIAN_POINT('Ctrl Pts',(2.44836354387018,0.130666507954962,20.8645429337503));
#9129=CARTESIAN_POINT('Ctrl Pts',(2.45000209268374,0.0493963140860758,20.8603183101646));
#9130=CARTESIAN_POINT('Ctrl Pts',(2.45164709050126,-0.0321937431872997,
20.8560770592963));
#9131=CARTESIAN_POINT('Ctrl Pts',(2.44921384221654,-0.113957869725936,20.851835808428));
#9132=CARTESIAN_POINT('Ctrl Pts',(2.44269255489614,-0.19545672732079,20.8475945575597));
#9133=CARTESIAN_POINT('Ctrl Pts',(2.43620855646406,-0.276489572355669,20.8433775582728));
#9134=CARTESIAN_POINT('Ctrl Pts',(2.425683180625,-0.357259705605165,20.8391605589858));
#9135=CARTESIAN_POINT('Ctrl Pts',(2.41115897688995,-0.437335841388503,20.8349435596989));
#9136=CARTESIAN_POINT('Ctrl Pts',(2.39663958824617,-0.517385430181111,20.8307279584394));
#9137=CARTESIAN_POINT('Ctrl Pts',(2.37812408725206,-0.596741021166517,20.82651235718));
#9138=CARTESIAN_POINT('Ctrl Pts',(2.35570652555985,-0.67497927037408,20.8222967559206));
#9139=CARTESIAN_POINT('Ctrl Pts',(2.33328952324378,-0.753215567335034,20.8180812598513));
#9140=CARTESIAN_POINT('Ctrl Pts',(2.30697078296014,-0.83033413118005,20.813865763782));
#9141=CARTESIAN_POINT('Ctrl Pts',(2.27689445744093,-0.905925979136689,20.8096502677127));
#9142=CARTESIAN_POINT('Ctrl Pts',(2.24649943318818,-0.982318823418311,20.8053901028471));
#9143=CARTESIAN_POINT('Ctrl Pts',(2.21226688043535,-1.05715194788155,20.8011299379815));
#9144=CARTESIAN_POINT('Ctrl Pts',(2.17439507993339,-1.13002490519522,20.7968697731159));
#9145=CARTESIAN_POINT('Ctrl Pts',(2.13686579880114,-1.2022387863869,20.792648137947));
#9146=CARTESIAN_POINT('Ctrl Pts',(2.09576312380993,-1.2725274392583,20.788426502778));
#9147=CARTESIAN_POINT('Ctrl Pts',(2.05132484037468,-1.34052849625131,20.7842048676091));
#9148=CARTESIAN_POINT('Ctrl Pts',(2.00627819305501,-1.40946049350526,20.7799254378951));
#9149=CARTESIAN_POINT('Ctrl Pts',(1.95780420739424,-1.47604138597227,20.7756460081812));
#9150=CARTESIAN_POINT('Ctrl Pts',(1.90619295800774,-1.53992813366134,20.7713665784673));
#9151=CARTESIAN_POINT('Ctrl Pts',(1.85458170862125,-1.6038148813504,20.7670871487534));
#9152=CARTESIAN_POINT('Ctrl Pts',(1.79983357142897,-1.66500716231496,20.7628077190395));
#9153=CARTESIAN_POINT('Ctrl Pts',(1.74227604047368,-1.72320180152858,20.7585282893256));
#9154=CARTESIAN_POINT('Ctrl Pts',(1.6853738889797,-1.78073380684068,20.7542975873853));
#9155=CARTESIAN_POINT('Ctrl Pts',(1.62551200269765,-1.83555251310833,20.7500668854451));
#9156=CARTESIAN_POINT('Ctrl Pts',(1.56297958485594,-1.88733809035995,20.7458361835048));
#9157=CARTESIAN_POINT('Ctrl Pts',(1.50053700889227,-1.93904926598637,20.7416115599191));
#9158=CARTESIAN_POINT('Ctrl Pts',(1.43543187664608,-1.98773567326295,20.7373869363334));
#9159=CARTESIAN_POINT('Ctrl Pts',(1.36799047949149,-2.03311394122923,20.7331623127477));
#9160=CARTESIAN_POINT('Ctrl Pts',(1.30028364634082,-2.07867080908024,20.7289210618795));
#9161=CARTESIAN_POINT('Ctrl Pts',(1.23022245239336,-2.12089310400238,20.7246798110112));
#9162=CARTESIAN_POINT('Ctrl Pts',(1.15817097254333,-2.1595347296022,20.7204385601429));
#9163=CARTESIAN_POINT('Ctrl Pts',(1.08653148490456,-2.19795540139495,20.7162215608559));
#9164=CARTESIAN_POINT('Ctrl Pts',(1.01292482457161,-2.23283601945659,20.712004561569));
#9165=CARTESIAN_POINT('Ctrl Pts',(0.937736635034463,-2.26397885443178,20.707787562282));
#9166=CARTESIAN_POINT('Ctrl Pts',(0.862573372027066,-2.29511136487586,20.7035719610226));
#9167=CARTESIAN_POINT('Ctrl Pts',(0.785830050330809,-2.32250837516431,20.6993563597631));
#9168=CARTESIAN_POINT('Ctrl Pts',(0.707913520252535,-2.34601975649048,20.6951407585037));
#9169=CARTESIAN_POINT('Ctrl Pts',(0.629998934392989,-2.36953055114694,20.6909252624344));
#9170=CARTESIAN_POINT('Ctrl Pts',(0.550911643902007,-2.38915577630415,20.6867097663651));
#9171=CARTESIAN_POINT('Ctrl Pts',(0.471073550119092,-2.40479520133798,20.6824942702958));
#9172=CARTESIAN_POINT('Ctrl Pts',(0.390389465380692,-2.42060034691324,20.6782341054303));
#9173=CARTESIAN_POINT('Ctrl Pts',(0.30893904342235,-2.43233461074544,20.6739739405647));
#9174=CARTESIAN_POINT('Ctrl Pts',(0.227166314897859,-2.43994789193862,20.6697137756991));
#9175=CARTESIAN_POINT('Ctrl Pts',(0.146133153625253,-2.44749231724854,20.6654921405301));
#9176=CARTESIAN_POINT('Ctrl Pts',(0.0647839647791666,-2.45099004336908,
20.6612705053612));
#9177=CARTESIAN_POINT('Ctrl Pts',(-0.0164478485492509,-2.45044480008796,
20.6570488701922));
#9178=CARTESIAN_POINT('Ctrl Pts',(-0.0987917323190438,-2.44989209237989,
20.6527694404783));
#9179=CARTESIAN_POINT('Ctrl Pts',(-0.181014508631477,-2.44518490819373,
20.6484900107644));
#9180=CARTESIAN_POINT('Ctrl Pts',(-0.262670714200303,-2.43638140402965,
20.6442105810505));
#9181=CARTESIAN_POINT('Ctrl Pts',(-0.34432691976913,-2.42757789986558,20.6399311513366));
#9182=CARTESIAN_POINT('Ctrl Pts',(-0.425416080387844,-2.41467821747542,
20.6356517216227));
#9183=CARTESIAN_POINT('Ctrl Pts',(-0.505505990217785,-2.39779355738853,
20.6313722919088));
#9184=CARTESIAN_POINT('Ctrl Pts',(-0.584683955406296,-2.38110115466991,
20.6271415899686));
#9185=CARTESIAN_POINT('Ctrl Pts',(-0.663183129487585,-2.3604513204164,20.6229108880283));
#9186=CARTESIAN_POINT('Ctrl Pts',(-0.740578034953068,-2.33591404468252,
20.618680186088));
#9187=CARTESIAN_POINT('Ctrl Pts',(-0.817861745235176,-2.31141202226226,
20.6144555625024));
#9188=CARTESIAN_POINT('Ctrl Pts',(-0.894043898284959,-2.28303379019962,
20.6102309389167));
#9189=CARTESIAN_POINT('Ctrl Pts',(-0.968709589820252,-2.25090026002715,
20.606006315331));
#9190=CARTESIAN_POINT('Ctrl Pts',(-1.04366915074491,-2.2186402586375,20.6017650644627));
#9191=CARTESIAN_POINT('Ctrl Pts',(-1.11709982321976,-2.18259543340949,20.5975238135944));
#9192=CARTESIAN_POINT('Ctrl Pts',(-1.18859758538988,-2.1429386435466,20.5932825627261));
#9193=CARTESIAN_POINT('Ctrl Pts',(-1.25968652152083,-2.10350861222599,20.5890655634391));
#9194=CARTESIAN_POINT('Ctrl Pts',(-1.32886418144608,-2.06050803863655,20.5848485641522));
#9195=CARTESIAN_POINT('Ctrl Pts',(-1.39575553076863,-2.01415410242831,20.5806315648652));
#9196=CARTESIAN_POINT('Ctrl Pts',(-1.46262470414545,-1.96781553356404,20.5764159636058));
#9197=CARTESIAN_POINT('Ctrl Pts',(-1.52720869015642,-1.91812607443359,20.5722003623463));
#9198=CARTESIAN_POINT('Ctrl Pts',(-1.58916099330204,-1.86534650597879,20.5679847610869));
#9199=CARTESIAN_POINT('Ctrl Pts',(-1.65111175057791,-1.81256825451034,20.5637692650176));
#9200=CARTESIAN_POINT('Ctrl Pts',(-1.71043060224588,-1.75670034944357,20.5595537689482));
#9201=CARTESIAN_POINT('Ctrl Pts',(-1.76680485627142,-1.69804324145639,20.5553382728789));
#9202=CARTESIAN_POINT('Ctrl Pts',(-1.82377647061365,-1.63876458327385,20.5510781080133));
#9203=CARTESIAN_POINT('Ctrl Pts',(-1.87774036455432,-1.57663759770729,20.5468179431478));
#9204=CARTESIAN_POINT('Ctrl Pts',(-1.92841401193213,-1.51200848165075,20.5425577782822));
#9205=CARTESIAN_POINT('Ctrl Pts',(-1.97862935773705,-1.44796388293363,20.5383361431132));
#9206=CARTESIAN_POINT('Ctrl Pts',(-2.02561351182713,-1.38146265077644,20.5341145079442));
#9207=CARTESIAN_POINT('Ctrl Pts',(-2.06913496048165,-1.31287119143982,20.5298928727753));
#9208=CARTESIAN_POINT('Ctrl Pts',(-2.11325222147361,-1.24334070918508,20.5256134430614));
#9209=CARTESIAN_POINT('Ctrl Pts',(-2.15381100610034,-1.17166276615519,20.5213340133475));
#9210=CARTESIAN_POINT('Ctrl Pts',(-2.19061903077653,-1.09824337557742,20.5170545836337));
#9211=CARTESIAN_POINT('Ctrl Pts',(-2.22742705545273,-1.02482398499965,20.5127751539198));
#9212=CARTESIAN_POINT('Ctrl Pts',(-2.26048418261629,-0.949663622312802,
20.5084957242059));
#9213=CARTESIAN_POINT('Ctrl Pts',(-2.28964990358769,-0.873185873111157,
20.5042162944921));
#9214=CARTESIAN_POINT('Ctrl Pts',(-2.32256423751074,-0.786878588700953,
20.4993868380648));
#9215=CARTESIAN_POINT('Ctrl Pts',(-2.35062682283035,-0.698624244658884,
20.4945573816374));
#9216=CARTESIAN_POINT('Ctrl Pts',(-2.37363404666454,-0.608943070011404,
20.4897279252101));
#9217=CARTESIAN_POINT('Ctrl Pts',(-2.3965458373727,-0.519633889608201,20.4849185011921));
#9218=CARTESIAN_POINT('Ctrl Pts',(-2.4144439916773,-0.428909874618249,20.480109077174));
#9219=CARTESIAN_POINT('Ctrl Pts',(-2.42717418291953,-0.337306590165269,
20.475299653156));
#9220=CARTESIAN_POINT('Ctrl Pts',(-2.43981461087043,-0.246349219992158,
20.4705241414116));
#9221=CARTESIAN_POINT('Ctrl Pts',(-2.44735958946865,-0.154525137022721,
20.4657486296672));
#9222=CARTESIAN_POINT('Ctrl Pts',(-2.44970596636031,-0.0623773066003385,
20.4609731179229));
#9223=CARTESIAN_POINT('Ctrl Pts',(-2.45022115121845,-0.0421447654798911,
20.4599245773626));
#9224=CARTESIAN_POINT('Ctrl Pts',(-2.450485903419,-0.0218966818199169,20.4588760368023));
#9225=CARTESIAN_POINT('Ctrl Pts',(-2.45049945194367,-0.00163890932682414,
20.457827496242));
#9226=CARTESIAN_POINT('',(-2.45049932159731,0.0018234174231849,19.6578274961832));
#9227=CARTESIAN_POINT('Ctrl Pts',(-2.45049945194405,-0.0016389087485609,
20.4578274962121));
#9228=CARTESIAN_POINT('Ctrl Pts',(-2.45055421052199,0.0802362202531978,
20.4535896465835));
#9229=CARTESIAN_POINT('Ctrl Pts',(-2.44650126866439,0.16213599296622,20.4493517969549));
#9230=CARTESIAN_POINT('Ctrl Pts',(-2.43835979033716,0.243622213410317,20.4451139473264));
#9231=CARTESIAN_POINT('Ctrl Pts',(-2.43021791027475,0.325112454731139,20.4408758885843));
#9232=CARTESIAN_POINT('Ctrl Pts',(-2.41798713907075,0.406188647605483,20.4366378298422));
#9233=CARTESIAN_POINT('Ctrl Pts',(-2.40173848544128,0.486418027575255,20.4323997711001));
#9234=CARTESIAN_POINT('Ctrl Pts',(-2.38548424781655,0.566674979089633,20.4281602559111));
#9235=CARTESIAN_POINT('Ctrl Pts',(-2.36520947641849,0.646084091095377,20.4239207407222));
#9236=CARTESIAN_POINT('Ctrl Pts',(-2.34103593495705,0.724224413589979,20.4196812255333));
#9237=CARTESIAN_POINT('Ctrl Pts',(-2.31683056137721,0.802467632551038,20.4154361276808));
#9238=CARTESIAN_POINT('Ctrl Pts',(-2.28871630842795,0.87943828998129,20.4111910298283));
#9239=CARTESIAN_POINT('Ctrl Pts',(-2.25686416502691,0.9547326278165,20.4069459319758));
#9240=CARTESIAN_POINT('Ctrl Pts',(-2.22498765302891,1.03008456985588,20.4026975863959));
#9241=CARTESIAN_POINT('Ctrl Pts',(-2.18936775799366,1.10375722819108,20.398449240816));
#9242=CARTESIAN_POINT('Ctrl Pts',(-2.15022167574432,1.17537100319827,20.3942008952361));
#9243=CARTESIAN_POINT('Ctrl Pts',(-2.11100646739711,1.24711123736905,20.3899450477165));
#9244=CARTESIAN_POINT('Ctrl Pts',(-2.06825288420797,1.31678494324426,20.3856892001968));
#9245=CARTESIAN_POINT('Ctrl Pts',(-2.02222143977409,1.38404143670557,20.3814333526771));
#9246=CARTESIAN_POINT('Ctrl Pts',(-2.00645504894317,1.4070776932226,20.3799756674765));
#9247=CARTESIAN_POINT('Ctrl Pts',(-1.99030445808792,1.42983066454623,20.3785179822759));
#9248=CARTESIAN_POINT('Ctrl Pts',(-1.9737811738493,1.45228720567182,20.3770602970754));
#9249=CARTESIAN_POINT('Ctrl Pts',(-1.92582494114561,1.51746378294222,20.3728295951351));
#9250=CARTESIAN_POINT('Ctrl Pts',(-1.8745467411694,1.58038502095646,20.3685988931949));
#9251=CARTESIAN_POINT('Ctrl Pts',(-1.82018633211609,1.6406925264588,20.3643681912547));
#9252=CARTESIAN_POINT('Ctrl Pts',(-1.7659040240129,1.70091338666983,20.360143567669));
#9253=CARTESIAN_POINT('Ctrl Pts',(-1.70854861038468,1.75852762992404,20.3559189440833));
#9254=CARTESIAN_POINT('Ctrl Pts',(-1.64840183330696,1.81320755732769,20.3516943204977));
#9255=CARTESIAN_POINT('Ctrl Pts',(-1.58801833041419,1.86810269410764,20.3474530696294));
#9256=CARTESIAN_POINT('Ctrl Pts',(-1.52482172567997,1.92003998548779,20.3432118187611));
#9257=CARTESIAN_POINT('Ctrl Pts',(-1.45913655136706,1.96872313301404,20.3389705678928));
#9258=CARTESIAN_POINT('Ctrl Pts',(-1.39382696656726,2.01712790905287,20.3347535686059));
#9259=CARTESIAN_POINT('Ctrl Pts',(-1.3260575717552,2.06231537510799,20.3305365693189));
#9260=CARTESIAN_POINT('Ctrl Pts',(-1.25618125472393,2.10403396010621,20.326319570032));
#9261=CARTESIAN_POINT('Ctrl Pts',(-1.18632810322037,2.14573871448086,20.3221039687726));
#9262=CARTESIAN_POINT('Ctrl Pts',(-1.11436981557281,2.1839766333117,20.3178883675131));
#9263=CARTESIAN_POINT('Ctrl Pts',(-1.04068716598189,2.21854016699283,20.3136727662537));
#9264=CARTESIAN_POINT('Ctrl Pts',(-0.967006354963416,2.25310283822452,20.3094572701844));
#9265=CARTESIAN_POINT('Ctrl Pts',(-0.891601689049961,2.28399111007847,20.3052417741152));
#9266=CARTESIAN_POINT('Ctrl Pts',(-0.814876071396342,2.31104462057003,20.3010262780459));
#9267=CARTESIAN_POINT('Ctrl Pts',(-0.737337443617486,2.33838479904322,20.2967661131803));
#9268=CARTESIAN_POINT('Ctrl Pts',(-0.658450154465879,2.36180828715304,20.2925059483147));
#9269=CARTESIAN_POINT('Ctrl Pts',(-0.578646273070949,2.38120111302282,20.2882457834491));
#9270=CARTESIAN_POINT('Ctrl Pts',(-0.499564152321246,2.40041854669026,20.2840241482801));
#9271=CARTESIAN_POINT('Ctrl Pts',(-0.41958242575381,2.41567790543055,20.2798025131112));
#9272=CARTESIAN_POINT('Ctrl Pts',(-0.339130454732167,2.42692002024648,20.2755808779422));
#9273=CARTESIAN_POINT('Ctrl Pts',(-0.257577089375796,2.43831604057163,20.2713014482283));
#9274=CARTESIAN_POINT('Ctrl Pts',(-0.175540999427799,2.44558394767251,20.2670220185144));
#9275=CARTESIAN_POINT('Ctrl Pts',(-0.0934713727955725,2.44871667460074,
20.2627425888004));
#9276=CARTESIAN_POINT('Ctrl Pts',(-0.0114017461633575,2.45184940152897,
20.2584631590865));
#9277=CARTESIAN_POINT('Ctrl Pts',(0.0707009274014986,2.4508470197602,20.2541837293726));
#9278=CARTESIAN_POINT('Ctrl Pts',(0.152392883928499,2.44575686831867,20.2499042996586));
#9279=CARTESIAN_POINT('Ctrl Pts',(0.233154654090854,2.44072467594271,20.2456735977184));
#9280=CARTESIAN_POINT('Ctrl Pts',(0.313818783241487,2.43167844720005,20.2414428957781));
#9281=CARTESIAN_POINT('Ctrl Pts',(0.393954141627136,2.41862572224287,20.2372121938379));
#9282=CARTESIAN_POINT('Ctrl Pts',(0.473974367552768,2.40559175045987,20.2329875702522));
#9283=CARTESIAN_POINT('Ctrl Pts',(0.55346687639895,2.38856278878805,20.2287629466665));
#9284=CARTESIAN_POINT('Ctrl Pts',(0.632003614358155,2.3675982939338,20.2245383230808));
#9285=CARTESIAN_POINT('Ctrl Pts',(0.710849457379773,2.34655128697554,20.2202970722125));
#9286=CARTESIAN_POINT('Ctrl Pts',(0.788731516291807,2.32153773094163,20.2160558213442));
#9287=CARTESIAN_POINT('Ctrl Pts',(0.865224970328303,2.29267005928031,20.2118145704759));
#9288=CARTESIAN_POINT('Ctrl Pts',(0.94128103283111,2.26396745370656,20.207597571189));
#9289=CARTESIAN_POINT('Ctrl Pts',(1.01596388804184,2.23145485462087,20.203380571902));
#9290=CARTESIAN_POINT('Ctrl Pts',(1.08887096805654,2.19529275153078,20.1991635726151));
#9291=CARTESIAN_POINT('Ctrl Pts',(1.1617538777791,2.15914263696905,20.1949479713556));
#9292=CARTESIAN_POINT('Ctrl Pts',(1.23286176508385,2.11934562752412,20.1907323700962));
#9293=CARTESIAN_POINT('Ctrl Pts',(1.3018139754152,2.07610949215442,20.1865167688368));
#9294=CARTESIAN_POINT('Ctrl Pts',(1.37076446521094,2.03287443563788,20.1823012727675));
#9295=CARTESIAN_POINT('Ctrl Pts',(1.43755899154895,1.98620067179806,20.1780857766982));
#9296=CARTESIAN_POINT('Ctrl Pts',(1.50184459234321,1.9363401226152,20.1738702806289));
#9297=CARTESIAN_POINT('Ctrl Pts',(1.56681138471229,1.88595123449486,20.1696101157633));
#9298=CARTESIAN_POINT('Ctrl Pts',(1.6292153714371,1.83230790661776,20.1653499508977));
#9299=CARTESIAN_POINT('Ctrl Pts',(1.68872680245974,1.77571169863075,20.1610897860321));
#9300=CARTESIAN_POINT('Ctrl Pts',(1.74770000140563,1.71962735691947,20.1568681508632));
#9301=CARTESIAN_POINT('Ctrl Pts',(1.80383247632666,1.66064371619445,20.1526465156942));
#9302=CARTESIAN_POINT('Ctrl Pts',(1.85684201911466,1.59908973045611,20.1484248805252));
#9303=CARTESIAN_POINT('Ctrl Pts',(1.91057726705718,1.5366930654117,20.1441454508113));
#9304=CARTESIAN_POINT('Ctrl Pts',(1.96110312556303,1.47165553663225,20.1398660210974));
#9305=CARTESIAN_POINT('Ctrl Pts',(2.00817045738786,1.40435097610058,20.1355865913835));
#9306=CARTESIAN_POINT('Ctrl Pts',(2.05523778921268,1.3370464155689,20.1313071616696));
#9307=CARTESIAN_POINT('Ctrl Pts',(2.09884638929285,1.2674752737451,20.1270277319558));
#9308=CARTESIAN_POINT('Ctrl Pts',(2.13879579919847,1.19603627843431,20.1227483022419));
#9309=CARTESIAN_POINT('Ctrl Pts',(2.17829032470766,1.12541072403142,20.1185176003016));
#9310=CARTESIAN_POINT('Ctrl Pts',(2.21435715494338,1.05269401520267,20.1142868983613));
#9311=CARTESIAN_POINT('Ctrl Pts',(2.24676921058953,0.978252709859208,20.1100561964211));
#9312=CARTESIAN_POINT('Ctrl Pts',(2.27913469903013,0.903918356188484,20.1058315728354));
#9313=CARTESIAN_POINT('Ctrl Pts',(2.30785565738889,0.827864749770065,20.1016069492497));
#9314=CARTESIAN_POINT('Ctrl Pts',(2.33275032093671,0.750483970628084,20.097382325664));
#9315=CARTESIAN_POINT('Ctrl Pts',(2.35774296495488,0.672798636049037,20.0931410747957));
#9316=CARTESIAN_POINT('Ctrl Pts',(2.37887889886291,0.593776073551608,20.0888998239274));
#9317=CARTESIAN_POINT('Ctrl Pts',(2.39602264893294,0.513834327191517,20.0846585730591));
#9318=CARTESIAN_POINT('Ctrl Pts',(2.41306837060006,0.434349689788944,20.0804415737722));
#9319=CARTESIAN_POINT('Ctrl Pts',(2.42616734086377,0.35395681112558,20.0762245744852));
#9320=CARTESIAN_POINT('Ctrl Pts',(2.4352365374527,0.273081044115823,20.0720075751983));
#9321=CARTESIAN_POINT('Ctrl Pts',(2.44430272740455,0.192232089192166,20.0677919739388));
#9322=CARTESIAN_POINT('Ctrl Pts',(2.44934174488293,0.110901025627287,20.0635763726794));
#9323=CARTESIAN_POINT('Ctrl Pts',(2.45032218231688,0.0295203801778828,20.0593607714199));
#9324=CARTESIAN_POINT('Ctrl Pts',(2.45130259528638,-0.0518582346140824,
20.0551452753506));
#9325=CARTESIAN_POINT('Ctrl Pts',(2.44822462504784,-0.133285963790905,20.0509297792814));
#9326=CARTESIAN_POINT('Ctrl Pts',(2.44110897904662,-0.214329658278944,20.0467142832121));
#9327=CARTESIAN_POINT('Ctrl Pts',(2.43391793329733,-0.296232118667681,20.0424541183465));
#9328=CARTESIAN_POINT('Ctrl Pts',(2.42260315950338,-0.377741873168812,20.0381939534809));
#9329=CARTESIAN_POINT('Ctrl Pts',(2.40723966561878,-0.458418413975253,20.0339337886153));
#9330=CARTESIAN_POINT('Ctrl Pts',(2.39201512193373,-0.538365301648864,20.0297121534464));
#9331=CARTESIAN_POINT('Ctrl Pts',(2.3728149691518,-0.617493544060195,20.0254905182774));
#9332=CARTESIAN_POINT('Ctrl Pts',(2.34976298701067,-0.695387773026463,20.0212688831084));
#9333=CARTESIAN_POINT('Ctrl Pts',(2.32639542127129,-0.7743483806195,20.0169894533946));
#9334=CARTESIAN_POINT('Ctrl Pts',(2.29906992801853,-0.852040464810376,20.0127100236807));
#9335=CARTESIAN_POINT('Ctrl Pts',(2.2679659234488,-0.928052164522561,20.0084305939668));
#9336=CARTESIAN_POINT('Ctrl Pts',(2.23686191887908,-1.00406386423475,20.0041511642529));
#9337=CARTESIAN_POINT('Ctrl Pts',(2.20197967069622,-1.07839476317502,19.999871734539));
#9338=CARTESIAN_POINT('Ctrl Pts',(2.16354588173339,-1.15066044845319,19.9955923048252));
#9339=CARTESIAN_POINT('Ctrl Pts',(2.12554971953235,-1.22210327970913,19.9913616028849));
#9340=CARTESIAN_POINT('Ctrl Pts',(2.08393960868889,-1.29179642615623,19.9871309009447));
#9341=CARTESIAN_POINT('Ctrl Pts',(2.03890079209262,-1.35935051035563,19.9829001990044));
#9342=CARTESIAN_POINT('Ctrl Pts',(1.99392668388306,-1.42680753792399,19.9786755754187));
#9343=CARTESIAN_POINT('Ctrl Pts',(1.94553390923085,-1.49213122321285,19.9744509518331));
#9344=CARTESIAN_POINT('Ctrl Pts',(1.8939537027883,-1.55495646938893,19.9702263282474));
#9345=CARTESIAN_POINT('Ctrl Pts',(1.84217048685805,-1.61802898330433,19.9659850773791));
#9346=CARTESIAN_POINT('Ctrl Pts',(1.78717491795345,-1.67858293021693,19.9617438265108));
#9347=CARTESIAN_POINT('Ctrl Pts',(1.72924512267815,-1.73627807556676,19.9575025756425));
#9348=CARTESIAN_POINT('Ctrl Pts',(1.67164657145925,-1.7936433185945,19.9532855763556));
#9349=CARTESIAN_POINT('Ctrl Pts',(1.6111475916028,-1.84818203326638,19.9490685770686));
#9350=CARTESIAN_POINT('Ctrl Pts',(1.5480608525303,-1.89959412687636,19.9448515777817));
#9351=CARTESIAN_POINT('Ctrl Pts',(1.48499502809192,-1.95098917625259,19.9406359765222));
#9352=CARTESIAN_POINT('Ctrl Pts',(1.41934350830166,-1.99925936940489,19.9364203752628));
#9353=CARTESIAN_POINT('Ctrl Pts',(1.35145293885315,-2.04414412507171,19.9322047740033));
#9354=CARTESIAN_POINT('Ctrl Pts',(1.28356406344963,-2.08902776074799,19.927989277934));
#9355=CARTESIAN_POINT('Ctrl Pts',(1.21343663801125,-2.13052587132057,19.9237737818647));
#9356=CARTESIAN_POINT('Ctrl Pts',(1.14144604713651,-2.16842135469019,19.9195582857954));
#9357=CARTESIAN_POINT('Ctrl Pts',(1.06869262005342,-2.20671839118635,19.9152981209298));
#9358=CARTESIAN_POINT('Ctrl Pts',(0.994036728184708,-2.24133575668633,19.9110379560643));
#9359=CARTESIAN_POINT('Ctrl Pts',(0.91788934197804,-2.27209801854654,19.9067777911987));
#9360=CARTESIAN_POINT('Ctrl Pts',(0.84243064641623,-2.30258206098238,19.9025561560297));
#9361=CARTESIAN_POINT('Ctrl Pts',(0.765507791155449,-2.32928035591837,19.8983345208607));
#9362=CARTESIAN_POINT('Ctrl Pts',(0.687537015936515,-2.35207208684537,19.8941128856918));
#9363=CARTESIAN_POINT('Ctrl Pts',(0.608498814165895,-2.37517583850939,19.8898334559779));
#9364=CARTESIAN_POINT('Ctrl Pts',(0.528384264145614,-2.39426513924351,19.885554026264));
#9365=CARTESIAN_POINT('Ctrl Pts',(0.447636779228395,-2.40926784809868,19.8812745965501));
#9366=CARTESIAN_POINT('Ctrl Pts',(0.366889294311188,-2.42427055695384,19.8769951668362));
#9367=CARTESIAN_POINT('Ctrl Pts',(0.285509369436723,-2.43518667361799,19.8727157371223));
#9368=CARTESIAN_POINT('Ctrl Pts',(0.203942942233879,-2.4419986745109,19.8684363074084));
#9369=CARTESIAN_POINT('Ctrl Pts',(0.123305272054182,-2.4487331104805,19.8642056054682));
#9370=CARTESIAN_POINT('Ctrl Pts',(0.0421820279329571,-2.45148179185811,
19.8599749035279));
#9371=CARTESIAN_POINT('Ctrl Pts',(-0.0389991254238726,-2.45018964943863,
19.8557442015877));
#9372=CARTESIAN_POINT('Ctrl Pts',(-0.120063643801093,-2.44889936347225,
19.851519578002));
#9373=CARTESIAN_POINT('Ctrl Pts',(-0.201185445118751,-2.44357979119285,
19.8472949544163));
#9374=CARTESIAN_POINT('Ctrl Pts',(-0.281932378287597,-2.4342276771233,19.8430703308306));
#9375=CARTESIAN_POINT('Ctrl Pts',(-0.362997115410038,-2.42483875498304,
19.8388290799624));
#9376=CARTESIAN_POINT('Ctrl Pts',(-0.443683554332948,-2.41138544090157,
19.8345878290941));
#9377=CARTESIAN_POINT('Ctrl Pts',(-0.523555059252396,-2.39391736489195,
19.8303465782258));
#9378=CARTESIAN_POINT('Ctrl Pts',(-0.60296985685637,-2.37654917178937,19.8261295789388));
#9379=CARTESIAN_POINT('Ctrl Pts',(-0.681578555905265,-2.3552121055536,19.8219125796519));
#9380=CARTESIAN_POINT('Ctrl Pts',(-0.758959568270084,-2.33000657160689,
19.8176955803649));
#9381=CARTESIAN_POINT('Ctrl Pts',(-0.836314927136413,-2.30480939384611,
19.8134799791055));
#9382=CARTESIAN_POINT('Ctrl Pts',(-0.91244296571893,-2.27574643908791,19.8092643778461));
#9383=CARTESIAN_POINT('Ctrl Pts',(-0.986936920276588,-2.24296807052507,
19.8050487765866));
#9384=CARTESIAN_POINT('Ctrl Pts',(-1.06142901601773,-2.21019051986716,19.8008332805173));
#9385=CARTESIAN_POINT('Ctrl Pts',(-1.13428668356631,-2.1736979280292,19.796617784448));
#9386=CARTESIAN_POINT('Ctrl Pts',(-1.20512415503052,-2.13368836078795,19.7924022883788));
#9387=CARTESIAN_POINT('Ctrl Pts',(-1.27671224386715,-2.09325483888524,19.7881421235132));
#9388=CARTESIAN_POINT('Ctrl Pts',(-1.34623663860387,-2.04922958793333,19.7838819586476));
#9389=CARTESIAN_POINT('Ctrl Pts',(-1.4133273386569,-2.00186315311636,19.779621793782));
#9390=CARTESIAN_POINT('Ctrl Pts',(-1.47981125836186,-1.95492510884805,19.775400158613));
#9391=CARTESIAN_POINT('Ctrl Pts',(-1.54390499578219,-1.90470641275385,19.7711785234441));
#9392=CARTESIAN_POINT('Ctrl Pts',(-1.60528161640228,-1.85149161003794,19.7669568882751));
#9393=CARTESIAN_POINT('Ctrl Pts',(-1.66749848818512,-1.7975482921414,19.7626774585612));
#9394=CARTESIAN_POINT('Ctrl Pts',(-1.72692292784109,-1.74052655506609,19.7583980288473));
#9395=CARTESIAN_POINT('Ctrl Pts',(-1.78325421308252,-1.6807601439597,19.7541185991334));
#9396=CARTESIAN_POINT('Ctrl Pts',(-1.83958549832394,-1.62099373285332,19.7498391694195));
#9397=CARTESIAN_POINT('Ctrl Pts',(-1.89282336092224,-1.55848306367117,19.7455597397056));
#9398=CARTESIAN_POINT('Ctrl Pts',(-1.94271163188047,-1.49359357435559,19.7412803099917));
#9399=CARTESIAN_POINT('Ctrl Pts',(-1.99209745832981,-1.42935761275235,19.7370439801071));
#9400=CARTESIAN_POINT('Ctrl Pts',(-2.03838923801735,-1.36254563061871,19.7328076502224));
#9401=CARTESIAN_POINT('Ctrl Pts',(-2.08130749356317,-1.29348728916746,19.7285713203378));
#9402=CARTESIAN_POINT('Ctrl Pts',(-2.12416473962921,-1.22452711604652,19.7243410125125));
#9403=CARTESIAN_POINT('Ctrl Pts',(-2.16365774029283,-1.15332731247133,19.7201107046873));
#9404=CARTESIAN_POINT('Ctrl Pts',(-2.19954791923169,-1.08024960125128,19.715880396862));
#9405=CARTESIAN_POINT('Ctrl Pts',(-2.23539796364597,-1.00725360985776,19.7116548196176));
#9406=CARTESIAN_POINT('Ctrl Pts',(-2.26765298492923,-0.932384294427066,
19.7074292423732));
#9407=CARTESIAN_POINT('Ctrl Pts',(-2.29611906075015,-0.856030086422113,
19.7032036651288));
#9408=CARTESIAN_POINT('Ctrl Pts',(-2.32456236915016,-0.779736947192605,
19.6989814675386));
#9409=CARTESIAN_POINT('Ctrl Pts',(-2.34922259155874,-0.701961707256178,
19.6947592699485));
#9410=CARTESIAN_POINT('Ctrl Pts',(-2.36995348616866,-0.623113732313,19.6905370723584));
#9411=CARTESIAN_POINT('Ctrl Pts',(-2.39067451838713,-0.544303268032445,
19.6863168834113));
#9412=CARTESIAN_POINT('Ctrl Pts',(-2.40746982107492,-0.464421530264314,
19.6820966944641));
#9413=CARTESIAN_POINT('Ctrl Pts',(-2.42024309441003,-0.383892711523121,
19.677876505517));
#9414=CARTESIAN_POINT('Ctrl Pts',(-2.43301721239596,-0.303358567699503,
19.6736560375038));
#9415=CARTESIAN_POINT('Ctrl Pts',(-2.44176868987403,-0.222177713514921,
19.6694355694907));
#9416=CARTESIAN_POINT('Ctrl Pts',(-2.44645260879298,-0.140783105982285,
19.6652151014775));
#9417=CARTESIAN_POINT('Ctrl Pts',(-2.4491855556258,-0.0932914352864258,
19.6627525663891));
#9418=CARTESIAN_POINT('Ctrl Pts',(-2.45053470395958,-0.0457271215581164,
19.6602900313006));
#9419=CARTESIAN_POINT('Ctrl Pts',(-2.45049932159773,0.00182341686532293,
19.6578274962121));
#9420=CARTESIAN_POINT('',(-2.45075211844691,0.000775521760612707,18.8578274962121));
#9421=CARTESIAN_POINT('Ctrl Pts',(-2.45049932159731,0.00182341742318767,
19.6578274961832));
#9422=CARTESIAN_POINT('Ctrl Pts',(-2.45042940194533,0.095788769285848,19.6529612426404));
#9423=CARTESIAN_POINT('Ctrl Pts',(-2.44495079787585,0.189533578803116,19.6480949890976));
#9424=CARTESIAN_POINT('Ctrl Pts',(-2.43416311526941,0.282489253356498,19.6432287355548));
#9425=CARTESIAN_POINT('Ctrl Pts',(-2.42327182879274,0.376337665302642,19.6383157469791));
#9426=CARTESIAN_POINT('Ctrl Pts',(-2.40696909967135,0.469381553086519,19.6334027584035));
#9427=CARTESIAN_POINT('Ctrl Pts',(-2.38540708047696,0.561055532376605,19.6284897698279));
#9428=CARTESIAN_POINT('Ctrl Pts',(-2.3643914766168,0.650406349462673,19.6237012840769));
#9429=CARTESIAN_POINT('Ctrl Pts',(-2.33838008968937,0.738455789770857,19.618912798326));
#9430=CARTESIAN_POINT('Ctrl Pts',(-2.30755712572132,0.824700164625154,19.614124312575));
#9431=CARTESIAN_POINT('Ctrl Pts',(-2.28032455570944,0.900898416642212,19.6098936106347));
#9432=CARTESIAN_POINT('Ctrl Pts',(-2.24926248145931,0.975889639658068,19.6056629086945));
#9433=CARTESIAN_POINT('Ctrl Pts',(-2.2144977131412,1.04926170638807,19.6014322067542));
#9434=CARTESIAN_POINT('Ctrl Pts',(-2.17978289222936,1.12252835764708,19.5972075831685));
#9435=CARTESIAN_POINT('Ctrl Pts',(-2.14137614001205,1.19418005603882,19.5929829595828));
#9436=CARTESIAN_POINT('Ctrl Pts',(-2.09945329369666,1.2638220276551,19.5887583359971));
#9437=CARTESIAN_POINT('Ctrl Pts',(-2.05736544735254,1.33373809629311,19.5845170851289));
#9438=CARTESIAN_POINT('Ctrl Pts',(-2.01173392995358,1.40162813757825,19.5802758342606));
#9439=CARTESIAN_POINT('Ctrl Pts',(-1.96278458077779,1.46711517593574,19.5760345833923));
#9440=CARTESIAN_POINT('Ctrl Pts',(-1.91411512523693,1.5322277577271,19.5718175841053));
#9441=CARTESIAN_POINT('Ctrl Pts',(-1.86216595908345,1.59496436663864,19.5676005848184));
#9442=CARTESIAN_POINT('Ctrl Pts',(-1.80720292120841,1.65498273452499,19.5633835855314));
#9443=CARTESIAN_POINT('Ctrl Pts',(-1.75225810478283,1.71498120500937,19.5591679842719));
#9444=CARTESIAN_POINT('Ctrl Pts',(-1.6943017146434,1.77226288130959,19.5549523830125));
#9445=CARTESIAN_POINT('Ctrl Pts',(-1.63363893730656,1.82651966113587,19.550736781753));
#9446=CARTESIAN_POINT('Ctrl Pts',(-1.57297767366264,1.8807750871154,19.5465212856837));
#9447=CARTESIAN_POINT('Ctrl Pts',(-1.50961050445397,1.93200545746552,19.5423057896144));
#9448=CARTESIAN_POINT('Ctrl Pts',(-1.44387735729821,1.97994152112671,19.5380902935451));
#9449=CARTESIAN_POINT('Ctrl Pts',(-1.37744767988608,2.02838553123738,19.5338301286795));
#9450=CARTESIAN_POINT('Ctrl Pts',(-1.30860196654172,2.07346470535285,19.529569963814));
#9451=CARTESIAN_POINT('Ctrl Pts',(-1.23772139805673,2.1149458600145,19.5253097989484));
#9452=CARTESIAN_POINT('Ctrl Pts',(-1.16748188617039,2.15605185165922,19.5210881637794));
#9453=CARTESIAN_POINT('Ctrl Pts',(-1.09524462393809,2.19362448211211,19.5168665286104));
#9454=CARTESIAN_POINT('Ctrl Pts',(-1.02140392707162,2.22748384231237,19.5126448934415));
#9455=CARTESIAN_POINT('Ctrl Pts',(-0.94655234477819,2.26180674003659,19.5083654637276));
#9456=CARTESIAN_POINT('Ctrl Pts',(-0.870053552590683,2.29231374449871,19.5040860340137));
#9457=CARTESIAN_POINT('Ctrl Pts',(-0.792335812248403,2.31886916634567,19.4998066042998));
#9458=CARTESIAN_POINT('Ctrl Pts',(-0.714618071906124,2.34542458819263,19.495527174586));
#9459=CARTESIAN_POINT('Ctrl Pts',(-0.635681873070141,2.36802835533124,19.4912477448721));
#9460=CARTESIAN_POINT('Ctrl Pts',(-0.555965896586985,2.38659845215575,19.4869683151582));
#9461=CARTESIAN_POINT('Ctrl Pts',(-0.477157606948763,2.40495710036807,19.482737613218));
#9462=CARTESIAN_POINT('Ctrl Pts',(-0.397290797063172,2.41944256428239,19.4785069112777));
#9463=CARTESIAN_POINT('Ctrl Pts',(-0.316780622573661,2.42993832990919,19.4742762093374));
#9464=CARTESIAN_POINT('Ctrl Pts',(-0.236386119051856,2.44041901600877,19.4700515857518));
#9465=CARTESIAN_POINT('Ctrl Pts',(-0.155350543957463,2.44692132847501,19.4658269621661));
#9466=CARTESIAN_POINT('Ctrl Pts',(-0.0741010067707996,2.44937936849226,
19.4616023385804));
#9467=CARTESIAN_POINT('Ctrl Pts',(0.00746831251923698,2.45184708286871,
19.4573610877121));
#9468=CARTESIAN_POINT('Ctrl Pts',(0.0892528195595222,2.4502385139366,19.4531198368438));
#9469=CARTESIAN_POINT('Ctrl Pts',(0.170813297239063,2.4445394387259,19.4488785859755));
#9470=CARTESIAN_POINT('Ctrl Pts',(0.251907410013752,2.43887295097353,19.4446615866886));
#9471=CARTESIAN_POINT('Ctrl Pts',(0.332779579893849,2.4291626419863,19.4404445874016));
#9472=CARTESIAN_POINT('Ctrl Pts',(0.412998114036378,2.41544670978318,19.4362275881146));
#9473=CARTESIAN_POINT('Ctrl Pts',(0.493190053979881,2.40173532471166,19.4320119868552));
#9474=CARTESIAN_POINT('Ctrl Pts',(0.572728330459702,2.3840210318284,19.4277963855957));
#9475=CARTESIAN_POINT('Ctrl Pts',(0.65118867256248,2.36239360876343,19.4235807843363));
#9476=CARTESIAN_POINT('Ctrl Pts',(0.729647056877126,2.34076672535851,19.419365288267));
#9477=CARTESIAN_POINT('Ctrl Pts',(0.807027112241932,2.3152270305395,19.4151497921977));
#9478=CARTESIAN_POINT('Ctrl Pts',(0.882918422963899,2.28591454529493,19.4109342961284));
#9479=CARTESIAN_POINT('Ctrl Pts',(0.959613903217039,2.25629145522232,19.4066741312628));
#9480=CARTESIAN_POINT('Ctrl Pts',(1.03478844276865,2.2228153026946,19.4024139663972));
#9481=CARTESIAN_POINT('Ctrl Pts',(1.10803961507543,2.18568032004305,19.3981538015317));
#9482=CARTESIAN_POINT('Ctrl Pts',(1.18062829061635,2.1488811928479,19.3939321663627));
#9483=CARTESIAN_POINT('Ctrl Pts',(1.25132787185725,2.10848943841322,19.3897105311937));
#9484=CARTESIAN_POINT('Ctrl Pts',(1.3197736117042,2.06473917574333,19.3854888960248));
#9485=CARTESIAN_POINT('Ctrl Pts',(1.38915637955753,2.02038996825234,19.3812094663109));
#9486=CARTESIAN_POINT('Ctrl Pts',(1.45622272539394,1.97258988683397,19.376930036597));
#9487=CARTESIAN_POINT('Ctrl Pts',(1.52062670138999,1.92162553194419,19.3726506068831));
#9488=CARTESIAN_POINT('Ctrl Pts',(1.58503067738604,1.87066117705441,19.3683711771692));
#9489=CARTESIAN_POINT('Ctrl Pts',(1.64677195782055,1.81653292134733,19.3640917474553));
#9490=CARTESIAN_POINT('Ctrl Pts',(1.70554408044883,1.75956518482435,19.3598123177414));
#9491=CARTESIAN_POINT('Ctrl Pts',(1.76364699365454,1.70324611206166,19.3555816158012));
#9492=CARTESIAN_POINT('Ctrl Pts',(1.8190665934253,1.64394009257529,19.351350913861));
#9493=CARTESIAN_POINT('Ctrl Pts',(1.87148014956442,1.58193308954151,19.3471202119207));
#9494=CARTESIAN_POINT('Ctrl Pts',(1.92381840184534,1.5200151735094,19.342895588335));
#9495=CARTESIAN_POINT('Ctrl Pts',(1.97315889030848,1.45540433311514,19.3386709647494));
#9496=CARTESIAN_POINT('Ctrl Pts',(2.01921496789646,1.38842398546802,19.3344463411637));
#9497=CARTESIAN_POINT('Ctrl Pts',(2.06545231309397,1.32118001642413,19.3302050902954));
#9498=CARTESIAN_POINT('Ctrl Pts',(2.10837899763103,1.2515481785876,19.3259638394271));
#9499=CARTESIAN_POINT('Ctrl Pts',(2.14774526609153,1.17989004656427,19.3217225885588));
#9500=CARTESIAN_POINT('Ctrl Pts',(2.18688643721838,1.10864165757942,19.3175055892719));
#9501=CARTESIAN_POINT('Ctrl Pts',(2.22250757270791,1.03539049603139,19.3132885899849));
#9502=CARTESIAN_POINT('Ctrl Pts',(2.25440706421273,0.960520191785537,19.309071590698));
#9503=CARTESIAN_POINT('Ctrl Pts',(2.28629598033826,0.885674708683485,19.3048559894386));
#9504=CARTESIAN_POINT('Ctrl Pts',(2.31446552046429,0.809211576346526,19.3006403881792));
#9505=CARTESIAN_POINT('Ctrl Pts',(2.33876146051008,0.7315361104093,19.2964247869197));
#9506=CARTESIAN_POINT('Ctrl Pts',(2.36305679430942,0.653862582675529,19.2922092908504));
#9507=CARTESIAN_POINT('Ctrl Pts',(2.3834785824084,0.574977225666107,19.2879937947812));
#9508=CARTESIAN_POINT('Ctrl Pts',(2.39992234458836,0.495300908484432,19.2837782987119));
#9509=CARTESIAN_POINT('Ctrl Pts',(2.4165403503333,0.414780314585646,19.2795181338463));
#9510=CARTESIAN_POINT('Ctrl Pts',(2.42909540951884,0.333452369365408,19.2752579689807));
#9511=CARTESIAN_POINT('Ctrl Pts',(2.43753294594085,0.251760575652595,19.2709978041151));
#9512=CARTESIAN_POINT('Ctrl Pts',(2.44589417176715,0.170807617202951,19.2667761689461));
#9513=CARTESIAN_POINT('Ctrl Pts',(2.45021209118132,0.0894978380503747,19.2625545337772));
#9514=CARTESIAN_POINT('Ctrl Pts',(2.45048606309993,0.00826465686051566,
19.2583328986082));
#9515=CARTESIAN_POINT('Ctrl Pts',(2.45076378571743,-0.0740806134972785,
19.2540534688943));
#9516=CARTESIAN_POINT('Ctrl Pts',(2.44688602179809,-0.156346678642749,19.2497740391804));
#9517=CARTESIAN_POINT('Ctrl Pts',(2.4389064325815,-0.238087511458697,19.2454946094665));
#9518=CARTESIAN_POINT('Ctrl Pts',(2.4309268433649,-0.319828344274645,19.2412151797526));
#9519=CARTESIAN_POINT('Ctrl Pts',(2.4188455658135,-0.401043469149177,19.2369357500387));
#9520=CARTESIAN_POINT('Ctrl Pts',(2.40276943619433,-0.481299580812578,19.2326563203248));
#9521=CARTESIAN_POINT('Ctrl Pts',(2.38687635760244,-0.560641855375045,19.2284256183845));
#9522=CARTESIAN_POINT('Ctrl Pts',(2.36701920340031,-0.639345282321367,19.2241949164443));
#9523=CARTESIAN_POINT('Ctrl Pts',(2.34326366932798,-0.716983699959484,19.219964214504));
#9524=CARTESIAN_POINT('Ctrl Pts',(2.31954226542159,-0.794510572554247,19.2157395909183));
#9525=CARTESIAN_POINT('Ctrl Pts',(2.29193374025496,-0.87097503381822,19.2115149673326));
#9526=CARTESIAN_POINT('Ctrl Pts',(2.26055481508318,-0.945960981227155,19.207290343747));
#9527=CARTESIAN_POINT('Ctrl Pts',(2.22905238867009,-1.02124205848949,19.2030490928787));
#9528=CARTESIAN_POINT('Ctrl Pts',(2.19374991270444,-1.0950324933475,19.1988078420104));
#9529=CARTESIAN_POINT('Ctrl Pts',(2.15481616321522,-1.16692654128117,19.1945665911421));
#9530=CARTESIAN_POINT('Ctrl Pts',(2.11610503790499,-1.23840949720328,19.1903495918551));
#9531=CARTESIAN_POINT('Ctrl Pts',(2.07380427750137,-1.30801728147344,19.1861325925682));
#9532=CARTESIAN_POINT('Ctrl Pts',(2.02812726855209,-1.37537268860314,19.1819155932812));
#9533=CARTESIAN_POINT('Ctrl Pts',(1.98246540253054,-1.44270576594186,19.1776999920218));
#9534=CARTESIAN_POINT('Ctrl Pts',(1.93342977151758,-1.50778756438723,19.1734843907623));
#9535=CARTESIAN_POINT('Ctrl Pts',(1.8812776489379,-1.57026897619697,19.1692687895029));
#9536=CARTESIAN_POINT('Ctrl Pts',(1.82912682768837,-1.63274882893412,19.1650532934336));
#9537=CARTESIAN_POINT('Ctrl Pts',(1.77385996832874,-1.69262806770863,19.1608377973643));
#9538=CARTESIAN_POINT('Ctrl Pts',(1.71577435289581,-1.74959098647225,19.156622301295));
#9539=CARTESIAN_POINT('Ctrl Pts',(1.65707324299192,-1.8071575032401,19.1523621364294));
#9540=CARTESIAN_POINT('Ctrl Pts',(1.59549361899203,-1.86174517669218,19.1481019715638));
#9541=CARTESIAN_POINT('Ctrl Pts',(1.53137881103256,-1.91306800378881,19.1438418066982));
#9542=CARTESIAN_POINT('Ctrl Pts',(1.46784386891811,-1.96392665801415,19.1396201715293));
#9543=CARTESIAN_POINT('Ctrl Pts',(1.40181983312291,-2.01157905891122,19.1353985363603));
#9544=CARTESIAN_POINT('Ctrl Pts',(1.33367075656057,-2.05579000948423,19.1311769011913));
#9545=CARTESIAN_POINT('Ctrl Pts',(1.26458871333723,-2.10060621173513,19.1268974714774));
#9546=CARTESIAN_POINT('Ctrl Pts',(1.1933234328532,-2.14188577477813,19.1226180417635));
#9547=CARTESIAN_POINT('Ctrl Pts',(1.12027896859355,-2.17943233033902,19.1183386120496));
#9548=CARTESIAN_POINT('Ctrl Pts',(1.04723450433389,-2.21697888589991,19.1140591823357));
#9549=CARTESIAN_POINT('Ctrl Pts',(0.972411330325981,-2.25079229162899,19.1097797526218));
#9550=CARTESIAN_POINT('Ctrl Pts',(0.896231593655689,-2.28072777431534,19.105500322908));
#9551=CARTESIAN_POINT('Ctrl Pts',(0.82091927839707,-2.31032239629796,19.1012696209677));
#9552=CARTESIAN_POINT('Ctrl Pts',(0.743997881582165,-2.33623831222196,19.0970389190274));
#9553=CARTESIAN_POINT('Ctrl Pts',(0.66586127031152,-2.35830002728642,19.0928082170871));
#9554=CARTESIAN_POINT('Ctrl Pts',(0.587836919851385,-2.38033004573678,19.0885835935015));
#9555=CARTESIAN_POINT('Ctrl Pts',(0.508601266211257,-2.39851673566438,19.0843589699158));
#9556=CARTESIAN_POINT('Ctrl Pts',(0.428567344988989,-2.41273294850655,19.0801343463301));
#9557=CARTESIAN_POINT('Ctrl Pts',(0.348218426087391,-2.4270051135498,19.0758930954618));
#9558=CARTESIAN_POINT('Ctrl Pts',(0.267065384156518,-2.43727530688736,19.0716518445935));
#9559=CARTESIAN_POINT('Ctrl Pts',(0.185540729295466,-2.44346575334554,19.0674105937252));
#9560=CARTESIAN_POINT('Ctrl Pts',(0.104482234503321,-2.44962080267199,19.0631935944383));
#9561=CARTESIAN_POINT('Ctrl Pts',(0.0230568334204954,-2.45174259914225,
19.0589765951513));
#9562=CARTESIAN_POINT('Ctrl Pts',(-0.058302805595985,-2.4498063255816,19.0547595958643));
#9563=CARTESIAN_POINT('Ctrl Pts',(-0.139635472112221,-2.447870693938,19.0505439946049));
#9564=CARTESIAN_POINT('Ctrl Pts',(-0.22090195529595,-2.44187967493441,19.0463283933455));
#9565=CARTESIAN_POINT('Ctrl Pts',(-0.301669449306597,-2.43186056207075,
19.042112792086));
#9566=CARTESIAN_POINT('Ctrl Pts',(-0.382434927959681,-2.42184169920983,
19.0378972960167));
#9567=CARTESIAN_POINT('Ctrl Pts',(-0.462700980805989,-2.40779500065838,
19.0336817999474));
#9568=CARTESIAN_POINT('Ctrl Pts',(-0.542041223593945,-2.38979948153078,
19.0294663038781));
#9569=CARTESIAN_POINT('Ctrl Pts',(-0.622222181942375,-2.37161327590641,
19.0252061390125));
#9570=CARTESIAN_POINT('Ctrl Pts',(-0.701457116994926,-2.34939415684086,
19.020945974147));
#9571=CARTESIAN_POINT('Ctrl Pts',(-0.779319686541284,-2.32327593629538,
19.0166858092814));
#9572=CARTESIAN_POINT('Ctrl Pts',(-0.856478053016731,-2.29739393362997,
19.0124641741124));
#9573=CARTESIAN_POINT('Ctrl Pts',(-0.932288362691395,-2.26768330319229,
19.0082425389434));
#9574=CARTESIAN_POINT('Ctrl Pts',(-1.00635576936152,-2.23432278676846,19.0040209037745));
#9575=CARTESIAN_POINT('Ctrl Pts',(-1.08143716513512,-2.20050556203445,18.9997414740606));
#9576=CARTESIAN_POINT('Ctrl Pts',(-1.15472713540503,-2.16293798578523,18.9954620443467));
#9577=CARTESIAN_POINT('Ctrl Pts',(-1.22584182272403,-2.12185345291814,18.9911826146329));
#9578=CARTESIAN_POINT('Ctrl Pts',(-1.29695651004303,-2.08076892005105,18.986903184919));
#9579=CARTESIAN_POINT('Ctrl Pts',(-1.3658955380855,-2.03616775203834,18.9826237552051));
#9580=CARTESIAN_POINT('Ctrl Pts',(-1.43230863225199,-1.98832649028685,18.9783443254913));
#9581=CARTESIAN_POINT('Ctrl Pts',(-1.49744651369067,-1.94140383934044,18.9741470660679));
#9582=CARTESIAN_POINT('Ctrl Pts',(-1.5604081629043,-1.89118166509442,18.9699498066445));
#9583=CARTESIAN_POINT('Ctrl Pts',(-1.62083593804614,-1.83789039715052,18.9657525472211));
#9584=CARTESIAN_POINT('Ctrl Pts',(-1.68117667131845,-1.78467589145015,18.9615613336484));
#9585=CARTESIAN_POINT('Ctrl Pts',(-1.73899042455984,-1.7284013784966,18.9573701200757));
#9586=CARTESIAN_POINT('Ctrl Pts',(-1.79394951889508,-1.66933980173484,18.953178906503));
#9587=CARTESIAN_POINT('Ctrl Pts',(-1.84884541218041,-1.61034614373532,18.9489925126804));
#9588=CARTESIAN_POINT('Ctrl Pts',(-1.90089284763804,-1.54857213380597,18.9448061188577));
#9589=CARTESIAN_POINT('Ctrl Pts',(-1.949799360154,-1.48432904207357,18.9406197250351));
#9590=CARTESIAN_POINT('Ctrl Pts',(-1.99867561180049,-1.42012570070802,18.9364359215406));
#9591=CARTESIAN_POINT('Ctrl Pts',(-2.04441451086891,-1.35345668447874,18.9322521180462));
#9592=CARTESIAN_POINT('Ctrl Pts',(-2.08676327369891,-1.28466699558345,18.9280683145517));
#9593=CARTESIAN_POINT('Ctrl Pts',(-2.12909933263273,-1.21589794240471,18.9238857661259));
#9594=CARTESIAN_POINT('Ctrl Pts',(-2.16804702656787,-1.1450098823527,18.9197032177001));
#9595=CARTESIAN_POINT('Ctrl Pts',(-2.20339726727572,-1.07237620850235,18.9155206692743));
#9596=CARTESIAN_POINT('Ctrl Pts',(-2.23874817182224,-0.999741170671455,
18.9113380423049));
#9597=CARTESIAN_POINT('Ctrl Pts',(-2.27050128388473,-0.925360880408144,
18.9071554153354));
#9598=CARTESIAN_POINT('Ctrl Pts',(-2.29849448721695,-0.849631297818818,
18.902972788366));
#9599=CARTESIAN_POINT('Ctrl Pts',(-2.32651476312664,-0.773828476201883,
18.8987861163256));
#9600=CARTESIAN_POINT('Ctrl Pts',(-2.35076770707159,-0.6966742020151,18.8945994442852));
#9601=CARTESIAN_POINT('Ctrl Pts',(-2.37114045908617,-0.618581581753452,
18.8904127722448));
#9602=CARTESIAN_POINT('Ctrl Pts',(-2.39152389618695,-0.540448003531031,
18.8862239043817));
#9603=CARTESIAN_POINT('Ctrl Pts',(-2.40802299471504,-0.461375563097046,
18.8820350365187));
#9604=CARTESIAN_POINT('Ctrl Pts',(-2.42057614060227,-0.38178711024209,18.8778461686556));
#9605=CARTESIAN_POINT('Ctrl Pts',(-2.4331498751215,-0.302068122987079,18.8736504305577));
#9606=CARTESIAN_POINT('Ctrl Pts',(-2.44176468746064,-0.221831904193627,
18.8694546924599));
#9607=CARTESIAN_POINT('Ctrl Pts',(-2.44641093600418,-0.141505414027701,
18.8652589543621));
#9608=CARTESIAN_POINT('Ctrl Pts',(-2.44915406890085,-0.0940808659040406,
18.8627818016454));
#9609=CARTESIAN_POINT('Ctrl Pts',(-2.45051487676998,-0.0466248548202002,
18.8603046489288));
#9610=CARTESIAN_POINT('Ctrl Pts',(-2.45049987730867,0.000775441940834045,
18.8578274962121));
#9611=CARTESIAN_POINT('',(-2.45034175952418,-0.00225396745384549,18.0578274962121));
#9612=CARTESIAN_POINT('Ctrl Pts',(-2.45424115301751,0.000776625838913008,
18.8578274962121));
#9613=CARTESIAN_POINT('Ctrl Pts',(-2.45441689260005,0.0431881474040568,
18.8556144401662));
#9614=CARTESIAN_POINT('Ctrl Pts',(-2.45341292665042,0.0855911761083251,
18.8534013841204));
#9615=CARTESIAN_POINT('Ctrl Pts',(-2.40888053683753,0.93884568070453,18.8088029956023));
#9616=CARTESIAN_POINT('Ctrl Pts',(-1.43961464987565,2.51450507031629,18.7240323306577));
#9617=CARTESIAN_POINT('Ctrl Pts',(1.33466462877634,2.57174968017351,18.5968763332411));
#9618=CARTESIAN_POINT('Ctrl Pts',(2.8848211319999,0.270246415603432,18.4697203358243));
#9619=CARTESIAN_POINT('Ctrl Pts',(1.78908804275333,-2.27912045843473,18.3425643384076));
#9620=CARTESIAN_POINT('Ctrl Pts',(-0.947554210610886,-2.73813204698707,
18.2154083409909));
#9621=CARTESIAN_POINT('Ctrl Pts',(-2.34155166386826,-1.2062176413868,18.1204960602591));
#9622=CARTESIAN_POINT('Ctrl Pts',(-2.45213219889459,-0.19741509474636,18.0679691119994));
#9623=CARTESIAN_POINT('Ctrl Pts',(-2.45034175952418,-0.00225396745384549,
18.0578274962121));
#9624=CARTESIAN_POINT('',(-2.45013024099823,0.000414097004077804,17.2578274769431));
#9625=CARTESIAN_POINT('Ctrl Pts',(-2.45034175952418,-0.00225396745384549,
18.0578274962121));
#9626=CARTESIAN_POINT('Ctrl Pts',(-2.44464933131434,0.618230995521739,18.0255837795272));
#9627=CARTESIAN_POINT('Ctrl Pts',(-1.89007728857131,2.06341743069497,17.9509547303701));
#9628=CARTESIAN_POINT('Ctrl Pts',(0.540405443485623,2.84660992154335,17.8339403487407));
#9629=CARTESIAN_POINT('Ctrl Pts',(2.68589061564201,1.08683839166205,17.7067843513239));
#9630=CARTESIAN_POINT('Ctrl Pts',(2.36794055168644,-1.6697555606909,17.5796283539071));
#9631=CARTESIAN_POINT('Ctrl Pts',(-0.121828482878495,-2.89488927414131,
17.4524723564905));
#9632=CARTESIAN_POINT('Ctrl Pts',(-2.12790075727867,-1.68857036130835,17.3452054039253));
#9633=CARTESIAN_POINT('Ctrl Pts',(-2.44587085179714,-0.434202241831305,
17.2803237838326));
#9634=CARTESIAN_POINT('Ctrl Pts',(-2.44652391920135,0.000413115175876,17.2578274962121));
#9635=CARTESIAN_POINT('',(-2.45049912112546,0.00207541883864715,16.4578274962121));
#9636=CARTESIAN_POINT('Ctrl Pts',(-2.45049996499496,0.000414197662163056,
17.2578274749676));
#9637=CARTESIAN_POINT('Ctrl Pts',(-2.45048532431696,0.0870322165542004,
17.2533512807253));
#9638=CARTESIAN_POINT('Ctrl Pts',(-2.4458738856359,0.17353746902709,17.2488750864831));
#9639=CARTESIAN_POINT('Ctrl Pts',(-2.43672683137172,0.259446717599513,17.2443988922408));
#9640=CARTESIAN_POINT('Ctrl Pts',(-2.42754837478303,0.345650897198139,17.2399073309853));
#9641=CARTESIAN_POINT('Ctrl Pts',(-2.41380320604947,0.431254610299297,17.2354157697298));
#9642=CARTESIAN_POINT('Ctrl Pts',(-2.39560398952621,0.51578268230535,17.2309242084743));
#9643=CARTESIAN_POINT('Ctrl Pts',(-2.37737168473939,0.600464436043839,17.2264244810452));
#9644=CARTESIAN_POINT('Ctrl Pts',(-2.35466927232697,0.684066288710046,17.221924753616));
#9645=CARTESIAN_POINT('Ctrl Pts',(-2.32765907930525,0.76612887984193,17.2174250261868));
#9646=CARTESIAN_POINT('Ctrl Pts',(-2.30057021386121,0.848430494175921,17.2129121924294));
#9647=CARTESIAN_POINT('Ctrl Pts',(-2.26914861576148,0.9291835360433,17.208399358672));
#9648=CARTESIAN_POINT('Ctrl Pts',(-2.23360485339684,1.00794821736143,17.2038865249145));
#9649=CARTESIAN_POINT('Ctrl Pts',(-2.2185714769549,1.04126205432774,17.2019778038287));
#9650=CARTESIAN_POINT('Ctrl Pts',(-2.20280124227922,1.07422051047322,17.2000690827428));
#9651=CARTESIAN_POINT('Ctrl Pts',(-2.18631246248532,1.10679178998643,17.198160361657));
#9652=CARTESIAN_POINT('Ctrl Pts',(-2.14976489501516,1.17898640053239,17.1939296597167));
#9653=CARTESIAN_POINT('Ctrl Pts',(-2.10956882614381,1.24950456864096,17.1896989577765));
#9654=CARTESIAN_POINT('Ctrl Pts',(-2.06590160807849,1.31795326007363,17.1854682558362));
#9655=CARTESIAN_POINT('Ctrl Pts',(-2.02229712779015,1.38630360957091,17.1812436322506));
#9656=CARTESIAN_POINT('Ctrl Pts',(-1.97523165093694,1.45258999872321,17.1770190086649));
#9657=CARTESIAN_POINT('Ctrl Pts',(-1.92492900182796,1.51644274139237,17.1727943850792));
#9658=CARTESIAN_POINT('Ctrl Pts',(-1.87442837144425,1.58054679582369,17.1685531342109));
#9659=CARTESIAN_POINT('Ctrl Pts',(-1.82066524674829,1.64219758258882,17.1643118833426));
#9660=CARTESIAN_POINT('Ctrl Pts',(-1.76391083588777,1.70104932704426,17.1600706324743));
#9661=CARTESIAN_POINT('Ctrl Pts',(-1.70748094820539,1.75956455571421,17.1558536331874));
#9662=CARTESIAN_POINT('Ctrl Pts',(-1.64809421610665,1.81531232708092,17.1516366339004));
#9663=CARTESIAN_POINT('Ctrl Pts',(-1.5860571931162,1.86798630352697,17.1474196346135));
#9664=CARTESIAN_POINT('Ctrl Pts',(-1.52404073675602,1.92064281739751,17.143204033354));
#9665=CARTESIAN_POINT('Ctrl Pts',(-1.45937608854198,1.97022725920215,17.1389884320946));
#9666=CARTESIAN_POINT('Ctrl Pts',(-1.39240456823114,2.01647210949446,17.1347728308352));
#9667=CARTESIAN_POINT('Ctrl Pts',(-1.32543471903273,2.0627158058583,17.1305573347659));
#9668=CARTESIAN_POINT('Ctrl Pts',(-1.2561584954922,2.10561981303298,17.1263418386966));
#9669=CARTESIAN_POINT('Ctrl Pts',(-1.18494682731833,2.14495950228162,17.1221263426273));
#9670=CARTESIAN_POINT('Ctrl Pts',(-1.11298057665956,2.18471604794199,17.1178661777617));
#9671=CARTESIAN_POINT('Ctrl Pts',(-1.03903803618435,2.2208320401469,17.1136060128961));
#9672=CARTESIAN_POINT('Ctrl Pts',(-0.963526554606486,2.2531237934406,17.1093458480305));
#9673=CARTESIAN_POINT('Ctrl Pts',(-0.888698012437882,2.28512349431449,17.1051242128616));
#9674=CARTESIAN_POINT('Ctrl Pts',(-0.812329257027663,2.31336774702246,17.1009025776926));
#9675=CARTESIAN_POINT('Ctrl Pts',(-0.7348340068149,2.3377273648628,17.0966809425236));
#9676=CARTESIAN_POINT('Ctrl Pts',(-0.656277840028052,2.36242046794558,17.0924015128097));
#9677=CARTESIAN_POINT('Ctrl Pts',(-0.576564580054757,2.3831216445284,17.0881220830958));
#9678=CARTESIAN_POINT('Ctrl Pts',(-0.496136095112703,2.39974982552897,17.0838426533819));
#9679=CARTESIAN_POINT('Ctrl Pts',(-0.415707610170649,2.41637800652954,17.079563223668));
#9680=CARTESIAN_POINT('Ctrl Pts',(-0.334564395092556,2.42893318165386,17.0752837939541));
#9681=CARTESIAN_POINT('Ctrl Pts',(-0.25315194338759,2.43738883716962,17.0710043642402));
#9682=CARTESIAN_POINT('Ctrl Pts',(-0.172666495461915,2.44574821227059,17.0667736623));
#9683=CARTESIAN_POINT('Ctrl Pts',(-0.0916151872469946,2.45013243657524,
17.0625429603597));
#9684=CARTESIAN_POINT('Ctrl Pts',(-0.0104244858216357,2.45047782689323,
17.0583122584195));
#9685=CARTESIAN_POINT('Ctrl Pts',(0.0706495669060399,2.45082272098037,17.0540876348338));
#9686=CARTESIAN_POINT('Ctrl Pts',(0.151862153987194,2.44714030358705,17.0498630112481));
#9687=CARTESIAN_POINT('Ctrl Pts',(0.232781277887563,2.43941860423033,17.0456383876624));
#9688=CARTESIAN_POINT('Ctrl Pts',(0.314018883450085,2.43166651379264,17.0413971367941));
#9689=CARTESIAN_POINT('Ctrl Pts',(0.394960238835914,2.41984322854111,17.0371558859258));
#9690=CARTESIAN_POINT('Ctrl Pts',(0.475167796108238,2.40398956227801,17.0329146350575));
#9691=CARTESIAN_POINT('Ctrl Pts',(0.554916724509232,2.38822654768556,17.0286976357706));
#9692=CARTESIAN_POINT('Ctrl Pts',(0.633939762958023,2.3684792097371,17.0244806364836));
#9693=CARTESIAN_POINT('Ctrl Pts',(0.711813384088354,2.34483943079962,17.0202636371967));
#9694=CARTESIAN_POINT('Ctrl Pts',(0.789661188409645,2.32120748896602,17.0160480359372));
#9695=CARTESIAN_POINT('Ctrl Pts',(0.86635988747163,2.29368580369924,17.0118324346778));
#9696=CARTESIAN_POINT('Ctrl Pts',(0.94149976772727,2.26241650395534,17.0076168334184));
#9697=CARTESIAN_POINT('Ctrl Pts',(1.01663777304888,2.2311479844612,17.0034013373491));
#9698=CARTESIAN_POINT('Ctrl Pts',(1.09021660795131,2.19613221609753,16.9991858412798));
#9699=CARTESIAN_POINT('Ctrl Pts',(1.16184658839562,2.15755944414828,16.9949703452105));
#9700=CARTESIAN_POINT('Ctrl Pts',(1.23423558390045,2.11857794229777,16.9907101803449));
#9701=CARTESIAN_POINT('Ctrl Pts',(1.30463374341828,2.07596382114797,16.9864500154793));
#9702=CARTESIAN_POINT('Ctrl Pts',(1.37266608860103,2.02996011271274,16.9821898506137));
#9703=CARTESIAN_POINT('Ctrl Pts',(1.44008313702819,1.98437247008371,16.9779682154447));
#9704=CARTESIAN_POINT('Ctrl Pts',(1.5051766538526,1.93545663745896,16.9737465802758));
#9705=CARTESIAN_POINT('Ctrl Pts',(1.56761403231892,1.88349050851784,16.9695249451068));
#9706=CARTESIAN_POINT('Ctrl Pts',(1.63090618381286,1.83081295884671,16.9652455153929));
#9707=CARTESIAN_POINT('Ctrl Pts',(1.6914685570292,1.77500129807699,16.960966085679));
#9708=CARTESIAN_POINT('Ctrl Pts',(1.7489937598395,1.71638313847535,16.9566866559651));
#9709=CARTESIAN_POINT('Ctrl Pts',(1.80651896264979,1.65776497887372,16.9524072262512));
#9710=CARTESIAN_POINT('Ctrl Pts',(1.86100671849099,1.5963407309012,16.9481277965373));
#9711=CARTESIAN_POINT('Ctrl Pts',(1.91219354027981,1.53247059172833,16.9438483668235));
#9712=CARTESIAN_POINT('Ctrl Pts',(1.96279752275777,1.46932771059958,16.9396176648832));
#9713=CARTESIAN_POINT('Ctrl Pts',(2.01036573076263,1.40355688444311,16.9353869629429));
#9714=CARTESIAN_POINT('Ctrl Pts',(2.05461372784441,1.33548218983006,16.9311562610027));
#9715=CARTESIAN_POINT('Ctrl Pts',(2.09879815272956,1.2675052998219,16.926931637417));
#9716=CARTESIAN_POINT('Ctrl Pts',(2.13967158933008,1.19723150186897,16.9227070138313));
#9717=CARTESIAN_POINT('Ctrl Pts',(2.17699008478969,1.12501752018686,16.9184823902457));
#9718=CARTESIAN_POINT('Ctrl Pts',(2.21445545846413,1.05251931856005,16.9142411393774));
#9719=CARTESIAN_POINT('Ctrl Pts',(2.24833755111596,0.978065998396562,16.9099998885091));
#9720=CARTESIAN_POINT('Ctrl Pts',(2.27843378362012,0.902047528491999,16.9057586376408));
#9721=CARTESIAN_POINT('Ctrl Pts',(2.30835792509426,0.826463734149699,16.9015416383538));
#9722=CARTESIAN_POINT('Ctrl Pts',(2.33453921131335,0.749333077380558,16.8973246390669));
#9723=CARTESIAN_POINT('Ctrl Pts',(2.35682559033526,0.671061388205926,16.8931076397799));
#9724=CARTESIAN_POINT('Ctrl Pts',(2.37910458093497,0.59281564780859,16.8888920385205));
#9725=CARTESIAN_POINT('Ctrl Pts',(2.3974911012804,0.513430073128373,16.8846764372611));
#9726=CARTESIAN_POINT('Ctrl Pts',(2.41188282359256,0.433326084212761,16.8804608360016));
#9727=CARTESIAN_POINT('Ctrl Pts',(2.42627418679409,0.353224094098535,16.8762453399323));
#9728=CARTESIAN_POINT('Ctrl Pts',(2.43667086898234,0.272404183314324,16.872029843863));
#9729=CARTESIAN_POINT('Ctrl Pts',(2.44302184075596,0.191296982697953,16.8678143477938));
#9730=CARTESIAN_POINT('Ctrl Pts',(2.44944010953561,0.109330343248744,16.8635541829282));
#9731=CARTESIAN_POINT('Ctrl Pts',(2.4517263641234,0.027070771010427,16.8592940180626));
#9732=CARTESIAN_POINT('Ctrl Pts',(2.44988191779351,-0.0550348877385224,
16.855033853197));
#9733=CARTESIAN_POINT('Ctrl Pts',(2.44805415296768,-0.136397968154888,16.850812218028));
#9734=CARTESIAN_POINT('Ctrl Pts',(2.44217019982957,-0.217609443387193,16.8465905828591));
#9735=CARTESIAN_POINT('Ctrl Pts',(2.43228362234313,-0.29823921687362,16.8423689476901));
#9736=CARTESIAN_POINT('Ctrl Pts',(2.42226169676907,-0.379972818824617,16.8380895179762));
#9737=CARTESIAN_POINT('Ctrl Pts',(2.40812680941319,-0.461108184029412,16.8338100882623));
#9738=CARTESIAN_POINT('Ctrl Pts',(2.38998797701349,-0.54120949708128,16.8295306585485));
#9739=CARTESIAN_POINT('Ctrl Pts',(2.37184914461379,-0.621310810133148,16.8252512288346));
#9740=CARTESIAN_POINT('Ctrl Pts',(2.34970656253396,-0.700377616281152,16.8209717991207));
#9741=CARTESIAN_POINT('Ctrl Pts',(2.3237204142266,-0.777993371762617,16.8166923694068));
#9742=CARTESIAN_POINT('Ctrl Pts',(2.29803015748355,-0.854725354588237,16.8124616674665));
#9743=CARTESIAN_POINT('Ctrl Pts',(2.26848683192545,-0.930327787757224,16.8082309655263));
#9744=CARTESIAN_POINT('Ctrl Pts',(2.23520891010395,-1.00438607028967,16.804000263586));
#9745=CARTESIAN_POINT('Ctrl Pts',(2.20197879949943,-1.07833795144781,16.7997756400003));
#9746=CARTESIAN_POINT('Ctrl Pts',(2.1650249379799,-1.15074966746851,16.7955510164147));
#9747=CARTESIAN_POINT('Ctrl Pts',(2.12451516514688,-1.22122297843635,16.791326392829));
#9748=CARTESIAN_POINT('Ctrl Pts',(2.08384595386266,-1.29197365841333,16.7870851419607));
#9749=CARTESIAN_POINT('Ctrl Pts',(2.03959293116551,-1.36077019225043,16.7828438910924));
#9750=CARTESIAN_POINT('Ctrl Pts',(1.99197428751592,-1.42723112629855,16.7786026402241));
#9751=CARTESIAN_POINT('Ctrl Pts',(1.94462792849306,-1.49331203501978,16.7743856409372));
#9752=CARTESIAN_POINT('Ctrl Pts',(1.89395460707311,-1.55708359967046,16.7701686416502));
#9753=CARTESIAN_POINT('Ctrl Pts',(1.84021320517683,-1.61819826025516,16.7659516423633));
#9754=CARTESIAN_POINT('Ctrl Pts',(1.78648961973098,-1.67929265999287,16.7617360411038));
#9755=CARTESIAN_POINT('Ctrl Pts',(1.72970028052916,-1.7377315558649,16.7575204398444));
#9756=CARTESIAN_POINT('Ctrl Pts',(1.67014409817489,-1.7932007532152,16.7533048385849));
#9757=CARTESIAN_POINT('Ctrl Pts',(1.61058940190117,-1.84866856646579,16.7490893425156));
#9758=CARTESIAN_POINT('Ctrl Pts',(1.54826834079983,-1.90116651235793,16.7448738464464));
#9759=CARTESIAN_POINT('Ctrl Pts',(1.48351534306502,-1.9504185389015,16.7406583503771));
#9760=CARTESIAN_POINT('Ctrl Pts',(1.41807620106221,-2.00019245627457,16.7363981855115));
#9761=CARTESIAN_POINT('Ctrl Pts',(1.35015365218003,-2.04665094891283,16.7321380206459));
#9762=CARTESIAN_POINT('Ctrl Pts',(1.28012409681095,-2.08955319309271,16.7278778557803));
#9763=CARTESIAN_POINT('Ctrl Pts',(1.21072790132531,-2.13206742166647,16.7236562206113));
#9764=CARTESIAN_POINT('Ctrl Pts',(1.13926310063498,-2.17108929855924,16.7194345854424));
#9765=CARTESIAN_POINT('Ctrl Pts',(1.06612030182457,-2.20643099870299,16.7152129502734));
#9766=CARTESIAN_POINT('Ctrl Pts',(0.991976171870441,-2.24225652973101,16.7109335205595));
#9767=CARTESIAN_POINT('Ctrl Pts',(0.916108207728543,-2.27430016473768,16.7066540908456));
#9768=CARTESIAN_POINT('Ctrl Pts',(0.838941847434141,-2.30241760474154,16.7023746611317));
#9769=CARTESIAN_POINT('Ctrl Pts',(0.761775487139728,-2.33053504474541,16.6980952314178));
#9770=CARTESIAN_POINT('Ctrl Pts',(0.683311218800301,-2.35472620779242,16.6938158017039));
#9771=CARTESIAN_POINT('Ctrl Pts',(0.603985979936841,-2.37490024759772,16.68953637199));
#9772=CARTESIAN_POINT('Ctrl Pts',(0.525563978780598,-2.39484457547628,16.6853056700498));
#9773=CARTESIAN_POINT('Ctrl Pts',(0.446005557894124,-2.4109378551966,16.6810749681095));
#9774=CARTESIAN_POINT('Ctrl Pts',(0.365723438613278,-2.42305522356567,16.6768442661693));
#9775=CARTESIAN_POINT('Ctrl Pts',(0.285556662647657,-2.43515518261058,16.6726196425836));
#9776=CARTESIAN_POINT('Ctrl Pts',(0.204668709249403,-2.44329050640891,16.6683950189979));
#9777=CARTESIAN_POINT('Ctrl Pts',(0.123485271971944,-2.44738669556039,16.6641703954122));
#9778=CARTESIAN_POINT('Ctrl Pts',(0.0419823127471129,-2.45149900650196,
16.6599291445439));
#9779=CARTESIAN_POINT('Ctrl Pts',(-0.0398180013639428,-2.45154020316717,
16.6556878936756));
#9780=CARTESIAN_POINT('Ctrl Pts',(-0.12147682943596,-2.44748720730266,16.6514466428074));
#9781=CARTESIAN_POINT('Ctrl Pts',(-0.202668730232951,-2.44345738657254,
16.6472296435204));
#9782=CARTESIAN_POINT('Ctrl Pts',(-0.283720289483871,-2.43538009094091,
16.6430126442334));
#9783=CARTESIAN_POINT('Ctrl Pts',(-0.364199131769119,-2.42328480423136,
16.6387956449465));
#9784=CARTESIAN_POINT('Ctrl Pts',(-0.444651293557495,-2.41119352737397,
16.634580043687));
#9785=CARTESIAN_POINT('Ctrl Pts',(-0.524530655895172,-2.39508697373133,
16.6303644424276));
#9786=CARTESIAN_POINT('Ctrl Pts',(-0.603411223519619,-2.37504634593318,
16.6261488411682));
#9787=CARTESIAN_POINT('Ctrl Pts',(-0.682289822870212,-2.35500621820045,
16.6219333450989));
#9788=CARTESIAN_POINT('Ctrl Pts',(-0.760169226586095,-2.33103232705722,
16.6177178490296));
#9789=CARTESIAN_POINT('Ctrl Pts',(-0.836636278493729,-2.30325638770593,
16.6135023529603));
#9790=CARTESIAN_POINT('Ctrl Pts',(-0.913913600677536,-2.27518612527708,
16.6092421880947));
#9791=CARTESIAN_POINT('Ctrl Pts',(-0.989748000477595,-2.24323290960423,
16.6049820232291));
#9792=CARTESIAN_POINT('Ctrl Pts',(-1.0637332159051,-2.20758281733216,16.6007218583635));
#9793=CARTESIAN_POINT('Ctrl Pts',(-1.13704929574873,-2.17225515090111,16.5965002231946));
#9794=CARTESIAN_POINT('Ctrl Pts',(-1.20854912200698,-2.13329748850999,16.5922785880256));
#9795=CARTESIAN_POINT('Ctrl Pts',(-1.27786330003798,-2.09093654528683,16.5880569528566));
#9796=CARTESIAN_POINT('Ctrl Pts',(-1.34812639506825,-2.04799567714397,16.5837775231427));
#9797=CARTESIAN_POINT('Ctrl Pts',(-1.41614313681786,-2.00155791913127,16.5794980934288));
#9798=CARTESIAN_POINT('Ctrl Pts',(-1.48156186764036,-1.95190283629949,16.5752186637149));
#9799=CARTESIAN_POINT('Ctrl Pts',(-1.54698059846286,-1.90224775346771,16.570939234001));
#9800=CARTESIAN_POINT('Ctrl Pts',(-1.60980098518759,-1.84937571182599,16.5666598042871));
#9801=CARTESIAN_POINT('Ctrl Pts',(-1.6697100849671,-1.79360488462737,16.5623803745733));
#9802=CARTESIAN_POINT('Ctrl Pts',(-1.73069629536528,-1.73683134915223,16.5580240046415));
#9803=CARTESIAN_POINT('Ctrl Pts',(-1.78892059448119,-1.67681583650999,16.5536676347098));
#9804=CARTESIAN_POINT('Ctrl Pts',(-1.84401397873806,-1.61386576152375,16.5493112647781));
#9805=CARTESIAN_POINT('Ctrl Pts',(-1.89663132731389,-1.5537448217212,16.5451506811016));
#9806=CARTESIAN_POINT('Ctrl Pts',(-1.9463927235685,-1.49094779758312,16.5409900974251));
#9807=CARTESIAN_POINT('Ctrl Pts',(-1.99301105788362,-1.4257830035295,16.5368295137486));
#9808=CARTESIAN_POINT('Ctrl Pts',(-2.03958588784661,-1.360679021433,16.5326728127397));
#9809=CARTESIAN_POINT('Ctrl Pts',(-2.08302319534392,-1.2932120399579,16.5285161117308));
#9810=CARTESIAN_POINT('Ctrl Pts',(-2.1230755050836,-1.22372409051796,16.524359410722));
#9811=CARTESIAN_POINT('Ctrl Pts',(-2.16310357207443,-1.15427820054769,16.5202052256693));
#9812=CARTESIAN_POINT('Ctrl Pts',(-2.19975046767778,-1.0828141848471,16.5160510406167));
#9813=CARTESIAN_POINT('Ctrl Pts',(-2.23281243012162,-1.0097023828309,16.5118968555641));
#9814=CARTESIAN_POINT('Ctrl Pts',(-2.265865219138,-0.936610866537691,16.5077438231386));
#9815=CARTESIAN_POINT('Ctrl Pts',(-2.29533485359459,-0.861872909497991,
16.5035907907131));
#9816=CARTESIAN_POINT('Ctrl Pts',(-2.32106460665767,-0.785881251666621,
16.4994377582876));
#9817=CARTESIAN_POINT('Ctrl Pts',(-2.34680682649795,-0.709852773774594,
16.495282713603));
#9818=CARTESIAN_POINT('Ctrl Pts',(-2.36880538969035,-0.632569836508239,
16.4911276689184));
#9819=CARTESIAN_POINT('Ctrl Pts',(-2.38695297832093,-0.55444181776344,16.4869726242338));
#9820=CARTESIAN_POINT('Ctrl Pts',(-2.40510579337019,-0.476291298523169,
16.4828163829162));
#9821=CARTESIAN_POINT('Ctrl Pts',(-2.41940533677263,-0.397295685264642,
16.4786601415986));
#9822=CARTESIAN_POINT('Ctrl Pts',(-2.42979556890757,-0.317873785199594,
16.474503900281));
#9823=CARTESIAN_POINT('Ctrl Pts',(-2.4401976646121,-0.238361201189751,16.470342913366));
#9824=CARTESIAN_POINT('Ctrl Pts',(-2.44668150234325,-0.158421837288515,
16.4661819264511));
#9825=CARTESIAN_POINT('Ctrl Pts',(-2.44924304161787,-0.0784778509289605,
16.4620209395362));
#9826=CARTESIAN_POINT('Ctrl Pts',(-2.4501035481908,-0.051621996556521,16.4606231250948));
#9827=CARTESIAN_POINT('Ctrl Pts',(-2.45052185378628,-0.0247656044411454,
16.4592253106535));
#9828=CARTESIAN_POINT('Ctrl Pts',(-2.45049912112546,0.00207541883864715,
16.4578274962121));
#9829=CARTESIAN_POINT('',(-2.45049951066269,-0.00154862581067043,15.6578274962121));
#9830=CARTESIAN_POINT('Ctrl Pts',(-2.45186148920186,0.00207657267883799,
16.4578274962121));
#9831=CARTESIAN_POINT('Ctrl Pts',(-2.45316840210371,0.146834273666068,16.4502931231936));
#9832=CARTESIAN_POINT('Ctrl Pts',(-2.37555074445045,1.1045405278822,16.4003734177029));
#9833=CARTESIAN_POINT('Ctrl Pts',(-1.11386916294639,2.67479374468711,16.3080683797398));
#9834=CARTESIAN_POINT('Ctrl Pts',(1.64579100316184,2.38465889860411,16.180912382323));
#9835=CARTESIAN_POINT('Ctrl Pts',(2.89597065474372,-0.0926285897766665,
16.0537563849064));
#9836=CARTESIAN_POINT('Ctrl Pts',(1.49003463575844,-2.48495933025483,15.9266003874895));
#9837=CARTESIAN_POINT('Ctrl Pts',(-1.28252584789195,-2.59814424893407,15.7994443900729));
#9838=CARTESIAN_POINT('Ctrl Pts',(-2.4072097803276,-0.998919564647339,15.7098534263137));
#9839=CARTESIAN_POINT('Ctrl Pts',(-2.45396548163378,-0.0940230492670492,
15.6626477950268));
#9840=CARTESIAN_POINT('Ctrl Pts',(-2.45328308412766,-0.00155038492700349,
15.6578274962121));
#9841=CARTESIAN_POINT('',(-2.45039354441706,-0.00121703784683746,14.8578275494461));
#9842=CARTESIAN_POINT('Ctrl Pts',(-2.45049951066269,-0.00154862581067043,
15.6578274962121));
#9843=CARTESIAN_POINT('Ctrl Pts',(-2.4505500210209,0.0783774655743783,15.6536564556925));
#9844=CARTESIAN_POINT('Ctrl Pts',(-2.44668598205683,0.158458895275208,15.6494854151729));
#9845=CARTESIAN_POINT('Ctrl Pts',(-2.43888821404384,0.238274063628554,15.6453143746533));
#9846=CARTESIAN_POINT('Ctrl Pts',(-2.43108444750479,0.318150630752134,15.6411401255111));
#9847=CARTESIAN_POINT('Ctrl Pts',(-2.4193408568407,0.397760046304294,15.6369658763688));
#9848=CARTESIAN_POINT('Ctrl Pts',(-2.40369055215463,0.47667806692,15.6327916272266));
#9849=CARTESIAN_POINT('Ctrl Pts',(-2.38808610712666,0.555364836226782,15.628629609772));
#9850=CARTESIAN_POINT('Ctrl Pts',(-2.36859787333269,0.633363780969156,15.6244675923174));
#9851=CARTESIAN_POINT('Ctrl Pts',(-2.34531045813541,0.71025988550718,15.6203055748628));
#9852=CARTESIAN_POINT('Ctrl Pts',(-2.32203341019351,0.787121756896235,15.6161454102844));
#9853=CARTESIAN_POINT('Ctrl Pts',(-2.2949606750716,0.86288130469108,15.611985245706));
#9854=CARTESIAN_POINT('Ctrl Pts',(-2.26422727925668,0.937136637780155,15.6078250811276));
#9855=CARTESIAN_POINT('Ctrl Pts',(-2.23349754837517,1.01138311597885,15.6036654126456));
#9856=CARTESIAN_POINT('Ctrl Pts',(-2.19910820756072,1.08412529377227,15.5995057441636));
#9857=CARTESIAN_POINT('Ctrl Pts',(-2.16124259240274,1.15498082528857,15.5953460756816));
#9858=CARTESIAN_POINT('Ctrl Pts',(-2.12315117743551,1.22625888171129,15.5911616023114));
#9859=CARTESIAN_POINT('Ctrl Pts',(-2.08154210565964,1.29562727592304,15.5869771289412));
#9860=CARTESIAN_POINT('Ctrl Pts',(-2.03664817295185,1.36272318157867,15.582792655571));
#9861=CARTESIAN_POINT('Ctrl Pts',(-1.99196174743556,1.42950895884714,15.5786275235297));
#9862=CARTESIAN_POINT('Ctrl Pts',(-1.94402109266039,1.49404285456839,15.5744623914884));
#9863=CARTESIAN_POINT('Ctrl Pts',(-1.89309724305004,1.55599906116821,15.5702972594471));
#9864=CARTESIAN_POINT('Ctrl Pts',(-1.8418186862252,1.61838682024552,15.5661031154125));
#9865=CARTESIAN_POINT('Ctrl Pts',(-1.78751554941219,1.6781604800788,15.5619089713778));
#9866=CARTESIAN_POINT('Ctrl Pts',(-1.73050189298285,1.73502548926025,15.5577148273432));
#9867=CARTESIAN_POINT('Ctrl Pts',(-1.67348823655352,1.79189049844169,15.5535206833086));
#9868=CARTESIAN_POINT('Ctrl Pts',(-1.61376446905625,1.8458465818398,15.549326539274));
#9869=CARTESIAN_POINT('Ctrl Pts',(-1.55167630420393,1.89664200548549,15.5451323952393));
#9870=CARTESIAN_POINT('Ctrl Pts',(-1.48904695305643,1.94788018319229,15.5409016932991));
#9871=CARTESIAN_POINT('Ctrl Pts',(-1.42375917604961,1.99610924247822,15.5366709913588));
#9872=CARTESIAN_POINT('Ctrl Pts',(-1.35613416485738,2.04104149318591,15.5324402894186));
#9873=CARTESIAN_POINT('Ctrl Pts',(-1.28860631219869,2.0859091886128,15.5282156658329));
#9874=CARTESIAN_POINT('Ctrl Pts',(-1.21874827851875,2.1274892274372,15.5239910422472));
#9875=CARTESIAN_POINT('Ctrl Pts',(-1.14691430973519,2.16553407179953,15.5197664186615));
#9876=CARTESIAN_POINT('Ctrl Pts',(-1.07479761666251,2.20372865314228,15.5155251677933));
#9877=CARTESIAN_POINT('Ctrl Pts',(-1.00068976864277,2.2383598521934,15.511283916925));
#9878=CARTESIAN_POINT('Ctrl Pts',(-0.924978671719191,2.26922116746354,15.5070426660567));
#9879=CARTESIAN_POINT('Ctrl Pts',(-0.849700492791331,2.29990601694076,15.5028256667697));
#9880=CARTESIAN_POINT('Ctrl Pts',(-0.772837785029555,2.3268638009232,15.4986086674828));
#9881=CARTESIAN_POINT('Ctrl Pts',(-0.694794824440917,2.34993838258158,15.4943916681958));
#9882=CARTESIAN_POINT('Ctrl Pts',(-0.616777736800977,2.37300531451136,15.4901760669364));
#9883=CARTESIAN_POINT('Ctrl Pts',(-0.537581618971362,2.39219146885349,15.485960465677));
#9884=CARTESIAN_POINT('Ctrl Pts',(-0.457626837639022,2.40739027319471,15.4817448644175));
#9885=CARTESIAN_POINT('Ctrl Pts',(-0.377674051385011,2.4225886982865,15.4775293683482));
#9886=CARTESIAN_POINT('Ctrl Pts',(-0.296963096348684,2.43379988541402,15.473313872279));
#9887=CARTESIAN_POINT('Ctrl Pts',(-0.215924066860775,2.44096846504626,15.4690983762097));
#9888=CARTESIAN_POINT('Ctrl Pts',(-0.134026320903873,2.44821300532893,15.4648382113441));
#9889=CARTESIAN_POINT('Ctrl Pts',(-0.0517939874893621,2.45132869563443,
15.4605780464785));
#9890=CARTESIAN_POINT('Ctrl Pts',(0.0303260965828464,2.45031234291999,15.4563178816129));
#9891=CARTESIAN_POINT('Ctrl Pts',(0.11170347185729,2.44930518228214,15.452096246444));
#9892=CARTESIAN_POINT('Ctrl Pts',(0.192970154550172,2.44424051071898,15.447874611275));
#9893=CARTESIAN_POINT('Ctrl Pts',(0.27369552980105,2.43516755213413,15.443652976106));
#9894=CARTESIAN_POINT('Ctrl Pts',(0.355526042312747,2.42597038397371,15.4393735463921));
#9895=CARTESIAN_POINT('Ctrl Pts',(0.436799825927911,2.41265443022054,15.4350941166783));
#9896=CARTESIAN_POINT('Ctrl Pts',(0.517079988014912,2.39532430706042,15.4308146869644));
#9897=CARTESIAN_POINT('Ctrl Pts',(0.5973601501019,2.37799418390031,15.4265352572505));
#9898=CARTESIAN_POINT('Ctrl Pts',(0.676646233962757,2.35665008210104,15.4222558275366));
#9899=CARTESIAN_POINT('Ctrl Pts',(0.754520101635884,2.33144797630729,15.4179763978227));
#9900=CARTESIAN_POINT('Ctrl Pts',(0.831507257655783,2.30653283456915,15.4137456958824));
#9901=CARTESIAN_POINT('Ctrl Pts',(0.907403777978826,2.27775342892995,15.4095149939422));
#9902=CARTESIAN_POINT('Ctrl Pts',(0.981793887963674,2.24522404484657,15.4052842920019));
#9903=CARTESIAN_POINT('Ctrl Pts',(1.05607711982931,2.21274139653747,15.4010596684163));
#9904=CARTESIAN_POINT('Ctrl Pts',(1.12885781728258,2.17651965477312,15.3968350448306));
#9905=CARTESIAN_POINT('Ctrl Pts',(1.19973606806946,2.13672263454414,15.3926104212449));
#9906=CARTESIAN_POINT('Ctrl Pts',(1.27089328162873,2.09676898111705,15.3883691703766));
#9907=CARTESIAN_POINT('Ctrl Pts',(1.34013258959538,2.05321199180259,15.3841279195084));
#9908=CARTESIAN_POINT('Ctrl Pts',(1.4070703573616,2.00626599917217,15.3798866686401));
#9909=CARTESIAN_POINT('Ctrl Pts',(1.47362537325352,1.95958844493266,15.3756696693531));
#9910=CARTESIAN_POINT('Ctrl Pts',(1.53790471347362,1.90956080874419,15.3714526700662));
#9911=CARTESIAN_POINT('Ctrl Pts',(1.59955822498862,1.85643845437204,15.3672356707792));
#9912=CARTESIAN_POINT('Ctrl Pts',(1.66119129701568,1.80333371122259,15.3630200695198));
#9913=CARTESIAN_POINT('Ctrl Pts',(1.72019991700277,1.7471365906119,15.3588044682603));
#9914=CARTESIAN_POINT('Ctrl Pts',(1.77626689188751,1.6881428194274,15.3545888670009));
#9915=CARTESIAN_POINT('Ctrl Pts',(1.8323324677565,1.62915052028977,15.3503733709316));
#9916=CARTESIAN_POINT('Ctrl Pts',(1.8854562248713,1.5673620471762,15.3461578748623));
#9917=CARTESIAN_POINT('Ctrl Pts',(1.93535875271642,1.50310902741084,15.341942378793));
#9918=CARTESIAN_POINT('Ctrl Pts',(1.98579006431885,1.43817516131008,15.3376822139274));
#9919=CARTESIAN_POINT('Ctrl Pts',(2.03293116385478,1.37072457999735,15.3334220490618));
#9920=CARTESIAN_POINT('Ctrl Pts',(2.07653744401255,1.30113123612256,15.3291618841962));
#9921=CARTESIAN_POINT('Ctrl Pts',(2.11974934113627,1.23216730695611,15.3249402490273));
#9922=CARTESIAN_POINT('Ctrl Pts',(2.15948992514981,1.16109965892827,15.3207186138583));
#9923=CARTESIAN_POINT('Ctrl Pts',(2.19556744143376,1.08831698512703,15.3164969786893));
#9924=CARTESIAN_POINT('Ctrl Pts',(2.23213886198761,1.01453791032408,15.3122175489754));
#9925=CARTESIAN_POINT('Ctrl Pts',(2.26494596294879,0.938996950216263,15.3079381192615));
#9926=CARTESIAN_POINT('Ctrl Pts',(2.29384016231614,0.862118066012683,15.3036586895476));
#9927=CARTESIAN_POINT('Ctrl Pts',(2.3227343616835,0.785239181809103,15.2993792598337));
#9928=CARTESIAN_POINT('Ctrl Pts',(2.34771557258479,0.707022860765963,15.2950998301198));
#9929=CARTESIAN_POINT('Ctrl Pts',(2.36868854703008,0.627905102040517,15.2908204004059));
#9930=CARTESIAN_POINT('Ctrl Pts',(2.38942271247052,0.549688218547485,15.2865896984657));
#9931=CARTESIAN_POINT('Ctrl Pts',(2.40631748587874,0.470296136967602,15.2823589965254));
#9932=CARTESIAN_POINT('Ctrl Pts',(2.41924384829611,0.390140298458688,15.2781282945852));
#9933=CARTESIAN_POINT('Ctrl Pts',(2.43215163908745,0.310099621834392,15.2739036709995));
#9934=CARTESIAN_POINT('Ctrl Pts',(2.44110226899643,0.229297822829221,15.2696790474138));
#9935=CARTESIAN_POINT('Ctrl Pts',(2.44601694947692,0.148159822055846,15.2654544238281));
#9936=CARTESIAN_POINT('Ctrl Pts',(2.45095097316745,0.066702478164027,15.2612131729599));
#9937=CARTESIAN_POINT('Ctrl Pts',(2.45181708829446,-0.0150932609085146,
15.2569719220916));
#9938=CARTESIAN_POINT('Ctrl Pts',(2.44858779225843,-0.096788809285944,15.2527306712233));
#9939=CARTESIAN_POINT('Ctrl Pts',(2.44537696142003,-0.178017220420699,15.2485136719363));
#9940=CARTESIAN_POINT('Ctrl Pts',(2.4381174462129,-0.259146114168169,15.2442966726494));
#9941=CARTESIAN_POINT('Ctrl Pts',(2.4268343686435,-0.339742839763735,15.2400796733624));
#9942=CARTESIAN_POINT('Ctrl Pts',(2.41555503166114,-0.42031284578157,15.235864072103));
#9943=CARTESIAN_POINT('Ctrl Pts',(2.40025484563934,-0.500350573794205,15.2316484708435));
#9944=CARTESIAN_POINT('Ctrl Pts',(2.38101071310185,-0.579429231308029,15.2274328695841));
#9945=CARTESIAN_POINT('Ctrl Pts',(2.36176706075519,-0.658505915605031,15.2232173735148));
#9946=CARTESIAN_POINT('Ctrl Pts',(2.33857976857895,-0.736623125368398,15.2190018774455));
#9947=CARTESIAN_POINT('Ctrl Pts',(2.31157637857764,-0.813366397143319,15.2147863813762));
#9948=CARTESIAN_POINT('Ctrl Pts',(2.2842868516882,-0.890922866111946,15.2105262165106));
#9949=CARTESIAN_POINT('Ctrl Pts',(2.25310001776086,-0.96707564396322,15.206266051645));
#9950=CARTESIAN_POINT('Ctrl Pts',(2.218197847003,-1.04141661286502,15.2020058867794));
#9951=CARTESIAN_POINT('Ctrl Pts',(2.18361133774962,-1.11508522868453,15.1977842516105));
#9952=CARTESIAN_POINT('Ctrl Pts',(2.1453767009966,-1.18697429020506,15.1935626164415));
#9953=CARTESIAN_POINT('Ctrl Pts',(2.10371691515927,-1.25671213524529,15.1893409812725));
#9954=CARTESIAN_POINT('Ctrl Pts',(2.0614868033065,-1.32740469732228,15.1850615515586));
#9955=CARTESIAN_POINT('Ctrl Pts',(2.01573732590765,-1.39588628495882,15.1807821218447));
#9956=CARTESIAN_POINT('Ctrl Pts',(1.96674448748316,-1.4618024390986,15.1765026921308));
#9957=CARTESIAN_POINT('Ctrl Pts',(1.91775164905867,-1.52771859323837,15.1722232624169));
#9958=CARTESIAN_POINT('Ctrl Pts',(1.8655158122392,-1.59106897703662,15.1679438327031));
#9959=CARTESIAN_POINT('Ctrl Pts',(1.81035197820612,-1.65153745492047,15.1636644029892));
#9960=CARTESIAN_POINT('Ctrl Pts',(1.75581626777774,-1.71131740781391,15.1594337010489));
#9961=CARTESIAN_POINT('Ctrl Pts',(1.69821380838738,-1.76850562913858,15.1552029991086));
#9962=CARTESIAN_POINT('Ctrl Pts',(1.63782066989113,-1.82277088611744,15.1509722971684));
#9963=CARTESIAN_POINT('Ctrl Pts',(1.57751429971735,-1.87695817885346,15.1467476735827));
#9964=CARTESIAN_POINT('Ctrl Pts',(1.51442555639587,-1.92823053948142,15.142523049997));
#9965=CARTESIAN_POINT('Ctrl Pts',(1.44886903807624,-1.97629166888494,15.1382984264114));
#9966=CARTESIAN_POINT('Ctrl Pts',(1.38305450227046,-2.0245419573852,15.1340571755431));
#9967=CARTESIAN_POINT('Ctrl Pts',(1.31475304428415,-2.06955533231734,15.1298159246748));
#9968=CARTESIAN_POINT('Ctrl Pts',(1.24431851825873,-2.11107121507504,15.1255746738065));
#9969=CARTESIAN_POINT('Ctrl Pts',(1.17428673866117,-2.15234970894942,15.1213576745196));
#9970=CARTESIAN_POINT('Ctrl Pts',(1.10214662337587,-2.19017036109005,15.1171406752326));
#9971=CARTESIAN_POINT('Ctrl Pts',(1.02827552813991,-2.22432005076351,15.1129236759457));
#9972=CARTESIAN_POINT('Ctrl Pts',(0.954428922788017,-2.25845841906779,15.1087080746862));
#9973=CARTESIAN_POINT('Ctrl Pts',(0.878852898870565,-2.28892804667559,15.1044924734268));
#9974=CARTESIAN_POINT('Ctrl Pts',(0.801947921324733,-2.31556251945028,15.1002768721674));
#9975=CARTESIAN_POINT('Ctrl Pts',(0.72504486275666,-2.34219632762611,15.0960613760981));
#9976=CARTESIAN_POINT('Ctrl Pts',(0.646813356299004,-2.36499502006823,15.0918458800287));
#9977=CARTESIAN_POINT('Ctrl Pts',(0.567670917971575,-2.38384143325208,15.0876303839594));
#9978=CARTESIAN_POINT('Ctrl Pts',(0.487689860085084,-2.40288754928875,15.0833702190939));
#9979=CARTESIAN_POINT('Ctrl Pts',(0.406778917865914,-2.41789700011409,15.0791100542283));
#9980=CARTESIAN_POINT('Ctrl Pts',(0.325379740277694,-2.42880181871984,15.0748498893627));
#9981=CARTESIAN_POINT('Ctrl Pts',(0.244716751479458,-2.43960801218648,15.0706282541937));
#9982=CARTESIAN_POINT('Ctrl Pts',(0.163574796900046,-2.44638354323397,15.0664066190248));
#9983=CARTESIAN_POINT('Ctrl Pts',(0.0823870774699844,-2.44911466033462,
15.0621849838558));
#9984=CARTESIAN_POINT('Ctrl Pts',(8.78912479101573E-5,-2.45188316666093,
15.0579055541419));
#9985=CARTESIAN_POINT('Ctrl Pts',(-0.082257827778794,-2.45049569217384,
15.053626124428));
#9986=CARTESIAN_POINT('Ctrl Pts',(-0.164202633374892,-2.44499238141814,
15.0493466947141));
#9987=CARTESIAN_POINT('Ctrl Pts',(-0.246147438970991,-2.43948907066244,
15.0450672650002));
#9988=CARTESIAN_POINT('Ctrl Pts',(-0.327690851599183,-2.42987004615082,
15.0407878352863));
#9989=CARTESIAN_POINT('Ctrl Pts',(-0.408396532527029,-2.41622898795207,
15.0365084055725));
#9990=CARTESIAN_POINT('Ctrl Pts',(-0.488183257328885,-2.40274325381295,
15.0322777036322));
#9991=CARTESIAN_POINT('Ctrl Pts',(-0.567451338534771,-2.38527593323865,
15.0280470016919));
#9992=CARTESIAN_POINT('Ctrl Pts',(-0.645772822204954,-2.36387980068815,
15.0238162997517));
#9993=CARTESIAN_POINT('Ctrl Pts',(-0.723981779453858,-2.34251440849282,
15.019591676166));
#9994=CARTESIAN_POINT('Ctrl Pts',(-0.801246395387222,-2.31723153636678,
15.0153670525803));
#9995=CARTESIAN_POINT('Ctrl Pts',(-0.87714722712885,-2.28813526521929,15.0111424289946));
#9996=CARTESIAN_POINT('Ctrl Pts',(-0.953346789527534,-2.25892447690515,
15.0069011781263));
#9997=CARTESIAN_POINT('Ctrl Pts',(-1.02817134162219,-2.22587028670684,15.002659927258));
#9998=CARTESIAN_POINT('Ctrl Pts',(-1.10121021916515,-2.1891291198114,14.9984186763898));
#9999=CARTESIAN_POINT('Ctrl Pts',(-1.17383145853143,-2.1525980398514,14.9942016771028));
#10000=CARTESIAN_POINT('Ctrl Pts',(-1.24468696936429,-2.11242224432306,
14.9899846778158));
#10001=CARTESIAN_POINT('Ctrl Pts',(-1.3133932639374,-2.0688036118114,14.9857676785289));
#10002=CARTESIAN_POINT('Ctrl Pts',(-1.38207678087082,-2.02519943983061,
14.9815520772695));
#10003=CARTESIAN_POINT('Ctrl Pts',(-1.44861210416253,-1.97815494650574,
14.97733647601));
#10004=CARTESIAN_POINT('Ctrl Pts',(-1.51264250341415,-1.92791672716043,
14.9731208747506));
#10005=CARTESIAN_POINT('Ctrl Pts',(-1.57667130494187,-1.87767976138849,
14.9689053786813));
#10006=CARTESIAN_POINT('Ctrl Pts',(-1.63819494148964,-1.8242495159687,14.964689882612));
#10007=CARTESIAN_POINT('Ctrl Pts',(-1.69688885882355,-1.76791358691552,
14.9604743865427));
#10008=CARTESIAN_POINT('Ctrl Pts',(-1.7562047163974,-1.7109807036493,14.9562142216771));
#10009=CARTESIAN_POINT('Ctrl Pts',(-1.81263016772042,-1.65108051476925,
14.9519540568115));
#10010=CARTESIAN_POINT('Ctrl Pts',(-1.86586895503826,-1.58854754182065,
14.9476938919459));
#10011=CARTESIAN_POINT('Ctrl Pts',(-1.91862624119627,-1.52658012831694,
14.943472256777));
#10012=CARTESIAN_POINT('Ctrl Pts',(-1.9682540353506,-1.46202777234666,14.939250621608));
#10013=CARTESIAN_POINT('Ctrl Pts',(-2.01450623568521,-1.39524724561112,
14.935028986439));
#10014=CARTESIAN_POINT('Ctrl Pts',(-2.06139163258072,-1.32755248777827,
14.9307495567251));
#10015=CARTESIAN_POINT('Ctrl Pts',(-2.10480805075351,-1.25756850989386,
14.9264701270112));
#10016=CARTESIAN_POINT('Ctrl Pts',(-2.14454698933919,-1.18569324047842,
14.9221906972973));
#10017=CARTESIAN_POINT('Ctrl Pts',(-2.18428592792488,-1.11381797106297,
14.9179112675834));
#10018=CARTESIAN_POINT('Ctrl Pts',(-2.22034723029976,-1.04005187962091,
14.9136318378696));
#10019=CARTESIAN_POINT('Ctrl Pts',(-2.25257341972762,-0.964812540723137,
14.9093524081557));
#10020=CARTESIAN_POINT('Ctrl Pts',(-2.28784259062658,-0.882468672303579,
14.9046688901658));
#10021=CARTESIAN_POINT('Ctrl Pts',(-2.31863234322746,-0.798096502575592,
14.899985372176));
#10022=CARTESIAN_POINT('Ctrl Pts',(-2.3447298650929,-0.712174213055641,
14.8953018541861));
#10023=CARTESIAN_POINT('Ctrl Pts',(-2.3707485750078,-0.626511400403514,
14.8906324799602));
#10024=CARTESIAN_POINT('Ctrl Pts',(-2.39210319657218,-0.539308069372384,
14.8859631057343));
#10025=CARTESIAN_POINT('Ctrl Pts',(-2.40862911253215,-0.451061024987314,
14.8812937315084));
#10026=CARTESIAN_POINT('Ctrl Pts',(-2.42506955792523,-0.363270386463663,
14.8766485068705));
#10027=CARTESIAN_POINT('Ctrl Pts',(-2.4367309933493,-0.274447073716981,
14.8720032822326));
#10028=CARTESIAN_POINT('Ctrl Pts',(-2.44349925207793,-0.185099041311885,
14.8673580575947));
#10029=CARTESIAN_POINT('Ctrl Pts',(-2.44812801520219,-0.123994569068216,
14.8641812221087));
#10030=CARTESIAN_POINT('Ctrl Pts',(-2.45046918747776,-0.062645071709354,
14.8610043866226));
#10031=CARTESIAN_POINT('Ctrl Pts',(-2.4504996977374,-0.00121712321269822,
14.8578275511366));
#10032=CARTESIAN_POINT('',(-2.450499106739,0.00209233634422269,14.0578274722887));
#10033=CARTESIAN_POINT('Ctrl Pts',(-2.44705070124995,-0.00121434961548067,
14.8578274962121));
#10034=CARTESIAN_POINT('Ctrl Pts',(-2.44487279928209,0.485573530690027,
14.8326171343877));
#10035=CARTESIAN_POINT('Ctrl Pts',(-2.06824721923167,1.79388671502831,14.765021440091));
#10036=CARTESIAN_POINT('Ctrl Pts',(0.0634192762513089,2.89675751214696,
14.6550404133223));
#10037=CARTESIAN_POINT('Ctrl Pts',(2.46980661816694,1.51501859976684,14.5278844159054));
#10038=CARTESIAN_POINT('Ctrl Pts',(2.61094584679872,-1.25625947712439,14.4007284184888));
#10039=CARTESIAN_POINT('Ctrl Pts',(0.357387405644541,-2.87532612603628,
14.2735724210721));
#10040=CARTESIAN_POINT('Ctrl Pts',(-1.96297980716343,-1.9601448883806,14.1592721136464));
#10041=CARTESIAN_POINT('Ctrl Pts',(-2.44422976160869,-0.567055827848684,
14.0873571386931));
#10042=CARTESIAN_POINT('Ctrl Pts',(-2.44883291810884,0.00209045259362897,
14.0578274962121));
#10043=CARTESIAN_POINT('',(-2.45089304864667,0.000179724721355419,13.2578274962121));
#10044=CARTESIAN_POINT('Ctrl Pts',(-2.450499106739,0.00209233634422269,
14.0578274722887));
#10045=CARTESIAN_POINT('Ctrl Pts',(-2.45041577647118,0.0996869450801318,
14.0527672681355));
#10046=CARTESIAN_POINT('Ctrl Pts',(-2.44449835478114,0.197027745386937,
14.0477070639824));
#10047=CARTESIAN_POINT('Ctrl Pts',(-2.43286032705182,0.293497664483561,
14.0426468598292));
#10048=CARTESIAN_POINT('Ctrl Pts',(-2.42106460921774,0.39127470812082,14.0375180921581));
#10049=CARTESIAN_POINT('Ctrl Pts',(-2.40339228844355,0.488157094540066,
14.032389324487));
#10050=CARTESIAN_POINT('Ctrl Pts',(-2.38001045809076,0.583524180628866,
14.0272605568159));
#10051=CARTESIAN_POINT('Ctrl Pts',(-2.36785304147166,0.63311043541895,14.0245938466234));
#10052=CARTESIAN_POINT('Ctrl Pts',(-2.354152852917,0.682287388051048,14.021927136431));
#10053=CARTESIAN_POINT('Ctrl Pts',(-2.33893842772714,0.730970096037636,
14.0192604262385));
#10054=CARTESIAN_POINT('Ctrl Pts',(-2.31480093488946,0.808204595578842,
14.0150297242983));
#10055=CARTESIAN_POINT('Ctrl Pts',(-2.28678837606431,0.884387484301744,
14.010799022358));
#10056=CARTESIAN_POINT('Ctrl Pts',(-2.25501083799085,0.959101856188274,
14.0065683204177));
#10057=CARTESIAN_POINT('Ctrl Pts',(-2.22327895549577,1.03370888408064,14.0023436968321));
#10058=CARTESIAN_POINT('Ctrl Pts',(-2.18779301727481,1.106851161095,13.9981190732464));
#10059=CARTESIAN_POINT('Ctrl Pts',(-2.14871279704752,1.17812714331018,13.9938944496607));
#10060=CARTESIAN_POINT('Ctrl Pts',(-2.10947876480526,1.24968365368974,13.9896531987924));
#10061=CARTESIAN_POINT('Ctrl Pts',(-2.06662223866416,1.3193586940769,13.9854119479241));
#10062=CARTESIAN_POINT('Ctrl Pts',(-2.0203536715087,1.38676648792121,13.9811706970558));
#10063=CARTESIAN_POINT('Ctrl Pts',(-1.97434966920793,1.45378884226998,13.9769536977689));
#10064=CARTESIAN_POINT('Ctrl Pts',(-1.92497280611315,1.51856942078425,13.9727366984819));
#10065=CARTESIAN_POINT('Ctrl Pts',(-1.87247490186335,1.58075551300378,13.968519699195));
#10066=CARTESIAN_POINT('Ctrl Pts',(-1.81999440181729,1.6429209891733,13.9643040979356));
#10067=CARTESIAN_POINT('Ctrl Pts',(-1.76439521510269,1.70249333203805,13.9600884966761));
#10068=CARTESIAN_POINT('Ctrl Pts',(-1.70596985481517,1.75915238238815,13.9558728954167));
#10069=CARTESIAN_POINT('Ctrl Pts',(-1.64754595239124,1.81581001894866,13.9516573993474));
#10070=CARTESIAN_POINT('Ctrl Pts',(-1.58629635121681,1.86955418454522,13.9474419032781));
#10071=CARTESIAN_POINT('Ctrl Pts',(-1.52254984401921,1.92010213855333,13.9432264072088));
#10072=CARTESIAN_POINT('Ctrl Pts',(-1.45812785766163,1.9711857154687,13.9389662423432));
#10073=CARTESIAN_POINT('Ctrl Pts',(-1.39115610371203,2.01900462760382,13.9347060774777));
#10074=CARTESIAN_POINT('Ctrl Pts',(-1.32200604904638,2.06331050893577,13.9304459126121));
#10075=CARTESIAN_POINT('Ctrl Pts',(-1.2534813999018,2.10721567991493,13.9262242774431));
#10076=CARTESIAN_POINT('Ctrl Pts',(-1.18281813218952,2.14767092939085,13.9220026422742));
#10077=CARTESIAN_POINT('Ctrl Pts',(-1.11040298547042,2.18448059269438,13.9177810071052));
#10078=CARTESIAN_POINT('Ctrl Pts',(-1.03699646922666,2.22179418342283,13.9135015773913));
#10079=CARTESIAN_POINT('Ctrl Pts',(-0.961790195746483,2.25536141382249,
13.9092221476774));
#10080=CARTESIAN_POINT('Ctrl Pts',(-0.88520660629556,2.28502943398344,13.9049427179635));
#10081=CARTESIAN_POINT('Ctrl Pts',(-0.808623016844648,2.31469745414439,
13.9006632882497));
#10082=CARTESIAN_POINT('Ctrl Pts',(-0.730662597778344,2.34046617228505,
13.8963838585358));
#10083=CARTESIAN_POINT('Ctrl Pts',(-0.651760365548603,2.36223594839719,
13.8921044288219));
#10084=CARTESIAN_POINT('Ctrl Pts',(-0.573756554456367,2.38375784271352,
13.8878737268816));
#10085=CARTESIAN_POINT('Ctrl Pts',(-0.494538886439511,2.4014523915938,13.8836430249414));
#10086=CARTESIAN_POINT('Ctrl Pts',(-0.414517480633836,2.4151864334351,13.8794123230011));
#10087=CARTESIAN_POINT('Ctrl Pts',(-0.334611043569813,2.42890074323731,
13.8751876994154));
#10088=CARTESIAN_POINT('Ctrl Pts',(-0.253903616583601,2.43866576896866,
13.8709630758297));
#10089=CARTESIAN_POINT('Ctrl Pts',(-0.172819304132251,2.44439844095009,
13.8667384522441));
#10090=CARTESIAN_POINT('Ctrl Pts',(-0.0914158598692677,2.45015367559426,
13.8624972013758));
#10091=CARTESIAN_POINT('Ctrl Pts',(-0.0096330145461995,2.45184462109823,
13.8582559505075));
#10092=CARTESIAN_POINT('Ctrl Pts',(0.0720909456151732,2.44943935331339,
13.8540146996392));
#10093=CARTESIAN_POINT('Ctrl Pts',(0.153347606074584,2.44704783891148,13.8497977003522));
#10094=CARTESIAN_POINT('Ctrl Pts',(0.234545583426512,2.44060684242901,13.8455807010653));
#10095=CARTESIAN_POINT('Ctrl Pts',(0.315251995562358,2.43013712150034,13.8413637017783));
#10096=CARTESIAN_POINT('Ctrl Pts',(0.395931651756961,2.41967087151321,13.8371481005189));
#10097=CARTESIAN_POINT('Ctrl Pts',(0.476119605525095,2.4051786091569,13.8329324992594));
#10098=CARTESIAN_POINT('Ctrl Pts',(0.555388310547285,2.38673292902818,13.828716898));
#10099=CARTESIAN_POINT('Ctrl Pts',(0.634655037610613,2.3682877091668,13.8245014019307));
#10100=CARTESIAN_POINT('Ctrl Pts',(0.713002108820923,2.34588937412897,13.8202859058614));
#10101=CARTESIAN_POINT('Ctrl Pts',(0.790013795593493,2.31966127975012,13.8160704097921));
#10102=CARTESIAN_POINT('Ctrl Pts',(0.867841523774046,2.2931552637731,13.8118102449265));
#10103=CARTESIAN_POINT('Ctrl Pts',(0.944304934860477,2.26273798332441,13.8075500800609));
#10104=CARTESIAN_POINT('Ctrl Pts',(1.01899409668334,2.2285872836675,13.8032899151953));
#10105=CARTESIAN_POINT('Ctrl Pts',(1.09300775630467,2.19474544907535,13.7990682800263));
#10106=CARTESIAN_POINT('Ctrl Pts',(1.16527874189591,2.15723772646233,13.7948466448574));
#10107=CARTESIAN_POINT('Ctrl Pts',(1.23543316153471,2.1162833348539,13.7906250096884));
#10108=CARTESIAN_POINT('Ctrl Pts',(1.30654800115186,2.07476827413718,13.7863455799745));
#10109=CARTESIAN_POINT('Ctrl Pts',(1.37548747002716,2.02971173012123,13.7820661502606));
#10110=CARTESIAN_POINT('Ctrl Pts',(1.44189434374329,1.98138611872626,13.7777867205467));
#10111=CARTESIAN_POINT('Ctrl Pts',(1.50830121745942,1.93306050733129,13.7735072908328));
#10112=CARTESIAN_POINT('Ctrl Pts',(1.57217515553177,1.88146618777257,13.7692278611189));
#10113=CARTESIAN_POINT('Ctrl Pts',(1.63319686181335,1.8269149571239,13.764948431405));
#10114=CARTESIAN_POINT('Ctrl Pts',(1.69352374376336,1.77298487466464,13.7607177294648));
#10115=CARTESIAN_POINT('Ctrl Pts',(1.75128995276369,1.71596206270458,13.7564870275245));
#10116=CARTESIAN_POINT('Ctrl Pts',(1.80616148883633,1.65611923672317,13.7522563255843));
#10117=CARTESIAN_POINT('Ctrl Pts',(1.86095418960994,1.5963623884165,13.7480317019986));
#10118=CARTESIAN_POINT('Ctrl Pts',(1.91286016552321,1.53379391262591,13.7438070784129));
#10119=CARTESIAN_POINT('Ctrl Pts',(1.96157995994131,1.46872540345588,13.7395824548272));
#10120=CARTESIAN_POINT('Ctrl Pts',(2.01049150583125,1.40340079750728,13.7353412039589));
#10121=CARTESIAN_POINT('Ctrl Pts',(2.05619138227933,1.33555675297525,13.7310999530907));
#10122=CARTESIAN_POINT('Ctrl Pts',(2.0984154554648,1.26554447818575,13.7268587022224));
#10123=CARTESIAN_POINT('Ctrl Pts',(2.14039809031595,1.19593253538064,13.7226417029354));
#10124=CARTESIAN_POINT('Ctrl Pts',(2.17894432091395,1.1241774932692,13.7184247036485));
#10125=CARTESIAN_POINT('Ctrl Pts',(2.21383723189433,1.05065453916997,13.7142077043615));
#10126=CARTESIAN_POINT('Ctrl Pts',(2.24871857511137,0.977155959538485,13.7099921031021));
#10127=CARTESIAN_POINT('Ctrl Pts',(2.27994880462262,0.901891051630504,13.7057765018427));
#10128=CARTESIAN_POINT('Ctrl Pts',(2.30735747623917,0.825258581805236,13.7015609005832));
#10129=CARTESIAN_POINT('Ctrl Pts',(2.33476546393858,0.74862802415801,13.6973454045139));
#10130=CARTESIAN_POINT('Ctrl Pts',(2.35835192774053,0.670630410700876,13.6931299084446));
#10131=CARTESIAN_POINT('Ctrl Pts',(2.37799549961099,0.591682054679605,13.6889144123753));
#10132=CARTESIAN_POINT('Ctrl Pts',(2.39784722129248,0.511897135659761,13.6846542475098));
#10133=CARTESIAN_POINT('Ctrl Pts',(2.4136718605078,0.431141671581015,13.6803940826442));
#10134=CARTESIAN_POINT('Ctrl Pts',(2.42539699986736,0.349856603531223,13.6761339177786));
#10135=CARTESIAN_POINT('Ctrl Pts',(2.43701609495948,0.269306692244254,13.6719122826096));
#10136=CARTESIAN_POINT('Ctrl Pts',(2.44460956275511,0.188237192055988,13.6676906474407));
#10137=CARTESIAN_POINT('Ctrl Pts',(2.44815928378303,0.107081143190291,13.6634690122717));
#10138=CARTESIAN_POINT('Ctrl Pts',(2.45175760079408,0.0248140611052921,
13.6591895825578));
#10139=CARTESIAN_POINT('Ctrl Pts',(2.45120061758858,-0.0575414626753487,
13.6549101528439));
#10140=CARTESIAN_POINT('Ctrl Pts',(2.44652396436944,-0.139537599829008,
13.6506307231301));
#10141=CARTESIAN_POINT('Ctrl Pts',(2.4418473111503,-0.221533736982679,13.6463512934162));
#10142=CARTESIAN_POINT('Ctrl Pts',(2.43305110558808,-0.303170006760965,
13.6420718637023));
#10143=CARTESIAN_POINT('Ctrl Pts',(2.4202246227017,-0.384009147896767,13.6377924339884));
#10144=CARTESIAN_POINT('Ctrl Pts',(2.40754418870418,-0.463927813260419,
13.6335617320481));
#10145=CARTESIAN_POINT('Ctrl Pts',(2.39087714044234,-0.543368013967231,
13.6293310301079));
#10146=CARTESIAN_POINT('Ctrl Pts',(2.37027193396235,-0.621901285631722,
13.6251003281676));
#10147=CARTESIAN_POINT('Ctrl Pts',(2.3496963314944,-0.700321726593826,13.6208757045819));
#10148=CARTESIAN_POINT('Ctrl Pts',(2.32519392503057,-0.777837380340297,
13.6166510809963));
#10149=CARTESIAN_POINT('Ctrl Pts',(2.29686456028875,-0.854027775713154,
13.6124264574106));
#10150=CARTESIAN_POINT('Ctrl Pts',(2.26842369677213,-0.930518041408317,
13.6081852065423));
#10151=CARTESIAN_POINT('Ctrl Pts',(2.23612576042997,-1.00567212575424,13.603943955674));
#10152=CARTESIAN_POINT('Ctrl Pts',(2.20012302712488,-1.07907780790583,13.5997027048057));
#10153=CARTESIAN_POINT('Ctrl Pts',(2.164326158373,-1.1520637544826,13.5954857055188));
#10154=CARTESIAN_POINT('Ctrl Pts',(2.12486695278486,-1.22332081768395,13.5912687062318));
#10155=CARTESIAN_POINT('Ctrl Pts',(2.0819434113731,-1.29246349342646,13.5870517069449));
#10156=CARTESIAN_POINT('Ctrl Pts',(2.03903410005436,-1.36158324685933,13.5828361056854));
#10157=CARTESIAN_POINT('Ctrl Pts',(1.99266297873596,-1.42858961003027,13.578620504426));
#10158=CARTESIAN_POINT('Ctrl Pts',(1.94307303273131,-1.49312338387434,13.5744049031666));
#10159=CARTESIAN_POINT('Ctrl Pts',(1.89348432412387,-1.5576555474341,13.5701894070973));
#10160=CARTESIAN_POINT('Ctrl Pts',(1.84067723475027,-1.61971487623792,13.565973911028));
#10161=CARTESIAN_POINT('Ctrl Pts',(1.78493607301241,-1.67897393227502,13.5617584149587));
#10162=CARTESIAN_POINT('Ctrl Pts',(1.72860425941355,-1.73886091694939,13.5574982500931));
#10163=CARTESIAN_POINT('Ctrl Pts',(1.66927614260114,-1.79588756633691,13.5532380852275));
#10164=CARTESIAN_POINT('Ctrl Pts',(1.60728323947942,-1.84975426424392,13.5489779203619));
#10165=CARTESIAN_POINT('Ctrl Pts',(1.54585101131401,-1.90313378205489,13.5447562851929));
#10166=CARTESIAN_POINT('Ctrl Pts',(1.48180241256323,-1.95341003501791,13.540534650024));
#10167=CARTESIAN_POINT('Ctrl Pts',(1.4154917149567,-2.00033333594402,13.536313014855));
#10168=CARTESIAN_POINT('Ctrl Pts',(1.34827321825363,-2.0478990208553,13.5320335851411));
#10169=CARTESIAN_POINT('Ctrl Pts',(1.2787306347668,-2.09201898923083,13.5277541554272));
#10170=CARTESIAN_POINT('Ctrl Pts',(1.2072597701414,-2.13248073787271,13.5234747257133));
#10171=CARTESIAN_POINT('Ctrl Pts',(1.135788905516,-2.1729424865146,13.5191952959994));
#10172=CARTESIAN_POINT('Ctrl Pts',(1.06239022765311,-2.20974585407236,13.5149158662855));
#10173=CARTESIAN_POINT('Ctrl Pts',(0.987479701805409,-2.24272916075979,
13.5106364365716));
#10174=CARTESIAN_POINT('Ctrl Pts',(0.913422145486526,-2.27533690266182,
13.5064057346314));
#10175=CARTESIAN_POINT('Ctrl Pts',(0.837608461737434,-2.3043338221964,13.5021750326911));
#10176=CARTESIAN_POINT('Ctrl Pts',(0.760425119891014,-2.32952868345482,
13.4979443307509));
#10177=CARTESIAN_POINT('Ctrl Pts',(0.683352669269241,-2.35468734663017,
13.4937197071652));
#10178=CARTESIAN_POINT('Ctrl Pts',(0.604914907103674,-2.37605465728748,
13.4894950835795));
#10179=CARTESIAN_POINT('Ctrl Pts',(0.525519405338082,-2.39348691339917,
13.4852704599938));
#10180=CARTESIAN_POINT('Ctrl Pts',(0.445811418585593,-2.41098777942203,
13.4810292091255));
#10181=CARTESIAN_POINT('Ctrl Pts',(0.365138571434227,-2.42452235803849,
13.4767879582572));
#10182=CARTESIAN_POINT('Ctrl Pts',(0.283929885616584,-2.43399549507672,
13.4725467073889));
#10183=CARTESIAN_POINT('Ctrl Pts',(0.203185553149003,-2.44341446447419,
13.468329708102));
#10184=CARTESIAN_POINT('Ctrl Pts',(0.121911959836887,-2.44881825868415,
13.464112708815));
#10185=CARTESIAN_POINT('Ctrl Pts',(0.0405404212323698,-2.45016463206992,
13.4598957095281));
#10186=CARTESIAN_POINT('Ctrl Pts',(-0.0408041409269525,-2.45151055910344,
13.4556801082686));
#10187=CARTESIAN_POINT('Ctrl Pts',(-0.122246119268457,-2.4488017288125,
13.4514645070092));
#10188=CARTESIAN_POINT('Ctrl Pts',(-0.203351959348853,-2.44204795829832,
13.4472489057498));
#10189=CARTESIAN_POINT('Ctrl Pts',(-0.284455775629077,-2.43529435630815,
13.4430334096805));
#10190=CARTESIAN_POINT('Ctrl Pts',(-0.365223006958241,-2.42449605444568,
13.4388179136112));
#10191=CARTESIAN_POINT('Ctrl Pts',(-0.44522442942863,-2.40971480832068,
13.4346024175419));
#10192=CARTESIAN_POINT('Ctrl Pts',(-0.526073573539391,-2.39477693520299,
13.4303422526763));
#10193=CARTESIAN_POINT('Ctrl Pts',(-0.606140103294735,-2.37577127820813,
13.4260820878107));
#10194=CARTESIAN_POINT('Ctrl Pts',(-0.684992626946587,-2.3528143469107,
13.4218219229451));
#10195=CARTESIAN_POINT('Ctrl Pts',(-0.763131994204292,-2.33006504222541,
13.4176002877761));
#10196=CARTESIAN_POINT('Ctrl Pts',(-0.840078802224773,-2.30343585993608,
13.4133786526072));
#10197=CARTESIAN_POINT('Ctrl Pts',(-0.915431317714254,-2.27308947306259,
13.4091570174382));
#10198=CARTESIAN_POINT('Ctrl Pts',(-0.991815415556953,-2.24232764156884,
13.4048775877243));
#10199=CARTESIAN_POINT('Ctrl Pts',(-1.06656078941694,-2.20774626487551,
13.4005981580104));
#10200=CARTESIAN_POINT('Ctrl Pts',(-1.13927448176671,-2.16956306780771,
13.3963187282965));
#10201=CARTESIAN_POINT('Ctrl Pts',(-1.21198817411647,-2.13137987073991,
13.3920392985826));
#10202=CARTESIAN_POINT('Ctrl Pts',(-1.2826697959722,-2.08959515933193,13.3877598688687));
#10203=CARTESIAN_POINT('Ctrl Pts',(-1.3509582053218,-2.04447112414769,13.3834804391548));
#10204=CARTESIAN_POINT('Ctrl Pts',(-1.4183296521778,-1.99995300508036,13.3792584727291));
#10205=CARTESIAN_POINT('Ctrl Pts',(-1.48362752635937,-1.95201570998192,
13.3750365063033));
#10206=CARTESIAN_POINT('Ctrl Pts',(-1.54648268776746,-1.90087915092873,
13.3708145398775));
#10207=CARTESIAN_POINT('Ctrl Pts',(-1.60924745713495,-1.84981613138795,
13.3665986450639));
#10208=CARTESIAN_POINT('Ctrl Pts',(-1.66957613039138,-1.79556327676153,
13.3623827502502));
#10209=CARTESIAN_POINT('Ctrl Pts',(-1.72712802140429,-1.73838403342877,
13.3581668554366));
#10210=CARTESIAN_POINT('Ctrl Pts',(-1.78461321438406,-1.68127105626034,
13.3539558465075));
#10211=CARTESIAN_POINT('Ctrl Pts',(-1.83932769036507,-1.6212387574476,13.3497448375783));
#10212=CARTESIAN_POINT('Ctrl Pts',(-1.89096455202603,-1.55859016838327,
13.3455338286492));
#10213=CARTESIAN_POINT('Ctrl Pts',(-1.94256868566732,-1.49598128669443,
13.3413254887045));
#10214=CARTESIAN_POINT('Ctrl Pts',(-1.99109878021877,-1.43075976556846,
13.3371171487599));
#10215=CARTESIAN_POINT('Ctrl Pts',(-2.03628630091438,-1.36326385953286,
13.3329088088152));
#10216=CARTESIAN_POINT('Ctrl Pts',(-2.08145918883159,-1.29578981025374,
13.3287018316297));
#10217=CARTESIAN_POINT('Ctrl Pts',(-2.12329139246497,-1.22604322647744,
13.3244948544441));
#10218=CARTESIAN_POINT('Ctrl Pts',(-2.16155690934293,-1.15439247124704,
13.3202878772586));
#10219=CARTESIAN_POINT('Ctrl Pts',(-2.19982189664581,-1.08274270762626,
13.3160809582955));
#10220=CARTESIAN_POINT('Ctrl Pts',(-2.23452007640637,-1.00918923771928,
13.3118740393323));
#10221=CARTESIAN_POINT('Ctrl Pts',(-2.26547144885606,-0.934124919064908,
13.3076671203692));
#10222=CARTESIAN_POINT('Ctrl Pts',(-2.29645345916556,-0.858986296433364,
13.3034560370998));
#10223=CARTESIAN_POINT('Ctrl Pts',(-2.32368107498482,-0.782334270582736,
13.2992449538305));
#10224=CARTESIAN_POINT('Ctrl Pts',(-2.34702275463093,-0.704581038096152,
13.2950338705611));
#10225=CARTESIAN_POINT('Ctrl Pts',(-2.37037558795451,-0.626790651707603,
13.2908207750516));
#10226=CARTESIAN_POINT('Ctrl Pts',(-2.38983867445933,-0.547898464757276,
13.2866076795421));
#10227=CARTESIAN_POINT('Ctrl Pts',(-2.4053312616335,-0.46832870060312,13.2823945840326));
#10228=CARTESIAN_POINT('Ctrl Pts',(-2.42085181559001,-0.388615299350151,
13.2781738831616));
#10229=CARTESIAN_POINT('Ctrl Pts',(-2.43238748256562,-0.30822234053528,
13.2739531822907));
#10230=CARTESIAN_POINT('Ctrl Pts',(-2.43990926163131,-0.227580853776741,
13.2697324814198));
#10231=CARTESIAN_POINT('Ctrl Pts',(-2.4469812836525,-0.151761241794422,
13.2657641530172));
#10232=CARTESIAN_POINT('Ctrl Pts',(-2.45050555932682,-0.0757222904314883,
13.2617958246147));
#10233=CARTESIAN_POINT('Ctrl Pts',(-2.45049999341142,0.000179695898497237,
13.2578274962121));
#10234=CARTESIAN_POINT('',(-2.45049902004184,-0.00219152320485761,12.4578274962121));
#10235=CARTESIAN_POINT('Ctrl Pts',(-2.45452289746772,0.000179990899257165,
13.2578274962121));
#10236=CARTESIAN_POINT('Ctrl Pts',(-2.45453302561943,0.00977866883437539,
13.2573264780541));
#10237=CARTESIAN_POINT('Ctrl Pts',(-2.45448160011236,0.0193772351782657,
13.2568254598961));
#10238=CARTESIAN_POINT('Ctrl Pts',(-2.44478267249261,0.840936583347449,
13.2139391092659));
#10239=CARTESIAN_POINT('Ctrl Pts',(-1.53984848482298,2.45440272420173,13.1291684443213));
#10240=CARTESIAN_POINT('Ctrl Pts',(1.22986534347375,2.62348190878122,13.0020124469047));
#10241=CARTESIAN_POINT('Ctrl Pts',(2.87157581782199,0.386365644539962,12.8748564494879));
#10242=CARTESIAN_POINT('Ctrl Pts',(1.87954498804306,-2.20511603474788,12.7477004520711));
#10243=CARTESIAN_POINT('Ctrl Pts',(-0.836359972883942,-2.7741175325747,
12.6205444546545));
#10244=CARTESIAN_POINT('Ctrl Pts',(-2.31723869397904,-1.27307296623665,
12.5239203157511));
#10245=CARTESIAN_POINT('Ctrl Pts',(-2.4513350646012,-0.230535143793987,
12.4696815093198));
#10246=CARTESIAN_POINT('Ctrl Pts',(-2.44936814623945,-0.00220089742423947,
12.4578280353609));
#10247=CARTESIAN_POINT('',(-2.45026621721638,0.000935076449264825,11.6578274533481));
#10248=CARTESIAN_POINT('Ctrl Pts',(-2.45049902004184,-0.00219152320485761,
12.4578274962121));
#10249=CARTESIAN_POINT('Ctrl Pts',(-2.45057110097417,0.078407328605816,
12.4536452785263));
#10250=CARTESIAN_POINT('Ctrl Pts',(-2.4466624732506,0.159090238605734,12.4494630608406));
#10251=CARTESIAN_POINT('Ctrl Pts',(-2.43877499133106,0.239430139410592,
12.4452808431548));
#10252=CARTESIAN_POINT('Ctrl Pts',(-2.43089124206696,0.319732020328914,
12.441100604653));
#10253=CARTESIAN_POINT('Ctrl Pts',(-2.41903242136504,0.399690743454207,
12.4369203661511));
#10254=CARTESIAN_POINT('Ctrl Pts',(-2.40325239789606,0.478882200553359,
12.4327401276493));
#10255=CARTESIAN_POINT('Ctrl Pts',(-2.38747480138559,0.558061478052139,
12.4285605320658));
#10256=CARTESIAN_POINT('Ctrl Pts',(-2.36777729279835,0.636473259442116,
12.4243809364822));
#10257=CARTESIAN_POINT('Ctrl Pts',(-2.34426496445777,0.71370303797574,12.4202013408987));
#10258=CARTESIAN_POINT('Ctrl Pts',(-2.32074874143639,0.790945609174209,
12.4160210529893));
#10259=CARTESIAN_POINT('Ctrl Pts',(-2.29341658455472,0.867005336426674,
12.41184076508));
#10260=CARTESIAN_POINT('Ctrl Pts',(-2.26242315094786,0.941483794897807,
12.4076604771707));
#10261=CARTESIAN_POINT('Ctrl Pts',(-2.23139545641759,1.01604458373585,12.4034755682657));
#10262=CARTESIAN_POINT('Ctrl Pts',(-2.1966985937168,1.08902017892346,12.3992906593607));
#10263=CARTESIAN_POINT('Ctrl Pts',(-2.15853467669386,1.1600337492979,12.3951057504556));
#10264=CARTESIAN_POINT('Ctrl Pts',(-2.12034575527428,1.23109384664386,12.3909180996643));
#10265=CARTESIAN_POINT('Ctrl Pts',(-2.07868550646702,1.30018895778788,12.3867304488729));
#10266=CARTESIAN_POINT('Ctrl Pts',(-2.03379981297172,1.36697058152551,12.3825427980816));
#10267=CARTESIAN_POINT('Ctrl Pts',(-1.98884110883373,1.43386083161799,12.3783483356972));
#10268=CARTESIAN_POINT('Ctrl Pts',(-1.94064677863175,1.49842971071624,12.3741538733129));
#10269=CARTESIAN_POINT('Ctrl Pts',(-1.88950296486554,1.56036175157056,12.3699594109285));
#10270=CARTESIAN_POINT('Ctrl Pts',(-1.87435517587672,1.57870480065947,12.3687170938927));
#10271=CARTESIAN_POINT('Ctrl Pts',(-1.85894889207212,1.59681678924601,12.3674747768568));
#10272=CARTESIAN_POINT('Ctrl Pts',(-1.8432921369087,1.61469017090294,12.366232459821));
#10273=CARTESIAN_POINT('Ctrl Pts',(-1.78997316716356,1.67555784660342,12.3620017578807));
#10274=CARTESIAN_POINT('Ctrl Pts',(-1.73353580191259,1.73389616839639,12.3577710559405));
#10275=CARTESIAN_POINT('Ctrl Pts',(-1.67424937452314,1.789368403071,12.3535403540002));
#10276=CARTESIAN_POINT('Ctrl Pts',(-1.61504812541672,1.84476093940802,12.3493157304146));
#10277=CARTESIAN_POINT('Ctrl Pts',(-1.55300628043559,1.89729525171528,12.3450911068289));
#10278=CARTESIAN_POINT('Ctrl Pts',(-1.48843239794972,1.94666875629462,12.3408664832432));
#10279=CARTESIAN_POINT('Ctrl Pts',(-1.42360436543798,1.9962365852197,12.3366252323749));
#10280=CARTESIAN_POINT('Ctrl Pts',(-1.35622463416943,2.04261831545925,12.3323839815066));
#10281=CARTESIAN_POINT('Ctrl Pts',(-1.28664173093628,2.08554628484081,12.3281427306383));
#10282=CARTESIAN_POINT('Ctrl Pts',(-1.21745670452995,2.12822879099152,12.3239257313514));
#10283=CARTESIAN_POINT('Ctrl Pts',(-1.14609403315411,2.16749667985552,12.3197087320644));
#10284=CARTESIAN_POINT('Ctrl Pts',(-1.07292669755181,2.20312926349785,12.3154917327775));
#10285=CARTESIAN_POINT('Ctrl Pts',(-0.999783618522003,2.23875003415913,
12.311276131518));
#10286=CARTESIAN_POINT('Ctrl Pts',(-0.924837481142166,2.27073768942736,
12.3070605302586));
#10287=CARTESIAN_POINT('Ctrl Pts',(-0.84848531263859,2.29891777239565,12.3028449289992));
#10288=CARTESIAN_POINT('Ctrl Pts',(-0.772135049318726,2.32709715219813,
12.2986294329299));
#10289=CARTESIAN_POINT('Ctrl Pts',(-0.694379261299608,2.3514689885923,12.2944139368606));
#10290=CARTESIAN_POINT('Ctrl Pts',(-0.615633016713481,2.37190772137793,
12.2901984407913));
#10291=CARTESIAN_POINT('Ctrl Pts',(-0.536052350768697,2.3925630297637,12.2859382759257));
#10292=CARTESIAN_POINT('Ctrl Pts',(-0.455460577744214,2.40920124798693,
12.2816781110601));
#10293=CARTESIAN_POINT('Ctrl Pts',(-0.374297886007959,2.42174551564155,
12.2774179461945));
#10294=CARTESIAN_POINT('Ctrl Pts',(-0.293869244241128,2.43417633068524,
12.2731963110256));
#10295=CARTESIAN_POINT('Ctrl Pts',(-0.212880443295602,2.44258696296552,
12.2689746758566));
#10296=CARTESIAN_POINT('Ctrl Pts',(-0.131764318647952,2.44695492691043,
12.2647530406876));
#10297=CARTESIAN_POINT('Ctrl Pts',(-0.0495377073469863,2.45138268865367,
12.2604736109737));
#10298=CARTESIAN_POINT('Ctrl Pts',(0.0328192455460188,2.45165625337551,
12.2561941812598));
#10299=CARTESIAN_POINT('Ctrl Pts',(0.11485837516566,2.44780673331338,12.2519147515459));
#10300=CARTESIAN_POINT('Ctrl Pts',(0.196897504785295,2.44395721325124,12.247635321832));
#10301=CARTESIAN_POINT('Ctrl Pts',(0.278618329220953,2.43598472122157,12.2433558921182));
#10302=CARTESIAN_POINT('Ctrl Pts',(0.35958270914079,2.42397411811409,12.2390764624043));
#10303=CARTESIAN_POINT('Ctrl Pts',(0.439625187255648,2.41210027387136,12.234845760464));
#10304=CARTESIAN_POINT('Ctrl Pts',(0.519229428313152,2.39623519297794,12.2306150585238));
#10305=CARTESIAN_POINT('Ctrl Pts',(0.597966501057326,2.37642300813918,12.2263843565835));
#10306=CARTESIAN_POINT('Ctrl Pts',(0.676590450293147,2.35663928795854,12.2221597329978));
#10307=CARTESIAN_POINT('Ctrl Pts',(0.754349258431024,2.33291983907684,12.2179351094121));
#10308=CARTESIAN_POINT('Ctrl Pts',(0.830821468793549,2.30536026186619,12.2137104858265));
#10309=CARTESIAN_POINT('Ctrl Pts',(0.907594658646335,2.27769221561218,12.2094692349582));
#10310=CARTESIAN_POINT('Ctrl Pts',(0.98307063199569,2.24615381785958,12.2052279840899));
#10311=CARTESIAN_POINT('Ctrl Pts',(1.05683565332237,2.2108931796599,12.2009867332216));
#10312=CARTESIAN_POINT('Ctrl Pts',(1.13017888436362,2.17583416269456,12.1967697339346));
#10313=CARTESIAN_POINT('Ctrl Pts',(1.20183025301668,2.13709556008851,12.1925527346477));
#10314=CARTESIAN_POINT('Ctrl Pts',(1.2714022780472,2.09487147514505,12.1883357353607));
#10315=CARTESIAN_POINT('Ctrl Pts',(1.34095123842937,2.0526613884095,12.1841201341013));
#10316=CARTESIAN_POINT('Ctrl Pts',(1.40842182686337,2.00696835508838,12.1799045328419));
#10317=CARTESIAN_POINT('Ctrl Pts',(1.47345241214861,1.95803172577296,12.1756889315824));
#10318=CARTESIAN_POINT('Ctrl Pts',(1.53848137475285,1.90909631755279,12.1714734355131));
#10319=CARTESIAN_POINT('Ctrl Pts',(1.60107008431499,1.8569177547608,12.1672579394439));
#10320=CARTESIAN_POINT('Ctrl Pts',(1.66088825234819,1.80177702927187,12.1630424433746));
#10321=CARTESIAN_POINT('Ctrl Pts',(1.72134027355505,1.74605201434383,12.158782278509));
#10322=CARTESIAN_POINT('Ctrl Pts',(1.77896232133806,1.68730200332968,12.1545221136434));
#10323=CARTESIAN_POINT('Ctrl Pts',(1.83345145153556,1.62585547477694,12.1502619487778));
#10324=CARTESIAN_POINT('Ctrl Pts',(1.88744777224751,1.56496467967076,12.1460403136088));
#10325=CARTESIAN_POINT('Ctrl Pts',(1.93836737087246,1.50142635194799,12.1418186784399));
#10326=CARTESIAN_POINT('Ctrl Pts',(1.98595700024202,1.43559222733676,12.1375970432709));
#10327=CARTESIAN_POINT('Ctrl Pts',(2.0341981356899,1.36885682795383,12.133317613557));
#10328=CARTESIAN_POINT('Ctrl Pts',(2.07901716722194,1.29976271141695,12.1290381838431));
#10329=CARTESIAN_POINT('Ctrl Pts',(2.1201976109185,1.22870352024216,12.1247587541292));
#10330=CARTESIAN_POINT('Ctrl Pts',(2.16137805461507,1.15764432906738,12.1204793244153));
#10331=CARTESIAN_POINT('Ctrl Pts',(2.19891974441531,1.08462052950482,12.1161998947014));
#10332=CARTESIAN_POINT('Ctrl Pts',(2.23265681392604,1.01004643518486,12.1119204649876));
#10333=CARTESIAN_POINT('Ctrl Pts',(2.26600973592268,0.936321479612382,12.1076897630473));
#10334=CARTESIAN_POINT('Ctrl Pts',(2.29576972894466,0.860804072338048,12.103459061107));
#10335=CARTESIAN_POINT('Ctrl Pts',(2.32174166943275,0.783878734511687,12.0992283591668));
#10336=CARTESIAN_POINT('Ctrl Pts',(2.3476762953887,0.707063917229259,12.0950037355811));
#10337=CARTESIAN_POINT('Ctrl Pts',(2.36983353019139,0.628845623690227,12.0907791119954));
#10338=CARTESIAN_POINT('Ctrl Pts',(2.38806556893495,0.549629955940727,12.0865544884097));
#10339=CARTESIAN_POINT('Ctrl Pts',(2.40636936537588,0.470102510995376,12.0823132375414));
#10340=CARTESIAN_POINT('Ctrl Pts',(2.42071680629526,0.389570256432995,12.0780719866732));
#10341=CARTESIAN_POINT('Ctrl Pts',(2.43100841586246,0.308461232581811,12.0738307358049));
#10342=CARTESIAN_POINT('Ctrl Pts',(2.44124117774198,0.227815992210994,12.0696137365179));
#10343=CARTESIAN_POINT('Ctrl Pts',(2.44746430597294,0.14660102661504,12.0653967372309));
#10344=CARTESIAN_POINT('Ctrl Pts',(2.44963120743725,0.0652472033846067,
12.061179737944));
#10345=CARTESIAN_POINT('Ctrl Pts',(2.45179739052633,-0.0160796492736131,
12.0569641366846));
#10346=CARTESIAN_POINT('Ctrl Pts',(2.44991000487722,-0.0975448036227609,
12.0527485354251));
#10347=CARTESIAN_POINT('Ctrl Pts',(2.44397449488414,-0.178714628264822,
12.0485329341657));
#10348=CARTESIAN_POINT('Ctrl Pts',(2.43803913299736,-0.259882427510101,
12.0443174380964));
#10349=CARTESIAN_POINT('Ctrl Pts',(2.42805588260066,-0.34075444795722,12.0401019420271));
#10350=CARTESIAN_POINT('Ctrl Pts',(2.41408216762724,-0.420900864746285,
12.0358864459578));
#10351=CARTESIAN_POINT('Ctrl Pts',(2.39996038252938,-0.501896539583761,
12.0316262810922));
#10352=CARTESIAN_POINT('Ctrl Pts',(2.38176312807819,-0.582150661691685,
12.0273661162266));
#10353=CARTESIAN_POINT('Ctrl Pts',(2.3596025575257,-0.661230686310136,12.023105951361));
#10354=CARTESIAN_POINT('Ctrl Pts',(2.33764241115569,-0.739595496974737,
12.0188843161921));
#10355=CARTESIAN_POINT('Ctrl Pts',(2.31179055803468,-0.816806935920933,
12.0146626810231));
#10356=CARTESIAN_POINT('Ctrl Pts',(2.28220561160518,-0.892461649796697,
12.0104410458541));
#10357=CARTESIAN_POINT('Ctrl Pts',(2.25221564473989,-0.969152083147433,
12.0061616161402));
#10358=CARTESIAN_POINT('Ctrl Pts',(2.21838980108288,-1.04424239429594,12.0018821864263));
#10359=CARTESIAN_POINT('Ctrl Pts',(2.18094183158227,-1.11733745003672,11.9976027567124));
#10360=CARTESIAN_POINT('Ctrl Pts',(2.14349386208166,-1.1904325057775,11.9933233269985));
#10361=CARTESIAN_POINT('Ctrl Pts',(2.10242406883344,-1.26153191406031,11.9890438972846));
#10362=CARTESIAN_POINT('Ctrl Pts',(2.05799098710902,-1.33027190715959,11.9847644675708));
#10363=CARTESIAN_POINT('Ctrl Pts',(2.01406384315971,-1.39822919156933,11.9805337656305));
#10364=CARTESIAN_POINT('Ctrl Pts',(1.96668442764706,-1.46413614849952,11.9763030636902));
#10365=CARTESIAN_POINT('Ctrl Pts',(1.91607038741404,-1.52762054204406,11.97207236175));
#10366=CARTESIAN_POINT('Ctrl Pts',(1.86552906563004,-1.59101372598326,11.9678477381643));
#10367=CARTESIAN_POINT('Ctrl Pts',(1.81176263630584,-1.65199089856448,11.9636231145786));
#10368=CARTESIAN_POINT('Ctrl Pts',(1.75503250946484,-1.71020792324253,11.9593984909929));
#10369=CARTESIAN_POINT('Ctrl Pts',(1.69807910406844,-1.7686540786117,11.9551572401246));
#10370=CARTESIAN_POINT('Ctrl Pts',(1.63813887967917,-1.82431791414245,11.9509159892564));
#10371=CARTESIAN_POINT('Ctrl Pts',(1.57551785703001,-1.87688404867738,11.9466747383881));
#10372=CARTESIAN_POINT('Ctrl Pts',(1.51325490299575,-1.92914960870573,11.9424577391011));
#10373=CARTESIAN_POINT('Ctrl Pts',(1.44834208503512,-1.9783524950656,11.9382407398142));
#10374=CARTESIAN_POINT('Ctrl Pts',(1.38111643225032,-2.02422025742461,11.9340237405272));
#10375=CARTESIAN_POINT('Ctrl Pts',(1.31391306624008,-2.07007281361697,11.9298081392678));
#10376=CARTESIAN_POINT('Ctrl Pts',(1.24439877190748,-2.11259217957145,11.9255925380083));
#10377=CARTESIAN_POINT('Ctrl Pts',(1.17294107577213,-2.15154815952758,11.9213769367489));
#10378=CARTESIAN_POINT('Ctrl Pts',(1.10148516269089,-2.19050316743138,11.9171614406796));
#10379=CARTESIAN_POINT('Ctrl Pts',(1.02808635306695,-2.22589474447284,11.9129459446103));
#10380=CARTESIAN_POINT('Ctrl Pts',(0.953137115382562,-2.25753845798476,
11.908730448541));
#10381=CARTESIAN_POINT('Ctrl Pts',(0.87739369068565,-2.28951747879367,11.9044702836754));
#10382=CARTESIAN_POINT('Ctrl Pts',(0.800067224637078,-2.31766853265137,
11.9002101188099));
#10383=CARTESIAN_POINT('Ctrl Pts',(0.721582103597065,-2.34185172839111,
11.8959499539443));
#10384=CARTESIAN_POINT('Ctrl Pts',(0.643806816095898,-2.36581620696274,
11.8917283187753));
#10385=CARTESIAN_POINT('Ctrl Pts',(0.564894218405914,-2.38588425469436,
11.8875066836064));
#10386=CARTESIAN_POINT('Ctrl Pts',(0.485269308089031,-2.40197084674789,
11.8832850484374));
#10387=CARTESIAN_POINT('Ctrl Pts',(0.404554325970041,-2.41827766561638,
11.8790056187235));
#10388=CARTESIAN_POINT('Ctrl Pts',(0.323107869493765,-2.4304931170988,11.8747261890096));
#10389=CARTESIAN_POINT('Ctrl Pts',(0.241377877170814,-2.43858298411444,
11.8704467592957));
#10390=CARTESIAN_POINT('Ctrl Pts',(0.159647884847869,-2.44667285113009,
11.8661673295818));
#10391=CARTESIAN_POINT('Ctrl Pts',(0.0776348498557966,-2.45063717540779,
11.861887899868));
#10392=CARTESIAN_POINT('Ctrl Pts',(-0.00421541329485567,-2.45049637426599,
11.8576084701541));
#10393=CARTESIAN_POINT('Ctrl Pts',(-0.0851336875214292,-2.45035717635794,
11.8533777682138));
#10394=CARTESIAN_POINT('Ctrl Pts',(-0.166197234216478,-2.44620538357498,
11.8491470662736));
#10395=CARTESIAN_POINT('Ctrl Pts',(-0.246975256662488,-2.43802245120846,
11.8449163643333));
#10396=CARTESIAN_POINT('Ctrl Pts',(-0.327637223317059,-2.42985127546414,
11.8406917407476));
#10397=CARTESIAN_POINT('Ctrl Pts',(-0.408014021675053,-2.41766050912247,
11.836467117162));
#10398=CARTESIAN_POINT('Ctrl Pts',(-0.487674785863702,-2.40148361502484,
11.8322424935763));
#10399=CARTESIAN_POINT('Ctrl Pts',(-0.567649079059602,-2.38524305187259,
11.828001242708));
#10400=CARTESIAN_POINT('Ctrl Pts',(-0.646901215105861,-2.36498491726102,
11.8237599918397));
#10401=CARTESIAN_POINT('Ctrl Pts',(-0.725000351671659,-2.34079574932884,
11.8195187409714));
#10402=CARTESIAN_POINT('Ctrl Pts',(-0.802652915369833,-2.31674489567981,
11.8153017416845));
#10403=CARTESIAN_POINT('Ctrl Pts',(-0.879165180861883,-2.28880798119376,
11.8110847423975));
#10404=CARTESIAN_POINT('Ctrl Pts',(-0.954125611932698,-2.25712085778632,
11.8068677431105));
#10405=CARTESIAN_POINT('Ctrl Pts',(-1.02906119198066,-2.22544423935353,
11.8026521418511));
#10406=CARTESIAN_POINT('Ctrl Pts',(-1.1024455312305,-2.19002006186729,11.7984365405917));
#10407=CARTESIAN_POINT('Ctrl Pts',(-1.17388610765322,-2.15103269530214,
11.7942209393323));
#10408=CARTESIAN_POINT('Ctrl Pts',(-1.24532490144898,-2.11204630157251,
11.790005443263));
#10409=CARTESIAN_POINT('Ctrl Pts',(-1.31481962114412,-2.06949711927528,
11.7857899471937));
#10410=CARTESIAN_POINT('Ctrl Pts',(-1.38200271650055,-2.02361526520856,
11.7815744511244));
#10411=CARTESIAN_POINT('Ctrl Pts',(-1.44989770624654,-1.97724723177901,
11.7773142862588));
#10412=CARTESIAN_POINT('Ctrl Pts',(-1.51543138132163,-1.92747573776857,
11.7730541213932));
#10413=CARTESIAN_POINT('Ctrl Pts',(-1.57825635937206,-1.87458185046736,
11.7687939565276));
#10414=CARTESIAN_POINT('Ctrl Pts',(-1.64051313703101,-1.82216634498823,
11.7645723213587));
#10415=CARTESIAN_POINT('Ctrl Pts',(-1.7001097143576,-1.76668506359617,11.7603506861897));
#10416=CARTESIAN_POINT('Ctrl Pts',(-1.75674450736484,-1.70844929273405,
11.7561290510207));
#10417=CARTESIAN_POINT('Ctrl Pts',(-1.81415463551072,-1.64941626921013,
11.7518496213068));
#10418=CARTESIAN_POINT('Ctrl Pts',(-1.86852094462973,-1.5875531383464,11.7475701915929));
#10419=CARTESIAN_POINT('Ctrl Pts',(-1.91957214723769,-1.52321798228266,
11.743290761879));
#10420=CARTESIAN_POINT('Ctrl Pts',(-1.97062334984566,-1.45888282621893,
11.7390113321651));
#10421=CARTESIAN_POINT('Ctrl Pts',(-2.01835921401425,-1.39207608219041,
11.7347319024512));
#10422=CARTESIAN_POINT('Ctrl Pts',(-2.06255553650021,-1.3231836262788,11.7304524727373));
#10423=CARTESIAN_POINT('Ctrl Pts',(-2.10727116745882,-1.25348168138612,
11.7261227595613));
#10424=CARTESIAN_POINT('Ctrl Pts',(-2.14852584144248,-1.18139238103366,
11.7217930463853));
#10425=CARTESIAN_POINT('Ctrl Pts',(-2.18606292576863,-1.1072845770532,11.7174633332092));
#10426=CARTESIAN_POINT('Ctrl Pts',(-2.22353816353652,-1.03329887399503,
11.7131407537215));
#10427=CARTESIAN_POINT('Ctrl Pts',(-2.25730779196089,-0.957301663986588,
11.7088181742337));
#10428=CARTESIAN_POINT('Ctrl Pts',(-2.28715895920277,-0.879689800633441,
11.7044955947459));
#10429=CARTESIAN_POINT('Ctrl Pts',(-2.31695826440011,-0.802212776560814,
11.7001805251089));
#10430=CARTESIAN_POINT('Ctrl Pts',(-2.34285250298379,-0.723127087239894,
11.6958654554718));
#10431=CARTESIAN_POINT('Ctrl Pts',(-2.36467584532787,-0.642851768701699,
11.6915503858348));
#10432=CARTESIAN_POINT('Ctrl Pts',(-2.38647684186266,-0.562658647332512,
11.6872397345734));
#10433=CARTESIAN_POINT('Ctrl Pts',(-2.40421511332889,-0.481278736727669,
11.6829290833119));
#10434=CARTESIAN_POINT('Ctrl Pts',(-2.41777398446152,-0.39914810542084,
11.6786184320505));
#10435=CARTESIAN_POINT('Ctrl Pts',(-2.43132082051032,-0.317090374654447,
11.6743116069961));
#10436=CARTESIAN_POINT('Ctrl Pts',(-2.44069556608535,-0.234283678081487,
11.6700047819418));
#10437=CARTESIAN_POINT('Ctrl Pts',(-2.44583244848948,-0.151175010884661,
11.6656979568875));
#10438=CARTESIAN_POINT('Ctrl Pts',(-2.44896156181122,-0.100549667102359,
11.6630744699957));
#10439=CARTESIAN_POINT('Ctrl Pts',(-2.45051917085277,-0.0498124829440769,
11.6604509831039));
#10440=CARTESIAN_POINT('Ctrl Pts',(-2.45049982187577,0.000934337641984426,
11.6578274962121));
#10441=CARTESIAN_POINT('',(-2.4527937259461,0.00178251817473156,10.8578274962121));
#10442=CARTESIAN_POINT('Ctrl Pts',(-2.44679607104562,0.000946051269979937,
11.6578268166126));
#10443=CARTESIAN_POINT('Ctrl Pts',(-2.44799340688633,0.35201353471065,11.6396500361819));
#10444=CARTESIAN_POINT('Ctrl Pts',(-2.21301218228035,1.52018188066365,11.5790879232791));
#10445=CARTESIAN_POINT('Ctrl Pts',(-0.415304589651594,2.8675334673887,11.4761404779038));
#10446=CARTESIAN_POINT('Ctrl Pts',(2.18604951050344,1.90168704744197,11.348984480487));
#10447=CARTESIAN_POINT('Ctrl Pts',(2.7824107934927,-0.808341675923911,11.2218284830704));
#10448=CARTESIAN_POINT('Ctrl Pts',(0.826810820091264,-2.77697856609673,
11.0946724856537));
#10449=CARTESIAN_POINT('Ctrl Pts',(-1.76285248037032,-2.22511816526007,
10.9733388233675));
#10450=CARTESIAN_POINT('Ctrl Pts',(-2.44705219281867,-0.700008467339178,
10.8943904935537));
#10451=CARTESIAN_POINT('Ctrl Pts',(-2.4527937259461,0.00178251817473156,
10.8578274962121));
#10452=CARTESIAN_POINT('',(-2.45241901939193,-0.00192082103873892,10.0578274962121));
#10453=CARTESIAN_POINT('Ctrl Pts',(-2.4527937259461,0.00178251817473156,
10.8578274962121));
#10454=CARTESIAN_POINT('Ctrl Pts',(-2.45370801450179,0.113536548380269,
10.8520051610814));
#10455=CARTESIAN_POINT('Ctrl Pts',(-2.39595452555011,1.03788523585881,10.8037974934788));
#10456=CARTESIAN_POINT('Ctrl Pts',(-1.22083211557998,2.62769766798767,10.7132044934033));
#10457=CARTESIAN_POINT('Ctrl Pts',(1.54828361268476,2.44909043186913,10.5860484959867));
#10458=CARTESIAN_POINT('Ctrl Pts',(2.89735029473491,0.0242354777121154,
10.4588924985699));
#10459=CARTESIAN_POINT('Ctrl Pts',(1.58903593310591,-2.42284768239323,10.3317365011533));
#10460=CARTESIAN_POINT('Ctrl Pts',(-1.17670453748705,-2.64775235251303,
10.2045805037364));
#10461=CARTESIAN_POINT('Ctrl Pts',(-2.3876741667315,-1.06551612567497,10.1132775020894));
#10462=CARTESIAN_POINT('Ctrl Pts',(-2.45349901262548,-0.127352508512948,
10.0643598329146));
#10463=CARTESIAN_POINT('Ctrl Pts',(-2.45241901939193,-0.00192082103873892,
10.0578274962121));
#10464=CARTESIAN_POINT('',(-2.4466576276378,-0.000722135771627219,9.25782749621205));
#10465=CARTESIAN_POINT('Ctrl Pts',(-2.45241901939193,-0.00192082103873892,
10.0578274962121));
#10466=CARTESIAN_POINT('Ctrl Pts',(-2.44649143258849,0.686516099035135,
10.0219745004424));
#10467=CARTESIAN_POINT('Ctrl Pts',(-1.78473046489226,2.19879973224981,9.94373617220041));
#10468=CARTESIAN_POINT('Ctrl Pts',(0.780241169782797,2.79042108036697,9.8231125114863));
#10469=CARTESIAN_POINT('Ctrl Pts',(2.76849932813169,0.854773396237229,9.6959565140695));
#10470=CARTESIAN_POINT('Ctrl Pts',(2.21755549651571,-1.86485219485422,9.56880051665281));
#10471=CARTESIAN_POINT('Ctrl Pts',(-0.367277696167932,-2.87407953659603,
9.44164451923604));
#10472=CARTESIAN_POINT('Ctrl Pts',(-2.19982859173748,-1.5479024331872,9.33798684575582));
#10473=CARTESIAN_POINT('Ctrl Pts',(-2.44761899138352,-0.36555854426161,
9.27671450474781));
#10474=CARTESIAN_POINT('Ctrl Pts',(-2.4466576276378,-0.000722135771627219,
9.25782749621205));
#10475=CARTESIAN_POINT('',(-2.45049898092435,0.0022348352783145,8.45782747312582));
#10476=CARTESIAN_POINT('Ctrl Pts',(-2.4466576276378,-0.000722135771627219,
9.25782749621205));
#10477=CARTESIAN_POINT('Ctrl Pts',(-2.44546154427314,0.453190091476666,
9.23432917227556));
#10478=CARTESIAN_POINT('Ctrl Pts',(-2.10644496581795,1.72751135573376,9.16844551586685));
#10479=CARTESIAN_POINT('Ctrl Pts',(-0.0534527617077329,2.89695855874034,
9.06017652698584));
#10480=CARTESIAN_POINT('Ctrl Pts',(2.40669974372965,1.61338849391436,8.93302052956913));
#10481=CARTESIAN_POINT('Ctrl Pts',(2.65948426593449,-1.14994327165152,8.80586453215237));
#10482=CARTESIAN_POINT('Ctrl Pts',(0.473052830333179,-2.85857431398534,
8.67870853473567));
#10483=CARTESIAN_POINT('Ctrl Pts',(-1.91761415784133,-2.0254181576049,8.56269618942219));
#10484=CARTESIAN_POINT('Ctrl Pts',(-2.4444075610822,-0.599329353249913,
8.48906917658101));
#10485=CARTESIAN_POINT('Ctrl Pts',(-2.44976479135255,0.00223372117810497,
8.45782749621206));
#10486=CARTESIAN_POINT('',(-2.4504999619844,-0.000431641586564807,7.65782749616008));
#10487=CARTESIAN_POINT('Ctrl Pts',(-2.45049898092435,0.0022348352783145,
8.45782747312582));
#10488=CARTESIAN_POINT('Ctrl Pts',(-2.45040110829094,0.109552269706613,
8.45225565092188));
#10489=CARTESIAN_POINT('Ctrl Pts',(-2.44324902256183,0.216554534016528,
8.44668382871794));
#10490=CARTESIAN_POINT('Ctrl Pts',(-2.42919252957169,0.322449847686588,
8.441112006514));
#10491=CARTESIAN_POINT('Ctrl Pts',(-2.41513603658154,0.428345161356646,
8.43554018431006));
#10492=CARTESIAN_POINT('Ctrl Pts',(-2.39417533386648,0.53313388035792,8.42996836210611));
#10493=CARTESIAN_POINT('Ctrl Pts',(-2.36651425439525,0.636050732052167,
8.42439653990217));
#10494=CARTESIAN_POINT('Ctrl Pts',(-2.34551111066831,0.714195817832587,
8.42016583796257));
#10495=CARTESIAN_POINT('Ctrl Pts',(-2.32059364397539,0.791446421958971,
8.41593513602298));
#10496=CARTESIAN_POINT('Ctrl Pts',(-2.29185503851226,0.867381537990035,
8.41170443408338));
#10497=CARTESIAN_POINT('Ctrl Pts',(-2.26315772251752,0.943207556153543,
8.40747981049835));
#10498=CARTESIAN_POINT('Ctrl Pts',(-2.23065033426224,1.01772140859261,8.40325518691333));
#10499=CARTESIAN_POINT('Ctrl Pts',(-2.19447632402472,1.09051543468901,8.3990305633283));
#10500=CARTESIAN_POINT('Ctrl Pts',(-2.15815994003272,1.16359596368433,8.39478931245985));
#10501=CARTESIAN_POINT('Ctrl Pts',(-2.11814813312979,1.23494264121746,8.39054806159139));
#10502=CARTESIAN_POINT('Ctrl Pts',(-2.0746356273981,1.30416151742431,8.38630681072294));
#10503=CARTESIAN_POINT('Ctrl Pts',(-2.03137192729937,1.37298459830708,8.38208981143663));
#10504=CARTESIAN_POINT('Ctrl Pts',(-1.98464770390307,1.43970374779213,8.37787281215031));
#10505=CARTESIAN_POINT('Ctrl Pts',(-1.93470034788306,1.50395638696777,8.373655812864));
#10506=CARTESIAN_POINT('Ctrl Pts',(-1.8847695505042,1.56818772498797,8.3694402116052));
#10507=CARTESIAN_POINT('Ctrl Pts',(-1.83161802763612,1.62995380963631,8.3652246103464));
#10508=CARTESIAN_POINT('Ctrl Pts',(-1.77552514303193,1.68892294568504,8.3610090090876));
#10509=CARTESIAN_POINT('Ctrl Pts',(-1.71943365809002,1.7478906103016,8.35679351301894));
#10510=CARTESIAN_POINT('Ctrl Pts',(-1.66040127865167,1.80406112886576,8.35257801695027));
#10511=CARTESIAN_POINT('Ctrl Pts',(-1.59874512760487,1.85713873120984,8.3483625208816));
#10512=CARTESIAN_POINT('Ctrl Pts',(-1.53643564748553,1.91077876147268,8.34410235601526));
#10513=CARTESIAN_POINT('Ctrl Pts',(-1.47144681660976,1.96125960981008,8.33984219114891));
#10514=CARTESIAN_POINT('Ctrl Pts',(-1.40413978355796,2.00831813172858,8.33558202628256));
#10515=CARTESIAN_POINT('Ctrl Pts',(-1.3374414874301,2.05495104790311,8.33136039111421));
#10516=CARTESIAN_POINT('Ctrl Pts',(-1.26846718406647,2.09822309531934,8.32713875594585));
#10517=CARTESIAN_POINT('Ctrl Pts',(-1.19759540764804,2.13792317204813,8.3229171207775));
#10518=CARTESIAN_POINT('Ctrl Pts',(-1.12575339054113,2.17816674622717,8.31863769106215));
#10519=CARTESIAN_POINT('Ctrl Pts',(-1.05196199707661,2.21473958837252,8.31435826134681));
#10520=CARTESIAN_POINT('Ctrl Pts',(-0.976637160731033,2.2474719367056,8.31007883163147));
#10521=CARTESIAN_POINT('Ctrl Pts',(-0.901312324385457,2.28020428503868,
8.30579940191612));
#10522=CARTESIAN_POINT('Ctrl Pts',(-0.824454527417156,2.30909602823884,
8.30151997220078));
#10523=CARTESIAN_POINT('Ctrl Pts',(-0.746494414108079,2.33403006401062,
8.29724054248544));
#10524=CARTESIAN_POINT('Ctrl Pts',(-0.669421994530714,2.35868018809576,
8.29300984054604));
#10525=CARTESIAN_POINT('Ctrl Pts',(-0.590982356308454,2.37955503273652,
8.28877913860664));
#10526=CARTESIAN_POINT('Ctrl Pts',(-0.511579914801459,2.39650500537172,
8.28454843666723));
#10527=CARTESIAN_POINT('Ctrl Pts',(-0.43229155275501,2.4134306255601,8.28032381308242));
#10528=CARTESIAN_POINT('Ctrl Pts',(-0.352043585654955,2.42644247676516,
8.27609918949761));
#10529=CARTESIAN_POINT('Ctrl Pts',(-0.271256422912863,2.43544045359941,
8.2718745659128));
#10530=CARTESIAN_POINT('Ctrl Pts',(-0.190151297860828,2.44447384469259,
8.26763331504429));
#10531=CARTESIAN_POINT('Ctrl Pts',(-0.108503175727459,2.44946155345117,
8.26339206417579));
#10532=CARTESIAN_POINT('Ctrl Pts',(-0.0267486987495833,2.4503540064887,
8.25915081330729));
#10533=CARTESIAN_POINT('Ctrl Pts',(0.0545383040092322,2.45124135645662,
8.25493381402122));
#10534=CARTESIAN_POINT('Ctrl Pts',(0.13592997892602,2.44808015204624,8.25071681473515));
#10535=CARTESIAN_POINT('Ctrl Pts',(0.216992958930068,2.44087367673437,8.24649981544908));
#10536=CARTESIAN_POINT('Ctrl Pts',(0.298029064782754,2.43366959052674,8.24228421419053));
#10537=CARTESIAN_POINT('Ctrl Pts',(0.378736229251284,2.42242293775493,8.23806861293197));
#10538=CARTESIAN_POINT('Ctrl Pts',(0.45868432623219,2.40718901187026,8.23385301167342));
#10539=CARTESIAN_POINT('Ctrl Pts',(0.538630428301518,2.3919554661114,8.22963751560502));
#10540=CARTESIAN_POINT('Ctrl Pts',(0.617817043904243,2.37273493317166,8.22542201953661));
#10541=CARTESIAN_POINT('Ctrl Pts',(0.695823807958463,2.34963390303217,8.22120652346821));
#10542=CARTESIAN_POINT('Ctrl Pts',(0.774657157626014,2.32628808669499,8.21694635860158));
#10543=CARTESIAN_POINT('Ctrl Pts',(0.852285033563614,2.29897916753237,8.21268619373496));
#10544=CARTESIAN_POINT('Ctrl Pts',(0.928290664938836,2.26786831438411,8.20842602886833));
#10545=CARTESIAN_POINT('Ctrl Pts',(1.00360888769098,2.23703883339655,8.20420439370026));
#10546=CARTESIAN_POINT('Ctrl Pts',(1.07733369203115,2.20247616804331,8.19998275853218));
#10547=CARTESIAN_POINT('Ctrl Pts',(1.14908264953447,2.16438428069944,8.19576112336411));
#10548=CARTESIAN_POINT('Ctrl Pts',(1.22181385642477,2.12577091214812,8.19148169364821));
#10549=CARTESIAN_POINT('Ctrl Pts',(1.29251428319559,2.0835312129496,8.18720226393231));
#10550=CARTESIAN_POINT('Ctrl Pts',(1.3608160100427,2.03792297126546,8.18292283421641));
#10551=CARTESIAN_POINT('Ctrl Pts',(1.42911773688982,1.99231472958133,8.17864340450051));
#10552=CARTESIAN_POINT('Ctrl Pts',(1.49502040911919,1.94333829060359,8.17436397478461));
#10553=CARTESIAN_POINT('Ctrl Pts',(1.55819241617889,1.89129232118215,8.17008454506871));
#10554=CARTESIAN_POINT('Ctrl Pts',(1.62064511451561,1.8398389737391,8.16585384312429));
#10555=CARTESIAN_POINT('Ctrl Pts',(1.68066394662119,1.78519214591384,8.16162314117987));
#10556=CARTESIAN_POINT('Ctrl Pts',(1.73790418615722,1.72761086177912,8.15739243923545));
#10557=CARTESIAN_POINT('Ctrl Pts',(1.79506218721933,1.67011230610558,8.1531678156456));
#10558=CARTESIAN_POINT('Ctrl Pts',(1.84944919910114,1.60968799436721,8.14894319205576));
#10559=CARTESIAN_POINT('Ctrl Pts',(1.900753442809,1.54663719069785,8.14471856846591));
#10560=CARTESIAN_POINT('Ctrl Pts',(1.9522596098063,1.48333823161757,8.14047731759866));
#10561=CARTESIAN_POINT('Ctrl Pts',(2.00065832399826,1.41739236331705,8.13623606673141));
#10562=CARTESIAN_POINT('Ctrl Pts',(2.0456715029086,1.34913985642248,8.13199481586416));
#10563=CARTESIAN_POINT('Ctrl Pts',(2.09042729536166,1.28127761903066,8.12777781657305));
#10564=CARTESIAN_POINT('Ctrl Pts',(2.13183590600191,1.2111354424295,8.12356081728193));
#10565=CARTESIAN_POINT('Ctrl Pts',(2.169665465371,1.13907946095803,8.11934381799081));
#10566=CARTESIAN_POINT('Ctrl Pts',(2.20748248341347,1.06704736762096,8.11512821672722));
#10567=CARTESIAN_POINT('Ctrl Pts',(2.24172259043421,0.993103140796551,8.11091261546363));
#10568=CARTESIAN_POINT('Ctrl Pts',(2.27219939945024,0.917638348772516,8.10669701420004));
#10569=CARTESIAN_POINT('Ctrl Pts',(2.30267544799107,0.842175439790226,8.10248151812661));
#10570=CARTESIAN_POINT('Ctrl Pts',(2.32938821208652,0.765192472675022,8.09826602205318));
#10571=CARTESIAN_POINT('Ctrl Pts',(2.35219963335394,0.687100527470042,8.09405052597975));
#10572=CARTESIAN_POINT('Ctrl Pts',(2.37525277196729,0.608181094248742,8.0897903611191));
#10573=CARTESIAN_POINT('Ctrl Pts',(2.39432124431933,0.528129501321001,8.08553019625845));
#10574=CARTESIAN_POINT('Ctrl Pts',(2.40931490965907,0.447383410616135,8.0812700313978));
#10575=CARTESIAN_POINT('Ctrl Pts',(2.42417296962649,0.36736760189666,8.07704839622479));
#10576=CARTESIAN_POINT('Ctrl Pts',(2.43502963114029,0.286670281452381,8.07282676105177));
#10577=CARTESIAN_POINT('Ctrl Pts',(2.44184932582168,0.20572340650544,8.06860512587876));
#10578=CARTESIAN_POINT('Ctrl Pts',(2.44876238268208,0.123668362207468,8.06432569617429));
#10579=CARTESIAN_POINT('Ctrl Pts',(2.4515270863782,0.0413573732023643,8.06004626646982));
#10580=CARTESIAN_POINT('Ctrl Pts',(2.450160978105,-0.0407606596062904,8.05576683676536));
#10581=CARTESIAN_POINT('Ctrl Pts',(2.44879486983181,-0.122878692414948,
8.05148740706089));
#10582=CARTESIAN_POINT('Ctrl Pts',(2.4432980477765,-0.204803283924434,8.04720797735643));
#10583=CARTESIAN_POINT('Ctrl Pts',(2.43374208045734,-0.286093928301824,
8.04292854765196));
#10584=CARTESIAN_POINT('Ctrl Pts',(2.4242949222569,-0.366458955933194,8.03869784571719));
#10585=CARTESIAN_POINT('Ctrl Pts',(2.41084509740716,-0.446506680336389,
8.03446714378243));
#10586=CARTESIAN_POINT('Ctrl Pts',(2.39342374342146,-0.525807031549031,
8.03023644184766));
#10587=CARTESIAN_POINT('Ctrl Pts',(2.37602741912779,-0.604993449977247,
8.02601181826745));
#10588=CARTESIAN_POINT('Ctrl Pts',(2.35467099705926,-0.683434177406085,
8.02178719468725));
#10589=CARTESIAN_POINT('Ctrl Pts',(2.32943728494609,-0.760705058155243,
8.01756257110704));
#10590=CARTESIAN_POINT('Ctrl Pts',(2.30410425789343,-0.83828006192888,8.01332132023738));
#10591=CARTESIAN_POINT('Ctrl Pts',(2.27486341023255,-0.914675519388884,
8.00908006936772));
#10592=CARTESIAN_POINT('Ctrl Pts',(2.24185026990555,-0.989473404051081,
8.00483881849806));
#10593=CARTESIAN_POINT('Ctrl Pts',(2.20902589961493,-1.06384359236965,8.0006218192165));
#10594=CARTESIAN_POINT('Ctrl Pts',(2.17247244941037,-1.13663399850362,7.99640481993494));
#10595=CARTESIAN_POINT('Ctrl Pts',(2.1323722126194,-1.20745144699431,7.99218782065338));
#10596=CARTESIAN_POINT('Ctrl Pts',(2.09228526993381,-1.27824541795222,7.9879722193993));
#10597=CARTESIAN_POINT('Ctrl Pts',(2.04865410464592,-1.34706732579106,7.98375661814521));
#10598=CARTESIAN_POINT('Ctrl Pts',(2.00170701861795,-1.41354846454433,7.97954101689113));
#10599=CARTESIAN_POINT('Ctrl Pts',(1.95476110404048,-1.48002794442226,7.97532552082713));
#10600=CARTESIAN_POINT('Ctrl Pts',(1.90449970238417,-1.54416639208273,7.97111002476313));
#10601=CARTESIAN_POINT('Ctrl Pts',(1.85119368584312,-1.60562517029803,7.96689452869914));
#10602=CARTESIAN_POINT('Ctrl Pts',(1.79732282089945,-1.66773518630887,7.96263436382715));
#10603=CARTESIAN_POINT('Ctrl Pts',(1.74034273862831,-1.72710802884643,7.95837419895515));
#10604=CARTESIAN_POINT('Ctrl Pts',(1.68057260332271,-1.78343095603982,7.95411403408316));
#10605=CARTESIAN_POINT('Ctrl Pts',(1.62134304002295,-1.83924448840633,7.94989239891933));
#10606=CARTESIAN_POINT('Ctrl Pts',(1.55937408610003,-1.89206279345339,7.9456707637555));
#10607=CARTESIAN_POINT('Ctrl Pts',(1.49500965569569,-1.94162210004332,7.94144912859166));
#10608=CARTESIAN_POINT('Ctrl Pts',(1.42976407049358,-1.99185987796442,7.93716969886559));
#10609=CARTESIAN_POINT('Ctrl Pts',(1.36205733028268,-2.03874846821623,7.93289026913952));
#10610=CARTESIAN_POINT('Ctrl Pts',(1.29227634889301,-2.08205957842031,7.92861083941345));
#10611=CARTESIAN_POINT('Ctrl Pts',(1.22249536750335,-2.12537068862438,7.92433140968737));
#10612=CARTESIAN_POINT('Ctrl Pts',(1.15064060594843,-2.16510413869198,7.9200519799613));
#10613=CARTESIAN_POINT('Ctrl Pts',(1.07712117087272,-2.20108160531539,7.91577255023523));
#10614=CARTESIAN_POINT('Ctrl Pts',(1.00443886592732,-2.23664941398521,7.91154184829876));
#10615=CARTESIAN_POINT('Ctrl Pts',(0.929856244915385,-2.26868015883045,
7.90731114636229));
#10616=CARTESIAN_POINT('Ctrl Pts',(0.853751750611722,-2.2969671739769,7.90308044442583));
#10617=CARTESIAN_POINT('Ctrl Pts',(0.777756597526991,-2.32521354846546,
7.89885582084401));
#10618=CARTESIAN_POINT('Ctrl Pts',(0.700244345910027,-2.34972671501645,
7.89463119726219));
#10619=CARTESIAN_POINT('Ctrl Pts',(0.621616440926069,-2.37034665194153,
7.89040657368037));
#10620=CARTESIAN_POINT('Ctrl Pts',(0.542679071974386,-2.39104774488235,
7.88616532281112));
#10621=CARTESIAN_POINT('Ctrl Pts',(0.462617675088182,-2.40782468790328,
7.88192407194188));
#10622=CARTESIAN_POINT('Ctrl Pts',(0.381857085611667,-2.42056510265024,
7.87768282107263));
#10623=CARTESIAN_POINT('Ctrl Pts',(0.30155828735309,-2.43323266736377,7.87346582178968));
#10624=CARTESIAN_POINT('Ctrl Pts',(0.220568734807663,-2.44190966729512,
7.86924882250672));
#10625=CARTESIAN_POINT('Ctrl Pts',(0.139317688967278,-2.44653649707925,
7.86503182322376));
#10626=CARTESIAN_POINT('Ctrl Pts',(0.0580935796269779,-2.45116179296804,
7.86081622196837));
#10627=CARTESIAN_POINT('Ctrl Pts',(-0.0233913869148578,-2.45173955870471,
7.85660062071298));
#10628=CARTESIAN_POINT('Ctrl Pts',(-0.104703613010195,-2.44826211901884,
7.85238501945759));
#10629=CARTESIAN_POINT('Ctrl Pts',(-0.186013810154746,-2.4447847661041,
7.84816952339237));
#10630=CARTESIAN_POINT('Ctrl Pts',(-0.26715081083336,-2.43725242990822,
7.84395402732716));
#10631=CARTESIAN_POINT('Ctrl Pts',(-0.347683249834275,-2.42570950605893,
7.83973853126194));
#10632=CARTESIAN_POINT('Ctrl Pts',(-0.429069037471752,-2.41404426953105,
7.83547836639165));
#10633=CARTESIAN_POINT('Ctrl Pts',(-0.509836893015987,-2.3982829970036,
7.83121820152137));
#10634=CARTESIAN_POINT('Ctrl Pts',(-0.589551077057614,-2.37852470610255,
7.82695803665108));
#10635=CARTESIAN_POINT('Ctrl Pts',(-0.668544311529168,-2.35894511277586,
7.82273640148625));
#10636=CARTESIAN_POINT('Ctrl Pts',(-0.74650242463531,-2.33544070461839,
7.81851476632141));
#10637=CARTESIAN_POINT('Ctrl Pts',(-0.82301744961681,-2.30815782121289,
7.81429313115658));
#10638=CARTESIAN_POINT('Ctrl Pts',(-0.900579972046674,-2.28050143272446,
7.81001370143357));
#10639=CARTESIAN_POINT('Ctrl Pts',(-0.976659138228902,-2.24896251977144,
7.80573427171055));
#10640=CARTESIAN_POINT('Ctrl Pts',(-1.05085352989834,-2.21374278286801,
7.80145484198754));
#10641=CARTESIAN_POINT('Ctrl Pts',(-1.12504792156778,-2.17852304596457,
7.79717541226452));
#10642=CARTESIAN_POINT('Ctrl Pts',(-1.19735713771531,-2.13962277520911,
7.79289598254151));
#10643=CARTESIAN_POINT('Ctrl Pts',(-1.26740975649506,-2.09728938373824,
7.78861655281849));
#10644=CARTESIAN_POINT('Ctrl Pts',(-1.33666472066548,-2.05543802171072,
7.78438585085046));
#10645=CARTESIAN_POINT('Ctrl Pts',(-1.40397472540247,-2.01007394635283,
7.78015514888243));
#10646=CARTESIAN_POINT('Ctrl Pts',(-1.46896112141315,-1.9614034449283,7.7759244469144));
#10647=CARTESIAN_POINT('Ctrl Pts',(-1.53385414985612,-1.91280286962088,
7.77169982330086));
#10648=CARTESIAN_POINT('Ctrl Pts',(-1.59642983071125,-1.86090557926777,
7.76747519968733));
#10649=CARTESIAN_POINT('Ctrl Pts',(-1.65633627736967,-1.80596245428004,
7.7632505760738));
#10650=CARTESIAN_POINT('Ctrl Pts',(-1.71647850345477,-1.75080308447673,
7.75900932521246));
#10651=CARTESIAN_POINT('Ctrl Pts',(-1.77393003301355,-1.69257409850204,
7.75476807435113));
#10652=CARTESIAN_POINT('Ctrl Pts',(-1.8283663722182,-1.63157183689277,7.75052682348979));
#10653=CARTESIAN_POINT('Ctrl Pts',(-1.88249144348427,-1.5709183872811,7.74630982417498));
#10654=CARTESIAN_POINT('Ctrl Pts',(-1.93363539989396,-1.50752364172897,
7.74209282486016));
#10655=CARTESIAN_POINT('Ctrl Pts',(-1.98151572079982,-1.44171623359909,
7.73787582554535));
#10656=CARTESIAN_POINT('Ctrl Pts',(-2.02938016833126,-1.37593064206547,
7.73366022425811));
#10657=CARTESIAN_POINT('Ctrl Pts',(-2.07398285556615,-1.30773435207906,
7.72944462297087));
#10658=CARTESIAN_POINT('Ctrl Pts',(-2.11508257455789,-1.23748775864715,
7.72522902168364));
#10659=CARTESIAN_POINT('Ctrl Pts',(-2.15618126800456,-1.16724291805077,
7.72101352558664));
#10660=CARTESIAN_POINT('Ctrl Pts',(-2.19377693308089,-1.09494827768069,
7.71679802948964));
#10661=CARTESIAN_POINT('Ctrl Pts',(-2.22767334950713,-1.02099054740761,
7.71258253339264));
#10662=CARTESIAN_POINT('Ctrl Pts',(-2.26192894312803,-0.946249137534035,
7.70832236856007));
#10663=CARTESIAN_POINT('Ctrl Pts',(-2.29240620798047,-0.869809616343446,
7.70406220372749));
#10664=CARTESIAN_POINT('Ctrl Pts',(-2.3189524794052,-0.792091944322416,
7.69980203889492));
#10665=CARTESIAN_POINT('Ctrl Pts',(-2.34525866195388,-0.715077163800797,
7.69558040369877));
#10666=CARTESIAN_POINT('Ctrl Pts',(-2.36770459988362,-0.63680772809343,
7.69135876850262));
#10667=CARTESIAN_POINT('Ctrl Pts',(-2.3861924512603,-0.557705868310855,
7.68713713330648));
#10668=CARTESIAN_POINT('Ctrl Pts',(-2.4049334024995,-0.477521099031188,
7.68285770365569));
#10669=CARTESIAN_POINT('Ctrl Pts',(-2.41960698558152,-0.396481427966423,
7.6785782740049));
#10670=CARTESIAN_POINT('Ctrl Pts',(-2.43016544912669,-0.315033553563563,
7.67429884435412));
#10671=CARTESIAN_POINT('Ctrl Pts',(-2.44072391267186,-0.233585679160702,
7.67001941470333));
#10672=CARTESIAN_POINT('Ctrl Pts',(-2.44716728347148,-0.151730095633827,
7.66573998505254));
#10673=CARTESIAN_POINT('Ctrl Pts',(-2.44950248378859,-0.0699130310708557,
7.66146055540175));
#10674=CARTESIAN_POINT('Ctrl Pts',(-2.4501633133589,-0.0467599271495813,
7.66024953567185));
#10675=CARTESIAN_POINT('Ctrl Pts',(-2.45049588145717,-0.0235974094178985,
7.65903851594195));
#10676=CARTESIAN_POINT('Ctrl Pts',(-2.45049996198422,-0.000431642580974575,
7.65782749621206));
#10677=CARTESIAN_POINT('',(-2.45049918758584,-0.00199540500347388,6.85782752364025));
#10678=CARTESIAN_POINT('Ctrl Pts',(-2.4504999619844,-0.000431641586563175,
7.65782749616008));
#10679=CARTESIAN_POINT('Ctrl Pts',(-2.45051414927918,0.0801119538488336,
7.65361697794695));
#10680=CARTESIAN_POINT('Ctrl Pts',(-2.44655306968272,0.160813628717667,
7.64940645973383));
#10681=CARTESIAN_POINT('Ctrl Pts',(-2.43859602484009,0.241246093510585,
7.64519594152071));
#10682=CARTESIAN_POINT('Ctrl Pts',(-2.43065032934474,0.321563835313509,
7.64099142888307));
#10683=CARTESIAN_POINT('Ctrl Pts',(-2.41872003131059,0.401612665828241,
7.63678691624544));
#10684=CARTESIAN_POINT('Ctrl Pts',(-2.40283644221121,0.480964948807892,
7.6325824036078));
#10685=CARTESIAN_POINT('Ctrl Pts',(-2.38697086817172,0.560227230962065,
7.62838265970011));
#10686=CARTESIAN_POINT('Ctrl Pts',(-2.36716100364736,0.638794076830931,
7.62418291579242));
#10687=CARTESIAN_POINT('Ctrl Pts',(-2.34348982424815,0.716244157843789,
7.61998317188473));
#10688=CARTESIAN_POINT('Ctrl Pts',(-2.31983319025584,0.793646647525318,
7.61578600862513));
#10689=CARTESIAN_POINT('Ctrl Pts',(-2.29232008706215,0.869933285897969,
7.61158884536554));
#10690=CARTESIAN_POINT('Ctrl Pts',(-2.26108403110359,0.944695323524109,
7.60739168210594));
#10691=CARTESIAN_POINT('Ctrl Pts',(-2.22985735715928,1.01943490573837,7.60319577949991));
#10692=CARTESIAN_POINT('Ctrl Pts',(-2.19491013179145,1.0926503630723,7.59899987689388));
#10693=CARTESIAN_POINT('Ctrl Pts',(-2.15642442957764,1.16395185876424,7.59480397428786));
#10694=CARTESIAN_POINT('Ctrl Pts',(-2.11793819786441,1.2352543354465,7.59060801395317));
#10695=CARTESIAN_POINT('Ctrl Pts',(-2.07591361739344,1.30464238543468,7.58641205361848));
#10696=CARTESIAN_POINT('Ctrl Pts',(-2.03057852696413,1.37175110564278,7.58221609328379));
#10697=CARTESIAN_POINT('Ctrl Pts',(-1.98519789816097,1.43892723548788,7.57801591817401));
#10698=CARTESIAN_POINT('Ctrl Pts',(-1.93650038246883,1.50381907313217,7.57381574306422));
#10699=CARTESIAN_POINT('Ctrl Pts',(-1.8847565881472,1.56609158526432,7.56961556795444));
#10700=CARTESIAN_POINT('Ctrl Pts',(-1.83298640190095,1.62839585949408,7.56541325054514));
#10701=CARTESIAN_POINT('Ctrl Pts',(-1.77816716181604,1.68807780204755,7.56121093313585));
#10702=CARTESIAN_POINT('Ctrl Pts',(-1.72060740202897,1.74483822117786,7.55700861572656));
#10703=CARTESIAN_POINT('Ctrl Pts',(-1.6629463687098,1.80169850744017,7.55279890454897));
#10704=CARTESIAN_POINT('Ctrl Pts',(-1.60253553610739,1.85562669028403,7.54858919337138));
#10705=CARTESIAN_POINT('Ctrl Pts',(-1.53971740741712,1.90636317507885,7.5443794821938));
#10706=CARTESIAN_POINT('Ctrl Pts',(-1.48960408144351,1.94683833812953,7.5410211741242));
#10707=CARTESIAN_POINT('Ctrl Pts',(-1.43795943764779,1.98528303519585,7.53766286605461));
#10708=CARTESIAN_POINT('Ctrl Pts',(-1.38496956816147,2.02158589856247,7.53430455798502));
#10709=CARTESIAN_POINT('Ctrl Pts',(-1.31821442288576,2.06731922346882,7.53007385605578));
#10710=CARTESIAN_POINT('Ctrl Pts',(-1.24906605095274,2.10982850004496,7.52584315412654));
#10711=CARTESIAN_POINT('Ctrl Pts',(-1.17786891945196,2.14885435955745,7.52161245219729));
#10712=CARTESIAN_POINT('Ctrl Pts',(-1.10677407864698,2.18782414964356,7.5173878286231));
#10713=CARTESIAN_POINT('Ctrl Pts',(-1.03363672858851,2.2233202406584,7.51316320504892));
#10714=CARTESIAN_POINT('Ctrl Pts',(-0.958830860654071,2.2551260786611,7.50893858147472));
#10715=CARTESIAN_POINT('Ctrl Pts',(-0.883730571369413,2.28705709825754,
7.50469733060362));
#10716=CARTESIAN_POINT('Ctrl Pts',(-0.806948993607136,2.3152684860934,7.50045607973252));
#10717=CARTESIAN_POINT('Ctrl Pts',(-0.728890171636918,2.3395874353593,7.49621482886142));
#10718=CARTESIAN_POINT('Ctrl Pts',(-0.651277692296751,2.3637673281611,7.49199782958701));
#10719=CARTESIAN_POINT('Ctrl Pts',(-0.572402984226607,2.38409903603495,
7.4877808303126));
#10720=CARTESIAN_POINT('Ctrl Pts',(-0.492682124565188,2.40046132527353,
7.48356383103818));
#10721=CARTESIAN_POINT('Ctrl Pts',(-0.412987694119799,2.41681819005383,
7.47934822979166));
#10722=CARTESIAN_POINT('Ctrl Pts',(-0.332448124346945,2.42920815602309,
7.47513262854513));
#10723=CARTESIAN_POINT('Ctrl Pts',(-0.251491314955957,2.43756074149994,
7.4709170272986));
#10724=CARTESIAN_POINT('Ctrl Pts',(-0.170536525653001,2.44591311855753,
7.46670153124256));
#10725=CARTESIAN_POINT('Ctrl Pts',(-0.0891649801482384,2.45022826877624,
7.46248603518651));
#10726=CARTESIAN_POINT('Ctrl Pts',(-0.00780992151061345,2.4504875545748,
7.45827053913046));
#10727=CARTESIAN_POINT('Ctrl Pts',(0.0744072028859268,2.45074958785351,
7.45401037425028));
#10728=CARTESIAN_POINT('Ctrl Pts',(0.156607004519655,2.44686927263525,7.4497502093701));
#10729=CARTESIAN_POINT('Ctrl Pts',(0.238343990175726,2.43888138136054,7.44549004448992));
#10730=CARTESIAN_POINT('Ctrl Pts',(0.319341731299578,2.43096573406329,7.44126840933491));
#10731=CARTESIAN_POINT('Ctrl Pts',(0.399884538280696,2.4190166412806,7.43704677417991));
#10732=CARTESIAN_POINT('Ctrl Pts',(0.479547533480251,2.40311972509341,7.4328251390249));
#10733=CARTESIAN_POINT('Ctrl Pts',(0.560301122679176,2.387005178608,7.42854570928213));
#10734=CARTESIAN_POINT('Ctrl Pts',(0.640150148698512,2.36683401927795,7.42426627953936));
#10735=CARTESIAN_POINT('Ctrl Pts',(0.718668183776595,2.34274759451957,7.41998684979659));
#10736=CARTESIAN_POINT('Ctrl Pts',(0.797186218854677,2.31866116976119,7.41570742005382));
#10737=CARTESIAN_POINT('Ctrl Pts',(0.874372824147611,2.29065970844442,7.41142799031106));
#10738=CARTESIAN_POINT('Ctrl Pts',(0.94982462113251,2.25893413783813,7.40714856056829));
#10739=CARTESIAN_POINT('Ctrl Pts',(1.02441728808841,2.22756980966057,7.40291785844694));
#10740=CARTESIAN_POINT('Ctrl Pts',(1.09759503318878,2.19244781989382,7.39868715632559));
#10741=CARTESIAN_POINT('Ctrl Pts',(1.16895329163391,2.15371735656707,7.39445645420424));
#10742=CARTESIAN_POINT('Ctrl Pts',(1.24020902791233,2.11504253825051,7.39023183043679));
#10743=CARTESIAN_POINT('Ctrl Pts',(1.30965006401606,2.07276976280726,7.38600720666934));
#10744=CARTESIAN_POINT('Ctrl Pts',(1.37689184720839,2.0270962214683,7.38178258290188));
#10745=CARTESIAN_POINT('Ctrl Pts',(1.44439827712931,1.98124292057027,7.37754133207895));
#10746=CARTESIAN_POINT('Ctrl Pts',(1.50968766814146,1.93196221118463,7.37330008125602));
#10747=CARTESIAN_POINT('Ctrl Pts',(1.57239597731041,1.87950023690821,7.36905883043309));
#10748=CARTESIAN_POINT('Ctrl Pts',(1.63474572211708,1.82733823873704,7.36484183096403));
#10749=CARTESIAN_POINT('Ctrl Pts',(1.69454346181136,1.77203155913337,7.36062483149498));
#10750=CARTESIAN_POINT('Ctrl Pts',(1.75146199913296,1.71386438074696,7.35640783202593));
#10751=CARTESIAN_POINT('Ctrl Pts',(1.80836166671137,1.65571648605564,7.35219223058466));
#10752=CARTESIAN_POINT('Ctrl Pts',(1.86238370242667,1.59471030791258,7.3479766291434));
#10753=CARTESIAN_POINT('Ctrl Pts',(1.91323717828737,1.53116744662985,7.34376102770214));
#10754=CARTESIAN_POINT('Ctrl Pts',(1.9640893852163,1.46762617091338,7.33954553145153));
#10755=CARTESIAN_POINT('Ctrl Pts',(2.011772899749,1.40154870168318,7.33533003520092));
#10756=CARTESIAN_POINT('Ctrl Pts',(2.05603748925338,1.33328920073053,7.33111453895032));
#10757=CARTESIAN_POINT('Ctrl Pts',(2.10077111685933,1.26430640589672,7.32685437430042));
#10758=CARTESIAN_POINT('Ctrl Pts',(2.14201265542884,1.19309545906634,7.32259420965052));
#10759=CARTESIAN_POINT('Ctrl Pts',(2.17955014489416,1.12004973813302,7.31833404500063));
#10760=CARTESIAN_POINT('Ctrl Pts',(2.21674814201247,1.04766464910641,7.31411240965347));
#10761=CARTESIAN_POINT('Ctrl Pts',(2.25030868244795,0.973478294070949,7.3098907743063));
#10762=CARTESIAN_POINT('Ctrl Pts',(2.28007371980181,0.897894248934212,7.30566913895914));
#10763=CARTESIAN_POINT('Ctrl Pts',(2.31024623886864,0.821275462405448,7.30138970965788));
#10764=CARTESIAN_POINT('Ctrl Pts',(2.33651838976551,0.743220896231788,7.29711028035661));
#10765=CARTESIAN_POINT('Ctrl Pts',(2.35877813837818,0.664165599763462,7.29283085105534));
#10766=CARTESIAN_POINT('Ctrl Pts',(2.38103788699085,0.585110303295135,7.28855142175408));
#10767=CARTESIAN_POINT('Ctrl Pts',(2.39928518814817,0.505054769405927,7.28427199245281));
#10768=CARTESIAN_POINT('Ctrl Pts',(2.41346217146823,0.424441511744397,7.27999256315154));
#10769=CARTESIAN_POINT('Ctrl Pts',(2.42747772865689,0.344746156434165,7.2757618615451));
#10770=CARTESIAN_POINT('Ctrl Pts',(2.43756794910575,0.264205964793622,7.27153115993865));
#10771=CARTESIAN_POINT('Ctrl Pts',(2.44363922756305,0.183241849791682,7.26730045833221));
#10772=CARTESIAN_POINT('Ctrl Pts',(2.44970178326352,0.102394057948189,7.26307583508002));
#10773=CARTESIAN_POINT('Ctrl Pts',(2.45175683019946,0.0211240121960097,
7.25885121182784));
#10774=CARTESIAN_POINT('Ctrl Pts',(2.44976195693876,-0.060138210279318,
7.25462658857565));
#10775=CARTESIAN_POINT('Ctrl Pts',(2.44775923205409,-0.141720272829519,
7.25038533762395));
#10776=CARTESIAN_POINT('Ctrl Pts',(2.44167455622559,-0.223293983005645,
7.24614408667225));
#10777=CARTESIAN_POINT('Ctrl Pts',(2.4315177793486,-0.304420003796851,7.24190283572055));
#10778=CARTESIAN_POINT('Ctrl Pts',(2.4214190801722,-0.38508213601366,7.23768583676393));
#10779=CARTESIAN_POINT('Ctrl Pts',(2.40729478148,-0.465301218741227,7.23346883780732));
#10780=CARTESIAN_POINT('Ctrl Pts',(2.38920666347201,-0.544648298648727,
7.2292518388507));
#10781=CARTESIAN_POINT('Ctrl Pts',(2.37112454206316,-0.623969073297096,
7.22503623791971));
#10782=CARTESIAN_POINT('Ctrl Pts',(2.34908131418291,-0.702417966135538,
7.22082063698871));
#10783=CARTESIAN_POINT('Ctrl Pts',(2.32318985582445,-0.779576259126962,
7.21660503605771));
#10784=CARTESIAN_POINT('Ctrl Pts',(2.29729904351051,-0.856732626862104,
7.21238954031452));
#10785=CARTESIAN_POINT('Ctrl Pts',(2.2675603406103,-0.932598018223689,7.20817404457134));
#10786=CARTESIAN_POINT('Ctrl Pts',(2.23413603237521,-1.006770300934,7.20395854882816));
#10787=CARTESIAN_POINT('Ctrl Pts',(2.20035754334729,-1.08172855048354,7.19969838357038));
#10788=CARTESIAN_POINT('Ctrl Pts',(2.16281505919034,-1.15495714735286,7.1954382183126));
#10789=CARTESIAN_POINT('Ctrl Pts',(2.12172455778278,-1.22606490484862,7.19117805305482));
#10790=CARTESIAN_POINT('Ctrl Pts',(2.08100569306159,-1.29652953922673,7.18695641820299));
#10791=CARTESIAN_POINT('Ctrl Pts',(2.03680303903082,-1.36491118172741,7.18273478335116));
#10792=CARTESIAN_POINT('Ctrl Pts',(1.98937033695942,-1.4308584529666,7.17851314849933));
#10793=CARTESIAN_POINT('Ctrl Pts',(1.94128826515444,-1.49770856465308,7.17423371803858));
#10794=CARTESIAN_POINT('Ctrl Pts',(1.88988734347876,-1.56205675916543,7.16995428757782));
#10795=CARTESIAN_POINT('Ctrl Pts',(1.83547268668684,-1.62357330183351,7.16567485711707));
#10796=CARTESIAN_POINT('Ctrl Pts',(1.78105802989493,-1.6850898445016,7.16139542665632));
#10797=CARTESIAN_POINT('Ctrl Pts',(1.72363002791887,-1.74377443049916,7.15711599619557));
#10798=CARTESIAN_POINT('Ctrl Pts',(1.66352939610883,-1.79933882253504,7.15283656573482));
#10799=CARTESIAN_POINT('Ctrl Pts',(1.60411311074133,-1.85427052082251,7.14860586376366));
#10800=CARTESIAN_POINT('Ctrl Pts',(1.54186129871659,-1.90635936664518,7.14437516179251));
#10801=CARTESIAN_POINT('Ctrl Pts',(1.47707716683612,-1.95529877338768,7.14014445982135));
#10802=CARTESIAN_POINT('Ctrl Pts',(1.4123861119746,-2.00416786763303,7.13591983620791));
#10803=CARTESIAN_POINT('Ctrl Pts',(1.34517033095112,-2.04989623151421,7.13169521259446));
#10804=CARTESIAN_POINT('Ctrl Pts',(1.27576845239048,-2.09221535839053,7.12747058898102));
#10805=CARTESIAN_POINT('Ctrl Pts',(1.20609342234507,-2.13470104462489,7.12322933812006));
#10806=CARTESIAN_POINT('Ctrl Pts',(1.13421539824854,-2.17375027803472,7.11898808725911));
#10807=CARTESIAN_POINT('Ctrl Pts',(1.06050908877473,-2.20913347777498,7.11474683639815));
#10808=CARTESIAN_POINT('Ctrl Pts',(0.987224233395099,-2.24431435569908,
7.11052983709113));
#10809=CARTESIAN_POINT('Ctrl Pts',(0.912132367711619,-2.27587080780046,
7.10631283778411));
#10810=CARTESIAN_POINT('Ctrl Pts',(0.835627586040501,-2.30362253580054,
7.10209583847709));
#10811=CARTESIAN_POINT('Ctrl Pts',(0.759148167431046,-2.3313650634765,7.09788023720051));
#10812=CARTESIAN_POINT('Ctrl Pts',(0.681257199863043,-2.35530521342064,
7.09366463592394));
#10813=CARTESIAN_POINT('Ctrl Pts',(0.602367836122385,-2.37531118803521,
7.08944903464736));
#10814=CARTESIAN_POINT('Ctrl Pts',(0.523480440929719,-2.39531666343519,
7.08523353856384));
#10815=CARTESIAN_POINT('Ctrl Pts',(0.443595150155823,-2.41138804542613,
7.08101804248031));
#10816=CARTESIAN_POINT('Ctrl Pts',(0.363137922745616,-2.42344405734153,
7.07680254639679));
#10817=CARTESIAN_POINT('Ctrl Pts',(0.281828144599183,-2.43562781864832,
7.0725423815569));
#10818=CARTESIAN_POINT('Ctrl Pts',(0.199934713527443,-2.44371051915612,
7.06828221671701));
#10819=CARTESIAN_POINT('Ctrl Pts',(0.11790345548595,-2.44766195075719,7.06402205187711));
#10820=CARTESIAN_POINT('Ctrl Pts',(0.0366141022588304,-2.45157764493086,
7.05980041670116));
#10821=CARTESIAN_POINT('Ctrl Pts',(-0.0448101247834487,-2.45143655996938,
7.0555787815252));
#10822=CARTESIAN_POINT('Ctrl Pts',(-0.125936422192143,-2.44726178974899,
7.05135714634924));
#10823=CARTESIAN_POINT('Ctrl Pts',(-0.208173344576256,-2.44302986661738,
7.04707771667738));
#10824=CARTESIAN_POINT('Ctrl Pts',(-0.290103626117359,-2.43465302941235,
7.04279828700552));
#10825=CARTESIAN_POINT('Ctrl Pts',(-0.371284847441249,-2.42220928329088,
7.03851885733366));
#10826=CARTESIAN_POINT('Ctrl Pts',(-0.452466068765136,-2.40976553716941,
7.0342394276618));
#10827=CARTESIAN_POINT('Ctrl Pts',(-0.532897762473629,-2.39325504493292,
7.02995999798993));
#10828=CARTESIAN_POINT('Ctrl Pts',(-0.612153123812642,-2.37280821032936,
7.02568056831807));
#10829=CARTESIAN_POINT('Ctrl Pts',(-0.690506065164704,-2.35259418814258,
7.02144986522828));
#10830=CARTESIAN_POINT('Ctrl Pts',(-0.768004043535359,-2.32845701955206,
7.01721916213848));
#10831=CARTESIAN_POINT('Ctrl Pts',(-0.844225134002871,-2.30048563853762,
7.01298845904869));
#10832=CARTESIAN_POINT('Ctrl Pts',(-0.920336715861448,-2.27255444465519,
7.00876383430817));
#10833=CARTESIAN_POINT('Ctrl Pts',(-0.995174620417518,-2.24080013779327,
7.00453920956766));
#10834=CARTESIAN_POINT('Ctrl Pts',(-1.06832976100188,-2.20536205004023,
7.00031458482714));
#10835=CARTESIAN_POINT('Ctrl Pts',(-1.14177280068195,-2.16978449712677,
6.9960733342469));
#10836=CARTESIAN_POINT('Ctrl Pts',(-1.21351934357818,-2.13049422494611,
6.99183208366666));
#10837=CARTESIAN_POINT('Ctrl Pts',(-1.28317349642087,-2.08768197484268,
6.98759083308642));
#10838=CARTESIAN_POINT('Ctrl Pts',(-1.35242938877218,-2.04511451169118,
6.98337383264018));
#10839=CARTESIAN_POINT('Ctrl Pts',(-1.41961635321147,-1.99906548242192,
6.97915683219393));
#10840=CARTESIAN_POINT('Ctrl Pts',(-1.4843694351532,-1.94976860934393,6.97493983174769));
#10841=CARTESIAN_POINT('Ctrl Pts',(-1.54910105002411,-1.90048807926359,
6.97072422932985));
#10842=CARTESIAN_POINT('Ctrl Pts',(-1.61140001499802,-1.84796212506383,
6.966508626912));
#10843=CARTESIAN_POINT('Ctrl Pts',(-1.6709318343281,-1.79246675144308,6.96229302449416));
#10844=CARTESIAN_POINT('Ctrl Pts',(-1.73046216815164,-1.73697276260684,
6.95807752726888));
#10845=CARTESIAN_POINT('Ctrl Pts',(-1.78722515418016,-1.67850981957754,
6.9538620300436));
#10846=CARTESIAN_POINT('Ctrl Pts',(-1.8409218391178,-1.61739204655492,6.94964653281833));
#10847=CARTESIAN_POINT('Ctrl Pts',(-1.8951874795977,-1.55562668614899,6.94538636932524));
#10848=CARTESIAN_POINT('Ctrl Pts',(-1.94632112084788,-1.49115025438227,
6.94112620583216));
#10849=CARTESIAN_POINT('Ctrl Pts',(-1.99405599006674,-1.42432122727949,
6.93686604233908));
#10850=CARTESIAN_POINT('Ctrl Pts',(-2.04135916454392,-1.358096574716,6.93264440603186));
#10851=CARTESIAN_POINT('Ctrl Pts',(-2.08532459200953,-1.2895621366162,6.92842276972465));
#10852=CARTESIAN_POINT('Ctrl Pts',(-2.12573736376488,-1.21909429918032,
6.92420113341743));
#10853=CARTESIAN_POINT('Ctrl Pts',(-2.16670335360515,-1.14766181417434,
6.91992170633141));
#10854=CARTESIAN_POINT('Ctrl Pts',(-2.20401846124588,-1.07424303669084,
6.9156422792454));
#10855=CARTESIAN_POINT('Ctrl Pts',(-2.23750873930705,-0.999252166134541,
6.91136285215939));
#10856=CARTESIAN_POINT('Ctrl Pts',(-2.27099901736822,-0.924261295578242,
6.90708342507337));
#10857=CARTESIAN_POINT('Ctrl Pts',(-2.30066434967179,-0.847698813057868,
6.90280399798736));
#10858=CARTESIAN_POINT('Ctrl Pts',(-2.32638329709889,-0.769994159055309,
6.89852457090134));
#10859=CARTESIAN_POINT('Ctrl Pts',(-2.3566686452367,-0.67849303891555,6.89348533127081));
#10860=CARTESIAN_POINT('Ctrl Pts',(-2.38157637743318,-0.585128820600957,
6.88844609164027));
#10861=CARTESIAN_POINT('Ctrl Pts',(-2.40091147363867,-0.490483787448861,
6.88340685200973));
#10862=CARTESIAN_POINT('Ctrl Pts',(-2.42003159244815,-0.396891065728579,
6.87842364119861));
#10863=CARTESIAN_POINT('Ctrl Pts',(-2.43370224826641,-0.302045926058559,
6.8734404303875));
#10864=CARTESIAN_POINT('Ctrl Pts',(-2.44178104459956,-0.206532274074234,
6.86845721957638));
#10865=CARTESIAN_POINT('Ctrl Pts',(-2.44752534292489,-0.138618826511733,
6.86491398759767));
#10866=CARTESIAN_POINT('Ctrl Pts',(-2.45044351293468,-0.0703678342595561,
6.86137075561896));
#10867=CARTESIAN_POINT('Ctrl Pts',(-2.45049918758584,-0.00199540500347388,
6.85782752364025));
#10868=CARTESIAN_POINT('',(-2.44727079087888,0.00140258600070248,6.05782749621206));
#10869=CARTESIAN_POINT('Ctrl Pts',(-2.44847580618664,-0.00199322855914286,
6.85782749621206));
#10870=CARTESIAN_POINT('Ctrl Pts',(-2.44423578927424,0.553673293985754,
6.82900785530291));
#10871=CARTESIAN_POINT('Ctrl Pts',(-1.98117851569519,1.93295874884265,6.75780288192152));
#10872=CARTESIAN_POINT('Ctrl Pts',(0.309238178351472,2.88090180145063,6.64421257606786));
#10873=CARTESIAN_POINT('Ctrl Pts',(2.5895656520796,1.29976107516381,6.51705657865114));
#10874=CARTESIAN_POINT('Ctrl Pts',(2.4948043245916,-1.47349273530034,6.38990058123439));
#10875=CARTESIAN_POINT('Ctrl Pts',(0.111868608253771,-2.89528816042125,
6.26274458381766));
#10876=CARTESIAN_POINT('Ctrl Pts',(-2.05182862477049,-1.82135004090711,
6.15205355547688));
#10877=CARTESIAN_POINT('Ctrl Pts',(-2.44467631807943,-0.498983029647765,
6.08374785960835));
#10878=CARTESIAN_POINT('Ctrl Pts',(-2.44727079087888,0.00140258600070248,
6.05782749621206));
#10879=CARTESIAN_POINT('Ctrl Pts',(-2.44727079087888,0.00140258600070248,
6.05782749621206));
#10880=CARTESIAN_POINT('Ctrl Pts',(-2.44891883545906,0.31925436769618,6.0413625271361));
#10881=CARTESIAN_POINT('Ctrl Pts',(-2.24355247310808,1.45329452179378,5.98251222558789));
#10882=CARTESIAN_POINT('Ctrl Pts',(-0.530612503065825,2.84843065415222,
5.88127659156747));
#10883=CARTESIAN_POINT('Ctrl Pts',(2.10758727991065,1.98834031509364,5.75412059415071));
#10884=CARTESIAN_POINT('Ctrl Pts',(2.812732038963,-0.695553730705045,5.62696459673398));
#10885=CARTESIAN_POINT('Ctrl Pts',(0.938155002898276,-2.7412257732876,5.49980859931725));
#10886=CARTESIAN_POINT('Ctrl Pts',(-1.70855726544326,-2.28836551633789,
5.37676289914326));
#10887=CARTESIAN_POINT('Ctrl Pts',(-2.448662628639,-0.732444886033958,5.29610253144154));
#10888=CARTESIAN_POINT('Ctrl Pts',(-2.45356474526275,0.00152995343032009,
5.25782749621206));
#10889=CARTESIAN_POINT('Origin',(0.,0.,3.52095488139519));
#10890=CARTESIAN_POINT('',(-1.13766281679009,-1.63852094212837,5.));
#10891=CARTESIAN_POINT('',(-1.99474929467261,-0.00167746926262795,6.47978083014939));
#10892=CARTESIAN_POINT('Ctrl Pts',(-1.99474929622187,-0.00167562595544705,
6.47978072236948));
#10893=CARTESIAN_POINT('Ctrl Pts',(-1.99483545784495,0.100895497651632,
6.47378329174917));
#10894=CARTESIAN_POINT('Ctrl Pts',(-1.98701043932826,0.203310863465348,
6.4676806320529));
#10895=CARTESIAN_POINT('Ctrl Pts',(-1.96937497030234,0.317421448938346,
6.46052004982015));
#10896=CARTESIAN_POINT('Ctrl Pts',(-1.96727993673741,0.330157217431481,
6.45971591010473));
#10897=CARTESIAN_POINT('Ctrl Pts',(-1.963773434283,0.350253645291977,6.45843877103503));
#10898=CARTESIAN_POINT('Ctrl Pts',(-1.96244380023555,0.357628362555231,
6.45796834281405));
#10899=CARTESIAN_POINT('Ctrl Pts',(-1.96011217704298,0.370155872022657,
6.45716614897992));
#10900=CARTESIAN_POINT('Ctrl Pts',(-1.9591313376779,0.375312559156564,6.4568350552308));
#10901=CARTESIAN_POINT('Ctrl Pts',(-1.95726986988266,0.384892924240948,
6.4562182546167));
#10902=CARTESIAN_POINT('Ctrl Pts',(-1.95639456720463,0.389317612686523,
6.45593271890036));
#10903=CARTESIAN_POINT('Ctrl Pts',(-1.95454910215499,0.398483106474347,
6.45533984795679));
#10904=CARTESIAN_POINT('Ctrl Pts',(-1.95357668142963,0.403223421909805,
6.45503244234779));
#10905=CARTESIAN_POINT('Ctrl Pts',(-1.95131894196877,0.414029460517692,
6.45432988210507));
#10906=CARTESIAN_POINT('Ctrl Pts',(-1.9500225755942,0.420092800105781,6.45393437629805));
#10907=CARTESIAN_POINT('Ctrl Pts',(-1.94596819471851,0.438632668434363,
6.45272101625882));
#10908=CARTESIAN_POINT('Ctrl Pts',(-1.94311859336475,0.451088630052562,
6.45190023447609));
#10909=CARTESIAN_POINT('Ctrl Pts',(-1.91673115779224,0.561539097367733,
6.44457117467772));
#10910=CARTESIAN_POINT('Ctrl Pts',(-1.88592180806099,0.65763034597248,6.43782599008551));
#10911=CARTESIAN_POINT('Ctrl Pts',(-1.83102027101028,0.792732209204058,
6.42781686022865));
#10912=CARTESIAN_POINT('Ctrl Pts',(-1.81263947984916,0.833904925648595,
6.42469358502988));
#10913=CARTESIAN_POINT('Ctrl Pts',(-1.77596335178935,0.909104539903885,
6.41887035459788));
#10914=CARTESIAN_POINT('Ctrl Pts',(-1.75804329577687,0.943292440308809,
6.41617538920016));
#10915=CARTESIAN_POINT('Ctrl Pts',(-1.6931828168785,1.05875684170231,6.40693979961625));
#10916=CARTESIAN_POINT('Ctrl Pts',(-1.64150169914192,1.13723770495279,6.40042327456305));
#10917=CARTESIAN_POINT('Ctrl Pts',(-1.57107855529992,1.22931954274143,6.3927050128987));
#10918=CARTESIAN_POINT('Ctrl Pts',(-1.55738454599874,1.24662257378676,6.39125157235773));
#10919=CARTESIAN_POINT('Ctrl Pts',(-1.54002211389152,1.26782805436302,6.38947009772506));
#10920=CARTESIAN_POINT('Ctrl Pts',(-1.53662202572881,1.27194686930946,6.38912406516935));
#10921=CARTESIAN_POINT('Ctrl Pts',(-1.53123558281951,1.27841880232028,6.38858039218694));
#10922=CARTESIAN_POINT('Ctrl Pts',(-1.52926028282817,1.28078102417959,6.38838196522768));
#10923=CARTESIAN_POINT('Ctrl Pts',(-1.52554376976702,1.28520467246108,6.38801041412956));
#10924=CARTESIAN_POINT('Ctrl Pts',(-1.52380386401095,1.28726711591932,6.38783720203768));
#10925=CARTESIAN_POINT('Ctrl Pts',(-1.51982425555209,1.29196507559292,6.38744267825979));
#10926=CARTESIAN_POINT('Ctrl Pts',(-1.51758188462613,1.29459829607974,6.38722156597914));
#10927=CARTESIAN_POINT('Ctrl Pts',(-1.51068680961063,1.30265266346664,6.38654525043112));
#10928=CARTESIAN_POINT('Ctrl Pts',(-1.50601175842704,1.30805473339989,6.38609166184389));
#10929=CARTESIAN_POINT('Ctrl Pts',(-1.46849566989697,1.35093720225692,6.38249004175736));
#10930=CARTESIAN_POINT('Ctrl Pts',(-1.43428646804993,1.38720371466403,6.37943807103119));
#10931=CARTESIAN_POINT('Ctrl Pts',(-1.38618047241073,1.43451809404303,6.37538544944971));
#10932=CARTESIAN_POINT('Ctrl Pts',(-1.37344580270871,1.44671528620066,6.37433393248397));
#10933=CARTESIAN_POINT('Ctrl Pts',(-1.30422033565708,1.51128101896889,6.36872016674912));
#10934=CARTESIAN_POINT('Ctrl Pts',(-1.24489149383222,1.56051503964148,6.36426581366972));
#10935=CARTESIAN_POINT('Ctrl Pts',(-1.10458100944215,1.66384482259954,6.3541587884084));
#10936=CARTESIAN_POINT('Ctrl Pts',(-1.02219467798493,1.71569079889588,6.34850760007928));
#10937=CARTESIAN_POINT('Ctrl Pts',(-0.902002049954595,1.77958820547176,
6.34032786939562));
#10938=CARTESIAN_POINT('Ctrl Pts',(-0.867116258291207,1.79684473030039,
6.33796194397986));
#10939=CARTESIAN_POINT('Ctrl Pts',(-0.809148149437407,1.8234377342857,6.33402825651246));
#10940=CARTESIAN_POINT('Ctrl Pts',(-0.786355536221787,1.83338233401351,
6.33248104399878));
#10941=CARTESIAN_POINT('Ctrl Pts',(-0.755949547503772,1.84597740904105,
6.33041388425508));
#10942=CARTESIAN_POINT('Ctrl Pts',(-0.748496865557286,1.84901183128992,
6.32990696939371));
#10943=CARTESIAN_POINT('Ctrl Pts',(-0.736829242274105,1.85368030250194,
6.32911290575315));
#10944=CARTESIAN_POINT('Ctrl Pts',(-0.732626702307686,1.85534528071483,
6.32882680122559));
#10945=CARTESIAN_POINT('Ctrl Pts',(-0.723928664410519,1.85875714184884,
6.32823444029299));
#10946=CARTESIAN_POINT('Ctrl Pts',(-0.719432421645852,1.86050203266296,
6.32792811927288));
#10947=CARTESIAN_POINT('Ctrl Pts',(-0.709279634326413,1.86439979459841,
6.32723614944195));
#10948=CARTESIAN_POINT('Ctrl Pts',(-0.703619550282622,1.86654325449338,
6.32685018844351));
#10949=CARTESIAN_POINT('Ctrl Pts',(-0.689120847414753,1.87195855883133,
6.32586098253435));
#10950=CARTESIAN_POINT('Ctrl Pts',(-0.680268713248486,1.87519355295221,
6.32525651476466));
#10951=CARTESIAN_POINT('Ctrl Pts',(-0.628244223989518,1.89378893971041,
6.3217007059215));
#10952=CARTESIAN_POINT('Ctrl Pts',(-0.58457894865682,1.90771964158041,6.31870241676991));
#10953=CARTESIAN_POINT('Ctrl Pts',(-0.410651896070864,1.95667629777106,
6.30669462949979));
#10954=CARTESIAN_POINT('Ctrl Pts',(-0.277474502821969,1.97995323086137,
6.29732692835705));
#10955=CARTESIAN_POINT('Ctrl Pts',(-0.0671962521706056,1.99506558345611,
6.28261850168907));
#10956=CARTESIAN_POINT('Ctrl Pts',(0.00885162920110615,1.99617757585605,
6.27732407312693));
#10957=CARTESIAN_POINT('Ctrl Pts',(0.115373037623233,1.99164610082271,6.2700756496008));
#10958=CARTESIAN_POINT('Ctrl Pts',(0.14593287779101,1.98964040498711,6.26801596116497));
#10959=CARTESIAN_POINT('Ctrl Pts',(0.19404508037269,1.98536812464061,6.26481644041901));
#10960=CARTESIAN_POINT('Ctrl Pts',(0.211633251299721,1.98357039289723,6.26365595607929));
#10961=CARTESIAN_POINT('Ctrl Pts',(0.234087125333168,1.98097325174916,6.26218810326669));
#10962=CARTESIAN_POINT('Ctrl Pts',(0.238976276339238,1.98038939276991,6.26186932122211));
#10963=CARTESIAN_POINT('Ctrl Pts',(0.246827286499457,1.97942233284843,6.26135881036512));
#10964=CARTESIAN_POINT('Ctrl Pts',(0.249790495085022,1.97905057792708,6.26116644657866));
#10965=CARTESIAN_POINT('Ctrl Pts',(0.255450902701729,1.97832752518511,6.26079961078503));
#10966=CARTESIAN_POINT('Ctrl Pts',(0.258148185381015,1.97797736970302,6.26062507957087));
#10967=CARTESIAN_POINT('Ctrl Pts',(0.264380546801473,1.97715533230295,6.26022242311067));
#10968=CARTESIAN_POINT('Ctrl Pts',(0.267915081921974,1.97667948614402,6.25999452395423));
#10969=CARTESIAN_POINT('Ctrl Pts',(0.278992644397972,1.97515788154757,6.25928164912899));
#10970=CARTESIAN_POINT('Ctrl Pts',(0.286531083075442,1.97407839144626,6.25879853859943));
#10971=CARTESIAN_POINT('Ctrl Pts',(0.367182079548968,1.9620575955819,6.25364968208958));
#10972=CARTESIAN_POINT('Ctrl Pts',(0.439648080560575,1.94710169364371,6.24919673160379));
#10973=CARTESIAN_POINT('Ctrl Pts',(0.649999597695964,1.89134069608987,6.2363481732548));
#10974=CARTESIAN_POINT('Ctrl Pts',(0.784491178788448,1.83963174432793,6.22820483318484));
#10975=CARTESIAN_POINT('Ctrl Pts',(0.960232980314657,1.74925403133659,6.21648535583192));
#10976=CARTESIAN_POINT('Ctrl Pts',(1.00717766616614,1.72265188078188,6.21324263821359));
#10977=CARTESIAN_POINT('Ctrl Pts',(1.07076977977223,1.68312749457902,6.20865138836919));
#10978=CARTESIAN_POINT('Ctrl Pts',(1.08837961537673,1.67179419998456,6.20735799507431));
#10979=CARTESIAN_POINT('Ctrl Pts',(1.11462089798262,1.65431555613821,6.20539535499746));
#10980=CARTESIAN_POINT('Ctrl Pts',(1.123387494083,1.64837502918241,6.20473362988915));
#10981=CARTESIAN_POINT('Ctrl Pts',(1.13937934459163,1.63735161293312,6.2035151157058));
#10982=CARTESIAN_POINT('Ctrl Pts',(1.14661896801578,1.63228996609139,6.20295913405017));
#10983=CARTESIAN_POINT('Ctrl Pts',(1.15817270784372,1.62409727327752,6.2020647204416));
#10984=CARTESIAN_POINT('Ctrl Pts',(1.16250836543807,1.62099669143672,6.20172745823199));
#10985=CARTESIAN_POINT('Ctrl Pts',(1.16683711738787,1.61787474917985,6.20138908820981));
#10986=CARTESIAN_POINT('Ctrl Pts',(1.1668427251728,1.61787070474099,6.20138864985752));
#10987=CARTESIAN_POINT('Ctrl Pts',(1.16685395790826,1.61786260339434,6.20138777180559));
#10988=CARTESIAN_POINT('Ctrl Pts',(1.16685958274033,1.61785854657172,6.20138733211519));
#10989=CARTESIAN_POINT('Ctrl Pts',(1.1668708493223,1.61785042063543,6.20138645140633));
#10990=CARTESIAN_POINT('Ctrl Pts',(1.16687649115576,1.61784635146123,6.20138601038133));
#10991=CARTESIAN_POINT('Ctrl Pts',(1.16688779196573,1.61783820065853,6.20138512698563));
#10992=CARTESIAN_POINT('Ctrl Pts',(1.16689345090486,1.61783411905672,6.20138468461783));
#10993=CARTESIAN_POINT('Ctrl Pts',(1.16690478602028,1.61782594333011,6.20138379852913));
#10994=CARTESIAN_POINT('Ctrl Pts',(1.1669104621646,1.61782184922808,6.20138335481071));
#10995=CARTESIAN_POINT('Ctrl Pts',(1.16692183156641,1.61781364858965,6.20138246603039));
#10996=CARTESIAN_POINT('Ctrl Pts',(1.1669275249085,1.61780954199195,6.20138202096186));
#10997=CARTESIAN_POINT('Ctrl Pts',(1.1669389288723,1.61780131624126,6.20138112946828));
#10998=CARTESIAN_POINT('Ctrl Pts',(1.16694463948499,1.6177971970945,6.20138068304391));
#10999=CARTESIAN_POINT('Ctrl Pts',(1.16695607815501,1.61778894612584,6.20137978882569));
#11000=CARTESIAN_POINT('Ctrl Pts',(1.1669618061394,1.61778481435627,6.20137934103752));
#11001=CARTESIAN_POINT('Ctrl Pts',(1.16697327957827,1.61777653812278,6.20137844408965));
#11002=CARTESIAN_POINT('Ctrl Pts',(1.16697902500957,1.6177723936753,6.20137799493174));
#11003=CARTESIAN_POINT('Ctrl Pts',(1.16699053327574,1.61776409213312,6.20137709524955));
#11004=CARTESIAN_POINT('Ctrl Pts',(1.16699629617251,1.61775993499349,6.20137664472041));
#11005=CARTESIAN_POINT('Ctrl Pts',(1.16700783944966,1.61775160800842,6.20137574228943));
#11006=CARTESIAN_POINT('Ctrl Pts',(1.16701361984161,1.61774743815436,6.20137529038668));
#11007=CARTESIAN_POINT('Ctrl Pts',(1.16702519843997,1.61773908550089,6.20137438518255));
#11008=CARTESIAN_POINT('Ctrl Pts',(1.16703099650494,1.61773490280323,6.20137393189223));
#11009=CARTESIAN_POINT('Ctrl Pts',(1.16704261023854,1.6177265246138,6.20137302392938));
#11010=CARTESIAN_POINT('Ctrl Pts',(1.16704842595355,1.61772232908827,6.20137256925323));
#11011=CARTESIAN_POINT('Ctrl Pts',(1.16706007514067,1.61771392513151,6.20137165850668));
#11012=CARTESIAN_POINT('Ctrl Pts',(1.16706590858467,1.61770971672027,6.20137120243846));
#11013=CARTESIAN_POINT('Ctrl Pts',(1.16707759338638,1.61770128687824,6.2013702888955));
#11014=CARTESIAN_POINT('Ctrl Pts',(1.16708344468417,1.61769706549038,6.20136983142542));
#11015=CARTESIAN_POINT('Ctrl Pts',(1.1670951650322,1.61768860981056,6.20136891509127));
#11016=CARTESIAN_POINT('Ctrl Pts',(1.1671010341701,1.61768437545507,6.20136845622033));
#11017=CARTESIAN_POINT('Ctrl Pts',(1.16711279038519,1.61767589370429,6.20136753706982));
#11018=CARTESIAN_POINT('Ctrl Pts',(1.16711867746088,1.6176716463098,6.20136707679033));
#11019=CARTESIAN_POINT('Ctrl Pts',(1.16713046958509,1.61766313845594,6.20136615482004));
#11020=CARTESIAN_POINT('Ctrl Pts',(1.16713637463946,1.61765887799204,6.20136569312876));
#11021=CARTESIAN_POINT('Ctrl Pts',(1.16714820292851,1.61765034384878,6.20136476831859));
#11022=CARTESIAN_POINT('Ctrl Pts',(1.16715412610175,1.61764607021344,6.20136430520449));
#11023=CARTESIAN_POINT('Ctrl Pts',(1.16716599042766,1.61763750987132,6.20136337756433));
#11024=CARTESIAN_POINT('Ctrl Pts',(1.167171931674,1.61763322309665,6.20136291303093));
#11025=CARTESIAN_POINT('Ctrl Pts',(1.1671838324892,1.6176246362274,6.2013619825253));
#11026=CARTESIAN_POINT('Ctrl Pts',(1.16718979197073,1.61762033619553,6.20136151655988));
#11027=CARTESIAN_POINT('Ctrl Pts',(1.16720172917041,1.61761172287293,6.20136058319685));
#11028=CARTESIAN_POINT('Ctrl Pts',(1.16720770690673,1.6176074095688,6.20136011579781));
#11029=CARTESIAN_POINT('Ctrl Pts',(1.1672196807526,1.61759876960217,6.20135917955681));
#11030=CARTESIAN_POINT('Ctrl Pts',(1.16722567684419,1.61759444295234,6.20135871071624));
#11031=CARTESIAN_POINT('Ctrl Pts',(1.16723768734518,1.61758577633339,6.20135777159645));
#11032=CARTESIAN_POINT('Ctrl Pts',(1.16724370180057,1.61758143633077,6.20135730131362));
#11033=CARTESIAN_POINT('Ctrl Pts',(1.16725574926075,1.61757274283819,6.20135635929115));
#11034=CARTESIAN_POINT('Ctrl Pts',(1.16726178219903,1.61756838939591,6.20135588755669));
#11035=CARTESIAN_POINT('Ctrl Pts',(1.16727386665867,1.61755966899877,6.20135494262827));
#11036=CARTESIAN_POINT('Ctrl Pts',(1.16727991815537,1.61755530206138,6.20135446943622));
#11037=CARTESIAN_POINT('Ctrl Pts',(1.1672920396957,1.61754655469914,6.20135352159538));
#11038=CARTESIAN_POINT('Ctrl Pts',(1.16729810977938,1.61754217424508,6.20135304694344));
#11039=CARTESIAN_POINT('Ctrl Pts',(1.16731026860616,1.61753339976737,6.20135209617397));
#11040=CARTESIAN_POINT('Ctrl Pts',(1.16731635733521,1.61752900575354,6.20135162005752));
#11041=CARTESIAN_POINT('Ctrl Pts',(1.1673285537123,1.617520203968,6.20135066633867));
#11042=CARTESIAN_POINT('Ctrl Pts',(1.16733466126203,1.61751579626691,6.20135018874394));
#11043=CARTESIAN_POINT('Ctrl Pts',(1.16734689496726,1.61750696733194,6.20134923209296));
#11044=CARTESIAN_POINT('Ctrl Pts',(1.16735302125991,1.61750254599875,6.20134875302597));
#11045=CARTESIAN_POINT('Ctrl Pts',(1.16736529280305,1.6174936895445,6.20134779340287));
#11046=CARTESIAN_POINT('Ctrl Pts',(1.16737143798602,1.61748925447185,6.20134731285203));
#11047=CARTESIAN_POINT('Ctrl Pts',(1.16738374734558,1.61748037051186,6.20134635025837));
#11048=CARTESIAN_POINT('Ctrl Pts',(1.16738991148429,1.61747592165153,6.2013458682185));
#11049=CARTESIAN_POINT('Ctrl Pts',(1.1674022588263,1.61746701006401,6.20134490264118));
#11050=CARTESIAN_POINT('Ctrl Pts',(1.1674084420091,1.61746254735126,6.20134441910532));
#11051=CARTESIAN_POINT('Ctrl Pts',(1.16742082737896,1.61745360810143,6.20134345054065));
#11052=CARTESIAN_POINT('Ctrl Pts',(1.1674270296184,1.6174491315262,6.20134296550774));
#11053=CARTESIAN_POINT('Ctrl Pts',(1.16743945331582,1.61744016439574,6.20134199393218));
#11054=CARTESIAN_POINT('Ctrl Pts',(1.16744567472654,1.61743567387429,6.20134150739319));
#11055=CARTESIAN_POINT('Ctrl Pts',(1.16745813680016,1.61742667882607,6.20134053280279));
#11056=CARTESIAN_POINT('Ctrl Pts',(1.16746437744894,1.61742217430916,6.20134004475245));
#11057=CARTESIAN_POINT('Ctrl Pts',(1.16747687802406,1.61741315125073,6.20133906713729));
#11058=CARTESIAN_POINT('Ctrl Pts',(1.16748313795783,1.61740863270348,6.20133857757186));
#11059=CARTESIAN_POINT('Ctrl Pts',(1.16749567725866,1.61739958147092,6.20133759691427));
#11060=CARTESIAN_POINT('Ctrl Pts',(1.16750195658278,1.61739504881626,6.20133710582545));
#11061=CARTESIAN_POINT('Ctrl Pts',(1.16751453465434,1.61738596937503,6.20133612212178));
#11062=CARTESIAN_POINT('Ctrl Pts',(1.16752083341089,1.61738142258154,6.20133562950621));
#11063=CARTESIAN_POINT('Ctrl Pts',(1.16753345051829,1.61737231473819,6.20133464273561));
#11064=CARTESIAN_POINT('Ctrl Pts',(1.16753976884214,1.61736775370747,6.20133414858267));
#11065=CARTESIAN_POINT('Ctrl Pts',(1.16755242488283,1.61735861753395,6.20133315875302));
#11066=CARTESIAN_POINT('Ctrl Pts',(1.16755876272582,1.61735404229972,6.20133266306642));
#11067=CARTESIAN_POINT('Ctrl Pts',(1.16757145817837,1.61734487744844,6.20133167014016));
#11068=CARTESIAN_POINT('Ctrl Pts',(1.16757781570674,1.61734028788965,6.20133117290683));
#11069=CARTESIAN_POINT('Ctrl Pts',(1.16759055051545,1.6173310943987,6.20133017688818));
#11070=CARTESIAN_POINT('Ctrl Pts',(1.16759692778888,1.61732649047118,6.20132967810338));
#11071=CARTESIAN_POINT('Ctrl Pts',(1.16760970206933,1.617317268255,6.20132867898318));
#11072=CARTESIAN_POINT('Ctrl Pts',(1.167616099105,1.61731264994529,6.2013281786455));
#11073=CARTESIAN_POINT('Ctrl Pts',(1.17154924071912,1.61447310142397,6.20102054973219));
#11074=CARTESIAN_POINT('Ctrl Pts',(1.17546561882557,1.61162390058299,6.20071287055676));
#11075=CARTESIAN_POINT('Ctrl Pts',(1.18439653130153,1.60507670837164,6.20000809586637));
#11076=CARTESIAN_POINT('Ctrl Pts',(1.18940417405175,1.60136944282339,6.1996106413179));
#11077=CARTESIAN_POINT('Ctrl Pts',(1.20475020153467,1.5898967570584,6.19838553768148));
#11078=CARTESIAN_POINT('Ctrl Pts',(1.21503035429342,1.58205435155071,6.19755487840136));
#11079=CARTESIAN_POINT('Ctrl Pts',(1.31283042549924,1.5059302549315,6.18955479129185));
#11080=CARTESIAN_POINT('Ctrl Pts',(1.39456791579108,1.43056716216406,6.18209546318093));
#11081=CARTESIAN_POINT('Ctrl Pts',(1.58017988328052,1.22833265497639,6.16317566618876));
#11082=CARTESIAN_POINT('Ctrl Pts',(1.67551834430475,1.09471829609673,6.15153291966259));
#11083=CARTESIAN_POINT('Ctrl Pts',(1.7655876895568,0.928640282536424,6.13891008189978));
#11084=CARTESIAN_POINT('Ctrl Pts',(1.77726939827769,0.906082943360314,6.13723293126986));
#11085=CARTESIAN_POINT('Ctrl Pts',(1.79097575625745,0.878330356717615,6.13522003300546));
#11086=CARTESIAN_POINT('Ctrl Pts',(1.79341303610973,0.873343036116761,6.13486026386835));
#11087=CARTESIAN_POINT('Ctrl Pts',(1.79719015755045,0.865531553428992,6.13429990467391));
#11088=CARTESIAN_POINT('Ctrl Pts',(1.79854421010301,0.862714354240172,6.13409844678299));
#11089=CARTESIAN_POINT('Ctrl Pts',(1.80105219526685,0.857464751667521,6.13372424413561));
#11090=CARTESIAN_POINT('Ctrl Pts',(1.80220781380114,0.855033219496038,6.1335513975929));
#11091=CARTESIAN_POINT('Ctrl Pts',(1.8048076775525,0.849534169211961,6.1331615678815));
#11092=CARTESIAN_POINT('Ctrl Pts',(1.80624902283492,0.846465312659504,6.13294476585074));
#11093=CARTESIAN_POINT('Ctrl Pts',(1.81046795662747,0.837422677624703,6.13230810352624));
#11094=CARTESIAN_POINT('Ctrl Pts',(1.81322381793899,0.831438724117706,6.13188956369581));
#11095=CARTESIAN_POINT('Ctrl Pts',(1.83181961182467,0.790528438261178,6.12904626848214));
#11096=CARTESIAN_POINT('Ctrl Pts',(1.8466803477236,0.755162540750613,6.1266781007164));
#11097=CARTESIAN_POINT('Ctrl Pts',(1.89084654305761,0.640937872351519,6.11924502511665));
#11098=CARTESIAN_POINT('Ctrl Pts',(1.91619033775963,0.560641539955537,6.11433854531592));
#11099=CARTESIAN_POINT('Ctrl Pts',(1.96058035079472,0.381184061292047,6.10360402756647));
#11100=CARTESIAN_POINT('Ctrl Pts',(1.97732676532404,0.281699036557145,6.09779666075204));
#11101=CARTESIAN_POINT('Ctrl Pts',(1.99114965917706,0.130309267377016,6.08876253496379));
#11102=CARTESIAN_POINT('Ctrl Pts',(1.99384125902702,0.0790815978831233,
6.08567371482998));
#11103=CARTESIAN_POINT('Ctrl Pts',(1.99498302481693,-0.00280721763638021,
6.08064711494166));
#11104=CARTESIAN_POINT('Ctrl Pts',(1.99470486916856,-0.0334286616570386,
6.07874777226864));
#11105=CARTESIAN_POINT('Ctrl Pts',(1.99344266254815,-0.0727301800558009,
6.07628010080449));
#11106=CARTESIAN_POINT('Ctrl Pts',(1.99310632073564,-0.0814279947685661,
6.07573210282954));
#11107=CARTESIAN_POINT('Ctrl Pts',(1.99247203792964,-0.0954526117014155,
6.07484535865277));
#11108=CARTESIAN_POINT('Ctrl Pts',(1.99220963197063,-0.100780972377443,
6.07450772827141));
#11109=CARTESIAN_POINT('Ctrl Pts',(1.99166829518422,-0.110943268996255,
6.07386237673639));
#11110=CARTESIAN_POINT('Ctrl Pts',(1.99139313192672,-0.115777374358363,
6.07355477602906));
#11111=CARTESIAN_POINT('Ctrl Pts',(1.99072381174659,-0.126826866884556,
6.07285025763432));
#11112=CARTESIAN_POINT('Ctrl Pts',(1.99031814327962,-0.133041481862757,
6.07245298136447));
#11113=CARTESIAN_POINT('Ctrl Pts',(1.98898144361166,-0.15214237476871,6.07122870810039));
#11114=CARTESIAN_POINT('Ctrl Pts',(1.98795432907092,-0.165021385584337,
6.07039870557162));
#11115=CARTESIAN_POINT('Ctrl Pts',(1.97696042151785,-0.287809682854197,
6.06244099233957));
#11116=CARTESIAN_POINT('Ctrl Pts',(1.95801560505594,-0.396704365877378,
6.05502683770449));
#11117=CARTESIAN_POINT('Ctrl Pts',(1.8867623249582,-0.669876521328289,6.03557328451888));
#11118=CARTESIAN_POINT('Ctrl Pts',(1.82201671894246,-0.829977488385105,
6.02330309043042));
#11119=CARTESIAN_POINT('Ctrl Pts',(1.72839140978783,-0.99601080332654,6.01066247690451));
#11120=CARTESIAN_POINT('Ctrl Pts',(1.7190168608733,-1.01210448053465,6.00943901982118));
#11121=CARTESIAN_POINT('Ctrl Pts',(1.70683388478276,-1.0323617532933,6.00790362057498));
#11122=CARTESIAN_POINT('Ctrl Pts',(1.70423366156926,-1.03664860391784,6.00757896282793));
#11123=CARTESIAN_POINT('Ctrl Pts',(1.70004853827431,-1.04349008966061,6.00706131406208));
#11124=CARTESIAN_POINT('Ctrl Pts',(1.69847399970036,-1.04605098936168,6.00686765633956));
#11125=CARTESIAN_POINT('Ctrl Pts',(1.69546722034032,-1.05091666194025,6.00649993024281));
#11126=CARTESIAN_POINT('Ctrl Pts',(1.69403608376109,-1.05322204334525,6.00632579623812));
#11127=CARTESIAN_POINT('Ctrl Pts',(1.69073469092016,-1.05851603515985,6.00592613158815));
#11128=CARTESIAN_POINT('Ctrl Pts',(1.688861213966,-1.06150261054767,6.00570081641614));
#11129=CARTESIAN_POINT('Ctrl Pts',(1.68287712720233,-1.07098610806003,6.00498579225285));
#11130=CARTESIAN_POINT('Ctrl Pts',(1.67873680853298,-1.07746433871588,6.0044980082182));
#11131=CARTESIAN_POINT('Ctrl Pts',(1.6117139351783,-1.18100879320996,5.99670930202907));
#11132=CARTESIAN_POINT('Ctrl Pts',(1.5405331982177,-1.27246596508619,5.98993339891934));
#11133=CARTESIAN_POINT('Ctrl Pts',(1.39203827205014,-1.43240140596483,5.97724958093508));
#11134=CARTESIAN_POINT('Ctrl Pts',(1.31657262010389,-1.5020585693946,5.97134753588054));
#11135=CARTESIAN_POINT('Ctrl Pts',(1.19402730263821,-1.59881148846721,5.96208572494271));
#11136=CARTESIAN_POINT('Ctrl Pts',(1.15064883809481,-1.63030854400094,5.95886328055533));
#11137=CARTESIAN_POINT('Ctrl Pts',(1.07975006847105,-1.67754781485643,5.95363852429944));
#11138=CARTESIAN_POINT('Ctrl Pts',(1.05303102294477,-1.69444751214884,5.95167866524807));
#11139=CARTESIAN_POINT('Ctrl Pts',(1.01837345362023,-1.71523192659664,5.94914290784695));
#11140=CARTESIAN_POINT('Ctrl Pts',(1.01079429292872,-1.71970926218264,5.94858876091558));
#11141=CARTESIAN_POINT('Ctrl Pts',(0.998555281127256,-1.72683051116412,
5.94769442636926));
#11142=CARTESIAN_POINT('Ctrl Pts',(0.99391392276094,-1.72950610781894,5.94735538930819));
#11143=CARTESIAN_POINT('Ctrl Pts',(0.985060923621533,-1.73456217632846,
5.9467089028518));
#11144=CARTESIAN_POINT('Ctrl Pts',(0.980851284860299,-1.73694609101891,
5.94640158050069));
#11145=CARTESIAN_POINT('Ctrl Pts',(0.971237109139491,-1.74234449418348,
5.94569987388336));
#11146=CARTESIAN_POINT('Ctrl Pts',(0.965827153216209,-1.74534918204492,
5.94530514167649));
#11147=CARTESIAN_POINT('Ctrl Pts',(0.949258326623996,-1.75445087862507,
5.94409653074269));
#11148=CARTESIAN_POINT('Ctrl Pts',(0.938055234607965,-1.76046630770092,
5.94327975810114));
#11149=CARTESIAN_POINT('Ctrl Pts',(0.840544929354676,-1.81162881203009,
5.93617328324466));
#11150=CARTESIAN_POINT('Ctrl Pts',(0.751109280151451,-1.85049841027218,
5.92966293700355));
#11151=CARTESIAN_POINT('Ctrl Pts',(0.525554038086432,-1.92947479610904,
5.91328536835762));
#11152=CARTESIAN_POINT('Ctrl Pts',(0.387310899573127,-1.9619038431194,5.90326336716052));
#11153=CARTESIAN_POINT('Ctrl Pts',(0.206893570312868,-1.98439922626238,
5.89079553690071));
#11154=CARTESIAN_POINT('Ctrl Pts',(0.166838072108192,-1.98816768296259,
5.88806818306347));
#11155=CARTESIAN_POINT('Ctrl Pts',(0.105295543908531,-1.99208437002136,
5.88396548495557));
#11156=CARTESIAN_POINT('Ctrl Pts',(0.0838759409859687,-1.99310115347258,
5.88255381144328));
#11157=CARTESIAN_POINT('Ctrl Pts',(0.0571860680969412,-1.99393705497265,
5.88081840913506));
#11158=CARTESIAN_POINT('Ctrl Pts',(0.0519283722696119,-1.99408090890421,
5.88047768902073));
#11159=CARTESIAN_POINT('Ctrl Pts',(0.0436093249084487,-1.99427559849121,
5.87994045021108));
#11160=CARTESIAN_POINT('Ctrl Pts',(0.0405483666366889,-1.99434018317582,
5.87974317577479));
#11161=CARTESIAN_POINT('Ctrl Pts',(0.0347847264327985,-1.99444851813789,
5.8793724863747));
#11162=CARTESIAN_POINT('Ctrl Pts',(0.0320821370276298,-1.99449382181939,
5.879198989199));
#11163=CARTESIAN_POINT('Ctrl Pts',(0.02588912740067,-1.99458504464769,5.87880214247683));
#11164=CARTESIAN_POINT('Ctrl Pts',(0.0223986785255345,-1.99462729523678,
5.87857900052784));
#11165=CARTESIAN_POINT('Ctrl Pts',(0.0116086709578286,-1.99472957760531,
5.87789077700168));
#11166=CARTESIAN_POINT('Ctrl Pts',(0.00430877727809598,-1.99475870405667,
5.87742739161974));
#11167=CARTESIAN_POINT('Ctrl Pts',(-0.0574059456853493,-1.99466615903818,
5.8735274262474));
#11168=CARTESIAN_POINT('Ctrl Pts',(-0.111800270555511,-1.99235801181298,
5.87020546836019));
#11169=CARTESIAN_POINT('Ctrl Pts',(-0.333123715251099,-1.97387152039378,
5.85691551669195));
#11170=CARTESIAN_POINT('Ctrl Pts',(-0.497789386475864,-1.93890519574217,
5.84750129925474));
#11171=CARTESIAN_POINT('Ctrl Pts',(-0.7046252326072,-1.86685993061634,5.83448494191983));
#11172=CARTESIAN_POINT('Ctrl Pts',(-0.75242932728827,-1.8481104459472,5.83139301507024));
#11173=CARTESIAN_POINT('Ctrl Pts',(-0.82753015280353,-1.81525769025027,
5.82636173799532));
#11174=CARTESIAN_POINT('Ctrl Pts',(-0.855317663129843,-1.8023313156661,
5.82446087641621));
#11175=CARTESIAN_POINT('Ctrl Pts',(-0.890605838408203,-1.78491587097732,
5.82199130850308));
#11176=CARTESIAN_POINT('Ctrl Pts',(-0.898390967220353,-1.78101013248547,
5.82144295189787));
#11177=CARTESIAN_POINT('Ctrl Pts',(-0.910905679881658,-1.77462866537391,
5.82055564037865));
#11178=CARTESIAN_POINT('Ctrl Pts',(-0.915651399804231,-1.77218468866558,
5.82021780205387));
#11179=CARTESIAN_POINT('Ctrl Pts',(-0.924685447948449,-1.76748631018066,
5.81957206063025));
#11180=CARTESIAN_POINT('Ctrl Pts',(-0.928975490992635,-1.76523527349147,
5.81926427807812));
#11181=CARTESIAN_POINT('Ctrl Pts',(-0.938764552515327,-1.76005326826835,
5.81855935272324));
#11182=CARTESIAN_POINT('Ctrl Pts',(-0.944258101465469,-1.75711212748711,
5.81816185118607));
#11183=CARTESIAN_POINT('Ctrl Pts',(-0.961105159534676,-1.74799071293887,
5.81693691282452));
#11184=CARTESIAN_POINT('Ctrl Pts',(-0.972412267543258,-1.7417258765555,
5.81610646916056));
#11185=CARTESIAN_POINT('Ctrl Pts',(-1.07975177043433,-1.68088212742121,
5.80814191946065));
#11186=CARTESIAN_POINT('Ctrl Pts',(-1.17113885925422,-1.6185348036098,5.8007209948428));
#11187=CARTESIAN_POINT('Ctrl Pts',(-1.39056148198761,-1.44048651914965,
5.78124908575034));
#11188=CARTESIAN_POINT('Ctrl Pts',(-1.5096311177695,-1.31517204783432,5.76896716401717));
#11189=CARTESIAN_POINT('Ctrl Pts',(-1.62200127168785,-1.16124036202486,
5.75633143902411));
#11190=CARTESIAN_POINT('Ctrl Pts',(-1.63266265342924,-1.14620243575778,
5.7551207358907));
#11191=CARTESIAN_POINT('Ctrl Pts',(-1.64594760561904,-1.12690239535459,
5.7535989366099));
#11192=CARTESIAN_POINT('Ctrl Pts',(-1.64876526123938,-1.12277586531809,
5.75327539657764));
#11193=CARTESIAN_POINT('Ctrl Pts',(-1.65325141030606,-1.11615247799598,
5.75275907754486));
#11194=CARTESIAN_POINT('Ctrl Pts',(-1.65492979963592,-1.11366239874826,
5.75256563814905));
#11195=CARTESIAN_POINT('Ctrl Pts',(-1.65811370318259,-1.10891562747181,
5.75219818172789));
#11196=CARTESIAN_POINT('Ctrl Pts',(-1.65962021823812,-1.10665968248471,
5.75202409980606));
#11197=CARTESIAN_POINT('Ctrl Pts',(-1.66307633079417,-1.10146136498175,
5.75162423141542));
#11198=CARTESIAN_POINT('Ctrl Pts',(-1.66502272186826,-1.09851688959549,
5.75139866201532));
#11199=CARTESIAN_POINT('Ctrl Pts',(-1.67021088471961,-1.09062283577806,
5.75079635040621));
#11200=CARTESIAN_POINT('Ctrl Pts',(-1.67343849847667,-1.08566392741619,
5.75042053910547));
#11201=CARTESIAN_POINT('Ctrl Pts',(-1.69643246002242,-1.04998980684191,
5.74773465461568));
#11202=CARTESIAN_POINT('Ctrl Pts',(-1.71537543318536,-1.01874884927788,
5.74547618279619));
#11203=CARTESIAN_POINT('Ctrl Pts',(-1.73957576146082,-0.97624635636358,
5.74250236399689));
#11204=CARTESIAN_POINT('Ctrl Pts',(-1.74560028333231,-0.965432774010427,
5.74175409617249));
#11205=CARTESIAN_POINT('Ctrl Pts',(-1.75892721409724,-0.940979256898706,
5.74007907521559));
#11206=CARTESIAN_POINT('Ctrl Pts',(-1.76617242179207,-0.927308957514271,
5.73915448839903));
#11207=CARTESIAN_POINT('Ctrl Pts',(-1.82286021482552,-0.817275045846243,
5.73179549247975));
#11208=CARTESIAN_POINT('Ctrl Pts',(-1.86454090950103,-0.717110462915257,
5.72559352667216));
#11209=CARTESIAN_POINT('Ctrl Pts',(-1.9364905485362,-0.494732056815316,
5.7119848237207));
#11210=CARTESIAN_POINT('Ctrl Pts',(-1.96375246862011,-0.37205501291752,
5.70456309050233));
#11211=CARTESIAN_POINT('Ctrl Pts',(-1.98093268101575,-0.234738892788047,
5.69592602231359));
#11212=CARTESIAN_POINT('Ctrl Pts',(-1.98242070417028,-0.221821489984438,
5.69511063144308));
#11213=CARTESIAN_POINT('Ctrl Pts',(-1.98443584273738,-0.202684227298421,
5.69389799127785));
#11214=CARTESIAN_POINT('Ctrl Pts',(-1.98506024343091,-0.196474778144652,
5.69350380762331));
#11215=CARTESIAN_POINT('Ctrl Pts',(-1.98611713431289,-0.185444645870438,
5.69280228346871));
#11216=CARTESIAN_POINT('Ctrl Pts',(-1.9865612396156,-0.180625104769318,
5.69249531120944));
#11217=CARTESIAN_POINT('Ctrl Pts',(-1.98745671334991,-0.170504202616952,
5.69184972126438));
#11218=CARTESIAN_POINT('Ctrl Pts',(-1.98790441989601,-0.165202563546381,
5.69151099085031));
#11219=CARTESIAN_POINT('Ctrl Pts',(-1.98902458286963,-0.151273449951201,
5.69061955969116));
#11220=CARTESIAN_POINT('Ctrl Pts',(-1.98966211143803,-0.142643353541211,
5.69006576557676));
#11221=CARTESIAN_POINT('Ctrl Pts',(-1.99226996191,-0.103912833767429,5.68757354836504));
#11222=CARTESIAN_POINT('Ctrl Pts',(-1.99361342319119,-0.0737755451558504,
5.68561558193784));
#11223=CARTESIAN_POINT('Ctrl Pts',(-1.99537187113631,0.00661805718719807,
5.68033950854938));
#11224=CARTESIAN_POINT('Ctrl Pts',(-1.99457189737183,0.0568764910081049,
5.67698549523901));
#11225=CARTESIAN_POINT('Ctrl Pts',(-1.9865115335522,0.20685853291375,5.66681389434118));
#11226=CARTESIAN_POINT('Ctrl Pts',(-1.97365340446702,0.306116713493541,
5.65985890814608));
#11227=CARTESIAN_POINT('Ctrl Pts',(-1.92840220335123,0.524923220974854,
5.64426807745429));
#11228=CARTESIAN_POINT('Ctrl Pts',(-1.89221036520727,0.643293764795097,
5.63565180152835));
#11229=CARTESIAN_POINT('Ctrl Pts',(-1.84242786372121,0.76455489259417,5.62709355044145));
#11230=CARTESIAN_POINT('Ctrl Pts',(-1.83951949558784,0.771526180106602,
5.62660257780486));
#11231=CARTESIAN_POINT('Ctrl Pts',(-1.83520622005182,0.781701945461527,
5.62588762401942));
#11232=CARTESIAN_POINT('Ctrl Pts',(-1.83383241346844,0.784919410784791,
5.62566181379824));
#11233=CARTESIAN_POINT('Ctrl Pts',(-1.83138003864552,0.790621307558209,
5.62526210580802));
#11234=CARTESIAN_POINT('Ctrl Pts',(-1.83030486868632,0.793107171775505,
5.62508800300706));
#11235=CARTESIAN_POINT('Ctrl Pts',(-1.82802060912128,0.798359147287296,
5.62472051122588));
#11236=CARTESIAN_POINT('Ctrl Pts',(-1.8268103061763,0.801124697518659,5.62452719827139));
#11237=CARTESIAN_POINT('Ctrl Pts',(-1.82355024617195,0.808528152580744,
5.62401019855294));
#11238=CARTESIAN_POINT('Ctrl Pts',(-1.82148905811442,0.813161045769863,
5.62368720496686));
#11239=CARTESIAN_POINT('Ctrl Pts',(-1.81152010643198,0.835339965892331,
5.6221432648916));
#11240=CARTESIAN_POINT('Ctrl Pts',(-1.80337602822225,0.852779527207339,
5.62093622002811));
#11241=CARTESIAN_POINT('Ctrl Pts',(-1.77994018711997,0.901126743211738,
5.6176020687051));
#11242=CARTESIAN_POINT('Ctrl Pts',(-1.7640970070584,0.931760976963422,5.61550343545838));
#11243=CARTESIAN_POINT('Ctrl Pts',(-1.70343175402551,1.04196234640266,5.60795017858878));
#11244=CARTESIAN_POINT('Ctrl Pts',(-1.65395328902846,1.11884138760937,5.60266975725423));
#11245=CARTESIAN_POINT('Ctrl Pts',(-1.50577979388946,1.3176440410781,5.58829082130289));
#11246=CARTESIAN_POINT('Ctrl Pts',(-1.39773334261183,1.43174396083351,5.57916958180672));
#11247=CARTESIAN_POINT('Ctrl Pts',(-1.26781432937435,1.54007540644937,5.56860584625756));
#11248=CARTESIAN_POINT('Ctrl Pts',(-1.2580887150382,1.54803042763973,5.56781760471203));
#11249=CARTESIAN_POINT('Ctrl Pts',(-1.24348388755124,1.55974784225511,5.56663736881999));
#11250=CARTESIAN_POINT('Ctrl Pts',(-1.23866121644361,1.56358047426879,5.56624819599186));
#11251=CARTESIAN_POINT('Ctrl Pts',(-1.23002062631253,1.57038218682327,5.5655518760555));
#11252=CARTESIAN_POINT('Ctrl Pts',(-1.22620949982333,1.57335984940326,5.56524507391428));
#11253=CARTESIAN_POINT('Ctrl Pts',(-1.21813833384278,1.57961877573058,5.56459599596803));
#11254=CARTESIAN_POINT('Ctrl Pts',(-1.21387578636663,1.58289672795081,5.5642535925637));
#11255=CARTESIAN_POINT('Ctrl Pts',(-1.20253516152739,1.59154506310076,5.56334361166134));
#11256=CARTESIAN_POINT('Ctrl Pts',(-1.19543443150329,1.59688541177246,5.56277486167977));
#11257=CARTESIAN_POINT('Ctrl Pts',(-1.16224158948563,1.62150377362716,5.56012068537297));
#11258=CARTESIAN_POINT('Ctrl Pts',(-1.13571862007832,1.64018993119354,5.55801252110072));
#11259=CARTESIAN_POINT('Ctrl Pts',(-1.06256816321573,1.68910128390786,5.55222805203436));
#11260=CARTESIAN_POINT('Ctrl Pts',(-1.01511720125407,1.71803677821077,5.54850685440975));
#11261=CARTESIAN_POINT('Ctrl Pts',(-0.875385112120838,1.79543397851492,
5.53764413397983));
#11262=CARTESIAN_POINT('Ctrl Pts',(-0.780437447968371,1.83869422144671,
5.5303680973131));
#11263=CARTESIAN_POINT('Ctrl Pts',(-0.611572399718526,1.90018774754922,
5.51783870096188));
#11264=CARTESIAN_POINT('Ctrl Pts',(-0.539173674083609,1.92198531499819,
5.51259214251872));
#11265=CARTESIAN_POINT('Ctrl Pts',(-0.429794959507707,1.94824741977908,
5.50499226884686));
#11266=CARTESIAN_POINT('Ctrl Pts',(-0.393645728192932,1.95587197569543,
5.50253269657453));
#11267=CARTESIAN_POINT('Ctrl Pts',(-0.351452381912605,1.96355395879441,
5.49973784430294));
#11268=CARTESIAN_POINT('Ctrl Pts',(-0.345597025245524,1.96459299198573,
5.49935167914772));
#11269=CARTESIAN_POINT('Ctrl Pts',(-0.336245698468212,1.96620928342696,
5.49873773953017));
#11270=CARTESIAN_POINT('Ctrl Pts',(-0.332752741792645,1.96680342924189,
5.49850903711937));
#11271=CARTESIAN_POINT('Ctrl Pts',(-0.326573498945125,1.96783757503372,
5.49810556661486));
#11272=CARTESIAN_POINT('Ctrl Pts',(-0.323887882895573,1.96828138526332,
5.49793058443278));
#11273=CARTESIAN_POINT('Ctrl Pts',(-0.318225880966407,1.96920515438684,
5.49756246719589));
#11274=CARTESIAN_POINT('Ctrl Pts',(-0.315249324177963,1.96968386176064,
5.49736940377541));
#11275=CARTESIAN_POINT('Ctrl Pts',(-0.307321234758452,1.97094047186723,
5.49685637041444));
#11276=CARTESIAN_POINT('Ctrl Pts',(-0.302367795855993,1.97170646961303,
5.49653706724388));
#11277=CARTESIAN_POINT('Ctrl Pts',(-0.27917130355343,1.97520409404567,5.49504736914465));
#11278=CARTESIAN_POINT('Ctrl Pts',(-0.260893088809021,1.97770136387354,
5.49388963222285));
#11279=CARTESIAN_POINT('Ctrl Pts',(-0.0705787679143973,2.00101860196148,
5.48197768228276));
#11280=CARTESIAN_POINT('Ctrl Pts',(0.10346290506844,1.99959272592379,5.47224164547537));
#11281=CARTESIAN_POINT('Ctrl Pts',(0.382160446189852,1.96077901704428,5.4557602292599));
#11282=CARTESIAN_POINT('Ctrl Pts',(0.487768397941316,1.93720882792712,5.44930870388769));
#11283=CARTESIAN_POINT('Ctrl Pts',(0.603264906900256,1.90138515958882,5.44175975933388));
#11284=CARTESIAN_POINT('Ctrl Pts',(0.615551939787139,1.89744298201715,5.44095043083739));
#11285=CARTESIAN_POINT('Ctrl Pts',(0.633717973541987,1.89141956481533,5.43974423864212));
#11286=CARTESIAN_POINT('Ctrl Pts',(0.639627023229914,1.88942946676524,5.43935036908409));
#11287=CARTESIAN_POINT('Ctrl Pts',(0.65011984886831,1.88584074369298,5.43864821945197));
#11288=CARTESIAN_POINT('Ctrl Pts',(0.654707322726424,1.88425302158516,5.43834030120745));
#11289=CARTESIAN_POINT('Ctrl Pts',(0.664343589367101,1.88087847579217,5.43769150455605));
#11290=CARTESIAN_POINT('Ctrl Pts',(0.669391066148478,1.87908803547684,5.43735050840611));
#11291=CARTESIAN_POINT('Ctrl Pts',(0.682669996322445,1.87431744287109,5.43645033017658));
#11292=CARTESIAN_POINT('Ctrl Pts',(0.690889076515815,1.87130341752442,5.43589002667382));
#11293=CARTESIAN_POINT('Ctrl Pts',(0.728088131141798,1.85738364583677,5.43333966573404));
#11294=CARTESIAN_POINT('Ctrl Pts',(0.756830266421681,1.8458586358357,5.4313290387166));
#11295=CARTESIAN_POINT('Ctrl Pts',(0.833110702010663,1.81319061908548,5.42588104560036));
#11296=CARTESIAN_POINT('Ctrl Pts',(0.880106935472394,1.79085026163924,5.42240501771151));
#11297=CARTESIAN_POINT('Ctrl Pts',(1.01590787719392,1.71965811697747,5.41200705733227));
#11298=CARTESIAN_POINT('Ctrl Pts',(1.10192098641263,1.66585104109242,5.40494875447953));
#11299=CARTESIAN_POINT('Ctrl Pts',(1.27978105537475,1.53476486151793,5.38953352226989));
#11300=CARTESIAN_POINT('Ctrl Pts',(1.36952528585145,1.45524925078667,5.38120156160177));
#11301=CARTESIAN_POINT('Ctrl Pts',(1.4563208046089,1.36315974014363,5.37293880354485));
#11302=CARTESIAN_POINT('Ctrl Pts',(1.46100720748692,1.35813574655702,5.37249201682164));
#11303=CARTESIAN_POINT('Ctrl Pts',(1.46801666512753,1.35054308544168,5.37182291036847));
#11304=CARTESIAN_POINT('Ctrl Pts',(1.47035908023618,1.34799248155751,5.37159916502835));
#11305=CARTESIAN_POINT('Ctrl Pts',(1.47440298705309,1.34356607864765,5.3712126653243));
#11306=CARTESIAN_POINT('Ctrl Pts',(1.47610756099954,1.34169312603902,5.37104967820269));
#11307=CARTESIAN_POINT('Ctrl Pts',(1.47965736587697,1.33777771639469,5.37071011568917));
#11308=CARTESIAN_POINT('Ctrl Pts',(1.48150191182836,1.33573471326586,5.37053359575939));
#11309=CARTESIAN_POINT('Ctrl Pts',(1.48594598782051,1.33079196323776,5.37010810759617));
#11310=CARTESIAN_POINT('Ctrl Pts',(1.48854125963519,1.32788841667238,5.36985946312305));
#11311=CARTESIAN_POINT('Ctrl Pts',(1.49755825512467,1.31774069925689,5.36899491600126));
#11312=CARTESIAN_POINT('Ctrl Pts',(1.50393586374513,1.31045725029181,5.36838226164647));
#11313=CARTESIAN_POINT('Ctrl Pts',(1.58871287782516,1.21220488086934,5.36021786304469));
#11314=CARTESIAN_POINT('Ctrl Pts',(1.65880757784344,1.11436793531017,5.35322296340594));
#11315=CARTESIAN_POINT('Ctrl Pts',(1.80218643627317,0.870437635295791,5.33681810773762));
#11316=CARTESIAN_POINT('Ctrl Pts',(1.86718634175054,0.720517499326425,5.3274514031093));
#11317=CARTESIAN_POINT('Ctrl Pts',(1.91918146435512,0.544251907777537,5.31608306181147));
#11318=CARTESIAN_POINT('Ctrl Pts',(1.92479874774447,0.524039464253312,5.31477555087322));
#11319=CARTESIAN_POINT('Ctrl Pts',(1.93206145943059,0.496212303706111,5.31296865518706));
#11320=CARTESIAN_POINT('Ctrl Pts',(1.93398275399293,0.488670479801494,5.31247826591798));
#11321=CARTESIAN_POINT('Ctrl Pts',(1.93696840268202,0.476657208407773,5.31169598204464));
#11322=CARTESIAN_POINT('Ctrl Pts',(1.93806153561012,0.47219293823856,5.31140502477862));
#11323=CARTESIAN_POINT('Ctrl Pts',(1.94026996437983,0.463037021388265,5.31080775817177));
#11324=CARTESIAN_POINT('Ctrl Pts',(1.94138369444478,0.458345031737235,5.31050140023966));
#11325=CARTESIAN_POINT('Ctrl Pts',(1.94391282647574,0.447515539170537,5.30979362066193));
#11326=CARTESIAN_POINT('Ctrl Pts',(1.9453161887259,0.441375304135935,5.30939181219178));
#11327=CARTESIAN_POINT('Ctrl Pts',(1.94961948984479,0.422127498653317,5.30813062931188));
#11328=CARTESIAN_POINT('Ctrl Pts',(1.95241615617427,0.408997455557157,5.30726793375808));
#11329=CARTESIAN_POINT('Ctrl Pts',(1.97852886095199,0.280025220012113,5.29876928998424));
#11330=CARTESIAN_POINT('Ctrl Pts',(1.9916362901664,0.162377204889784,5.29080067566583));
#11331=CARTESIAN_POINT('Ctrl Pts',(1.99800674982891,-0.124534297934065,
5.27095624988362));
#11332=CARTESIAN_POINT('Ctrl Pts',(1.98030586717885,-0.293141627222418,
5.25892010931736));
#11333=CARTESIAN_POINT('Ctrl Pts',(1.93840789848359,-0.470949176563014,
5.24687145907564));
#11334=CARTESIAN_POINT('Ctrl Pts',(1.93510062495414,-0.484359272753008,
5.24596728793283));
#11335=CARTESIAN_POINT('Ctrl Pts',(1.93051728763558,-0.502146717549188,
5.24477499731521));
#11336=CARTESIAN_POINT('Ctrl Pts',(1.92936522179259,-0.506555195162452,
5.24448007376748));
#11337=CARTESIAN_POINT('Ctrl Pts',(1.9274611372099,-0.513740599195335,5.24400036109387));
#11338=CARTESIAN_POINT('Ctrl Pts',(1.92671820698699,-0.516519883296295,
5.24381505114184));
#11339=CARTESIAN_POINT('Ctrl Pts',(1.92527391553418,-0.521876467056921,
5.24345837663292));
#11340=CARTESIAN_POINT('Ctrl Pts',(1.92457338752335,-0.524453975952867,
5.24328696443752));
#11341=CARTESIAN_POINT('Ctrl Pts',(1.92292667021037,-0.530465143650162,
5.2428876873275));
#11342=CARTESIAN_POINT('Ctrl Pts',(1.92197645257756,-0.533897709164933,
5.24266005640868));
#11343=CARTESIAN_POINT('Ctrl Pts',(1.91888779659482,-0.544940058709323,
5.24192891573797));
#11344=CARTESIAN_POINT('Ctrl Pts',(1.9167132845712,-0.552539802410515,5.24142745428522));
#11345=CARTESIAN_POINT('Ctrl Pts',(1.91151335971188,-0.570312969131404,
5.24025834960125));
#11346=CARTESIAN_POINT('Ctrl Pts',(1.90845178423322,-0.580475671742746,
5.23959266082213));
#11347=CARTESIAN_POINT('Ctrl Pts',(1.87068735171775,-0.702303050702932,
5.2316410010785));
#11348=CARTESIAN_POINT('Ctrl Pts',(1.82630652852721,-0.810748357969191,
5.22484274320764));
#11349=CARTESIAN_POINT('Ctrl Pts',(1.70020098125594,-1.05514084716902,5.20888758195758));
#11350=CARTESIAN_POINT('Ctrl Pts',(1.61130655733755,-1.18646086427432,5.19975982712934));
#11351=CARTESIAN_POINT('Ctrl Pts',(1.49392963985225,-1.32198872595641,5.18866484035132));
#11352=CARTESIAN_POINT('Ctrl Pts',(1.47974913353996,-1.33784244504943,5.18733865547572));
#11353=CARTESIAN_POINT('Ctrl Pts',(1.45996548697671,-1.35926103996997,5.18550606602541));
#11354=CARTESIAN_POINT('Ctrl Pts',(1.45457845909306,-1.36502428601496,5.18500879675367));
#11355=CARTESIAN_POINT('Ctrl Pts',(1.44595760576161,-1.37413821996671,5.1842156901674));
#11356=CARTESIAN_POINT('Ctrl Pts',(1.44274595093105,-1.37750984232699,5.18392080436705));
#11357=CARTESIAN_POINT('Ctrl Pts',(1.43614150503355,-1.38439481166425,5.18331557104669));
#11358=CARTESIAN_POINT('Ctrl Pts',(1.43274755925192,-1.38790700257863,5.18300517469529));
#11359=CARTESIAN_POINT('Ctrl Pts',(1.42489262242761,-1.39597608959126,5.18228820973392));
#11360=CARTESIAN_POINT('Ctrl Pts',(1.42042262837544,-1.4005241102549,5.18188125028765));
#11361=CARTESIAN_POINT('Ctrl Pts',(1.40636206078448,-1.41469355945827,5.18060432756427));
#11362=CARTESIAN_POINT('Ctrl Pts',(1.39669511952127,-1.42423833721886,5.17973101045326));
#11363=CARTESIAN_POINT('Ctrl Pts',(1.30073769388706,-1.51706663215664,5.17110534393398));
#11364=CARTESIAN_POINT('Ctrl Pts',(1.20721596881097,-1.5924917593615,5.16301494691285));
#11365=CARTESIAN_POINT('Ctrl Pts',(1.03649139783089,-1.70645929303209,5.14882714055206));
#11366=CARTESIAN_POINT('Ctrl Pts',(0.962508099534142,-1.7492556571168,5.14284667789002));
#11367=CARTESIAN_POINT('Ctrl Pts',(0.806752962026177,-1.82647295016002,
5.13078516638235));
#11368=CARTESIAN_POINT('Ctrl Pts',(0.724955751690994,-1.86045610765889,
5.12472186470645));
#11369=CARTESIAN_POINT('Ctrl Pts',(0.633851438582407,-1.89138032493641,
5.11843943049738));
#11370=CARTESIAN_POINT('Ctrl Pts',(0.626525452757398,-1.89381969613309,
5.11793748685206));
#11371=CARTESIAN_POINT('Ctrl Pts',(0.615744047215548,-1.89734022675981,
5.11720374107812));
#11372=CARTESIAN_POINT('Ctrl Pts',(0.612299663329723,-1.89845457953319,
5.11697006703781));
#11373=CARTESIAN_POINT('Ctrl Pts',(0.606254466106184,-1.90039220333834,
5.11656126657632));
#11374=CARTESIAN_POINT('Ctrl Pts',(0.603655021873108,-1.90121950833504,
5.11638591013217));
#11375=CARTESIAN_POINT('Ctrl Pts',(0.601037949391743,-1.90204651524843,
5.11620979154589));
#11376=CARTESIAN_POINT('Ctrl Pts',(0.601022058580757,-1.9020515365986,5.1162087221732));
#11377=CARTESIAN_POINT('Ctrl Pts',(0.600990694950365,-1.90206144678514,
5.11620661158774));
#11378=CARTESIAN_POINT('Ctrl Pts',(0.60097522218867,-1.90206633561466,5.11620557037802));
#11379=CARTESIAN_POINT('Ctrl Pts',(0.600944682111629,-1.90207598475756,
5.11620351527187));
#11380=CARTESIAN_POINT('Ctrl Pts',(0.600929614755258,-1.90208074509464,
5.11620250137189));
#11381=CARTESIAN_POINT('Ctrl Pts',(0.600899873110135,-1.90209014119548,
5.11620050004993));
#11382=CARTESIAN_POINT('Ctrl Pts',(0.600885198870916,-1.90209477695374,
5.11619951263054));
#11383=CARTESIAN_POINT('Ctrl Pts',(0.60085623164982,-1.90210392765807,5.11619756347288));
#11384=CARTESIAN_POINT('Ctrl Pts',(0.600841938685225,-1.90210844260827,
5.11619660173507));
#11385=CARTESIAN_POINT('Ctrl Pts',(0.600813722868489,-1.90211735524549,
5.1161947031886));
#11386=CARTESIAN_POINT('Ctrl Pts',(0.60079979989473,-1.90212175297998,5.1161937663711));
#11387=CARTESIAN_POINT('Ctrl Pts',(0.600772312851441,-1.90213043475296,
5.11619191690914));
#11388=CARTESIAN_POINT('Ctrl Pts',(0.600758748826103,-1.90213471878604,
5.11619100426704));
#11389=CARTESIAN_POINT('Ctrl Pts',(0.600731969096899,-1.90214317652406,
5.116189202442));
#11390=CARTESIAN_POINT('Ctrl Pts',(0.600718753420697,-1.90214735022836,
5.11618831326034));
#11391=CARTESIAN_POINT('Ctrl Pts',(0.600692660210878,-1.90215559054751,
5.11618655766958));
#11392=CARTESIAN_POINT('Ctrl Pts',(0.600679782674728,-1.90215965717082,
5.11618569125976));
#11393=CARTESIAN_POINT('Ctrl Pts',(0.600654355845628,-1.90216768647689,
5.11618398054502));
#11394=CARTESIAN_POINT('Ctrl Pts',(0.600641806564661,-1.90217164916312,
5.11618313624037));
#11395=CARTESIAN_POINT('Ctrl Pts',(0.600617026788357,-1.90217947360295,
5.11618146909812));
#11396=CARTESIAN_POINT('Ctrl Pts',(0.600604796270744,-1.90218333537046,
5.11618064625853));
#11397=CARTESIAN_POINT('Ctrl Pts',(0.60058064469499,-1.90219096093795,5.11617902141746));
#11398=CARTESIAN_POINT('Ctrl Pts',(0.600568723688315,-1.90219472472817,
5.11617821941899));
#11399=CARTESIAN_POINT('Ctrl Pts',(0.600545182366988,-1.90220215712849,
5.11617663566894));
#11400=CARTESIAN_POINT('Ctrl Pts',(0.600533562023444,-1.90220582575386,
5.11617585391498));
#11401=CARTESIAN_POINT('Ctrl Pts',(0.600510613391981,-1.90221307056931,
5.11617431007164));
#11402=CARTESIAN_POINT('Ctrl Pts',(0.60049928511379,-1.90221664676213,5.11617354798249));
#11403=CARTESIAN_POINT('Ctrl Pts',(0.6004769123105,-1.90222370935077,5.11617204290899));
#11404=CARTESIAN_POINT('Ctrl Pts',(0.600465867800263,-1.9022271957474,5.11617129992523));
#11405=CARTESIAN_POINT('Ctrl Pts',(0.600445699975258,-1.90223356188791,
5.11616994321385));
#11406=CARTESIAN_POINT('Ctrl Pts',(0.600436576677637,-1.90223644166018,
5.11616932948501));
#11407=CARTESIAN_POINT('Ctrl Pts',(0.600418357611893,-1.90224219237026,
5.11616810388953));
#11408=CARTESIAN_POINT('Ctrl Pts',(0.600409282098518,-1.9022450569159,5.11616749338542));
#11409=CARTESIAN_POINT('Ctrl Pts',(0.600391183907054,-1.90225076918808,
5.11616627594166));
#11410=CARTESIAN_POINT('Ctrl Pts',(0.600382162085712,-1.90225361664507,
5.11616566905957));
#11411=CARTESIAN_POINT('Ctrl Pts',(0.600364171034225,-1.90225929481953,
5.11616445884324));
#11412=CARTESIAN_POINT('Ctrl Pts',(0.600355202502612,-1.90226212531738,
5.11616385555593));
#11413=CARTESIAN_POINT('Ctrl Pts',(0.600337317392383,-1.90226776977743,
5.11616265248605));
#11414=CARTESIAN_POINT('Ctrl Pts',(0.600328401643277,-1.90227058347869,
5.11616205275922));
#11415=CARTESIAN_POINT('Ctrl Pts',(0.600310621472889,-1.90227619454529,
5.11616085676806));
#11416=CARTESIAN_POINT('Ctrl Pts',(0.600301757969406,-1.90227899162183,
5.11616026056541));
#11417=CARTESIAN_POINT('Ctrl Pts',(0.600284081898186,-1.90228456956512,
5.11615907159608));
#11418=CARTESIAN_POINT('Ctrl Pts',(0.600275270187719,-1.90228735016216,
5.11615847888701));
#11419=CARTESIAN_POINT('Ctrl Pts',(0.600257697194919,-1.90229289530902,
5.1161572968705));
#11420=CARTESIAN_POINT('Ctrl Pts',(0.60024893679643,-1.90229565958073,5.11615670762247));
#11421=CARTESIAN_POINT('Ctrl Pts',(0.60023146591235,-1.90230117224184,5.11615553249323));
#11422=CARTESIAN_POINT('Ctrl Pts',(0.600222756322408,-1.90230392034941,
5.11615494667221));
#11423=CARTESIAN_POINT('Ctrl Pts',(0.600205386767657,-1.9023094007753,5.11615377837747));
#11424=CARTESIAN_POINT('Ctrl Pts',(0.600196727611904,-1.90231213283914,
5.11615319595811));
#11425=CARTESIAN_POINT('Ctrl Pts',(0.600179458215574,-1.90231758140383,
5.11615203441879));
#11426=CARTESIAN_POINT('Ctrl Pts',(0.600170848970063,-1.90232029759151,
5.1161514553657));
#11427=CARTESIAN_POINT('Ctrl Pts',(0.600153678969677,-1.90232571454005,
5.11615030053019));
#11428=CARTESIAN_POINT('Ctrl Pts',(0.600145119203757,-1.90232841498967,
5.11614972481423));
#11429=CARTESIAN_POINT('Ctrl Pts',(0.600128047579786,-1.90233380064812,
5.11614857661364));
#11430=CARTESIAN_POINT('Ctrl Pts',(0.600119536776585,-1.90233648552493,
5.1161480041999));
#11431=CARTESIAN_POINT('Ctrl Pts',(0.600102562850611,-1.90234184011168,
5.11614686258828));
#11432=CARTESIAN_POINT('Ctrl Pts',(0.600094100646314,-1.90234450953262,
5.11614629345213));
#11433=CARTESIAN_POINT('Ctrl Pts',(0.6000772233725,-1.90234983338188,5.11614515835884));
#11434=CARTESIAN_POINT('Ctrl Pts',(0.600068809326611,-1.90235248748803,
5.11614459247049));
#11435=CARTESIAN_POINT('Ctrl Pts',(0.600052027743847,-1.90235778090719,
5.11614346383058));
#11436=CARTESIAN_POINT('Ctrl Pts',(0.600043661332126,-1.90236041986602,
5.11614290115464));
#11437=CARTESIAN_POINT('Ctrl Pts',(0.600026974885705,-1.90236568303423,
5.1161417789305));
#11438=CARTESIAN_POINT('Ctrl Pts',(0.600018655807818,-1.90236830694254,
5.11614121944661));
#11439=CARTESIAN_POINT('Ctrl Pts',(0.600002063280902,-1.90237354024771,
5.11614010355611));
#11440=CARTESIAN_POINT('Ctrl Pts',(0.599993791007381,-1.90237614927453,
5.11613954722852));
#11441=CARTESIAN_POINT('Ctrl Pts',(0.599977291810429,-1.90238135290666,
5.11613843763172));
#11442=CARTESIAN_POINT('Ctrl Pts',(0.599969065966349,-1.90238394717224,
5.11613788443506));
#11443=CARTESIAN_POINT('Ctrl Pts',(0.599952659172731,-1.90238912142755,
5.11613678106935));
#11444=CARTESIAN_POINT('Ctrl Pts',(0.599944479340818,-1.90239170106549,
5.11613623097543));
#11445=CARTESIAN_POINT('Ctrl Pts',(0.59992816411756,-1.90239684621061,5.11613513378452));
#11446=CARTESIAN_POINT('Ctrl Pts',(0.599920029875086,-1.90239941135615,
5.11613458676476));
#11447=CARTESIAN_POINT('Ctrl Pts',(0.599903805442814,-1.90240452764074,
5.11613349569595));
#11448=CARTESIAN_POINT('Ctrl Pts',(0.599895716395943,-1.90240707842002,
5.11613295172373));
#11449=CARTESIAN_POINT('Ctrl Pts',(0.599879581920754,-1.90241216611084,
5.11613186672067));
#11450=CARTESIAN_POINT('Ctrl Pts',(0.599871537665024,-1.90241470265329,
5.11613132576865));
#11451=CARTESIAN_POINT('Ctrl Pts',(0.599855492353792,-1.90241976200422,
5.11613024677773));
#11452=CARTESIAN_POINT('Ctrl Pts',(0.599847492490544,-1.90242228443741,
5.11612970881897));
#11453=CARTESIAN_POINT('Ctrl Pts',(0.599831519207564,-1.90242732085509,
5.11612863468762));
#11454=CARTESIAN_POINT('Ctrl Pts',(0.59982354691347,-1.90242983448462,5.1161280985906));
#11455=CARTESIAN_POINT('Ctrl Pts',(0.599807709929055,-1.90243482770856,
5.11612703364043));
#11456=CARTESIAN_POINT('Ctrl Pts',(0.599799797274981,-1.90243732242556,
5.11612650156182));
#11457=CARTESIAN_POINT('Ctrl Pts',(0.599784015155897,-1.90244229813457,
5.1161254403166));
#11458=CARTESIAN_POINT('Ctrl Pts',(0.599776145716583,-1.90244477911908,
5.11612491115167));
#11459=CARTESIAN_POINT('Ctrl Pts',(0.599760449674114,-1.90244972747614,
5.11612385570993));
#11460=CARTESIAN_POINT('Ctrl Pts',(0.599752623068072,-1.90245219485019,
5.11612332943289));
#11461=CARTESIAN_POINT('Ctrl Pts',(0.596769037986115,-1.90339276371807,
5.11592270850813));
#11462=CARTESIAN_POINT('Ctrl Pts',(0.593791058305956,-1.9043238897484,5.11572301614141));
#11463=CARTESIAN_POINT('Ctrl Pts',(0.585581761738283,-1.90686956446533,
5.11517401788902));
#11464=CARTESIAN_POINT('Ctrl Pts',(0.580345916025022,-1.90846958450192,
5.11482553044147));
#11465=CARTESIAN_POINT('Ctrl Pts',(0.553245875734745,-1.91662923651127,
5.1130300607523));
#11466=CARTESIAN_POINT('Ctrl Pts',(0.531275809044089,-1.92283508105358,
5.11160219131275));
#11467=CARTESIAN_POINT('Ctrl Pts',(0.4668949383013,-1.93983283296633,5.1074854205176));
#11468=CARTESIAN_POINT('Ctrl Pts',(0.424227876943702,-1.94960855766813,
5.10484156992936));
#11469=CARTESIAN_POINT('Ctrl Pts',(0.255799354590592,-1.98240620660087,
5.09461338342289));
#11470=CARTESIAN_POINT('Ctrl Pts',(0.128266004044852,-1.99472262025498,
5.0873011150277));
#11471=CARTESIAN_POINT('Ctrl Pts',(-0.0970385373153938,-1.99477079400317,
5.07401678910656));
#11472=CARTESIAN_POINT('Ctrl Pts',(-0.194361689752754,-1.98764856573406,
5.06816093898525));
#11473=CARTESIAN_POINT('Ctrl Pts',(-0.303437260793348,-1.97157739253857,
5.06127508079671));
#11474=CARTESIAN_POINT('Ctrl Pts',(-0.316089124841791,-1.96958859644474,
5.06047156146571));
#11475=CARTESIAN_POINT('Ctrl Pts',(-0.334904997509748,-1.96644489316413,
5.05926903272429));
#11476=CARTESIAN_POINT('Ctrl Pts',(-0.341084297102048,-1.96538250120667,
5.0588728979646));
#11477=CARTESIAN_POINT('Ctrl Pts',(-0.352102615806268,-1.96343462075366,
5.05816433847337));
#11478=CARTESIAN_POINT('Ctrl Pts',(-0.356943582300218,-1.96256032783435,
5.05785226520953));
#11479=CARTESIAN_POINT('Ctrl Pts',(-0.367156895998506,-1.96067673441863,
5.05719222777742));
#11480=CARTESIAN_POINT('Ctrl Pts',(-0.372528419594711,-1.95966324117194,
5.05684413480996));
#11481=CARTESIAN_POINT('Ctrl Pts',(-0.386758480432933,-1.95691770747346,
5.0559194023487));
#11482=CARTESIAN_POINT('Ctrl Pts',(-0.395609464360333,-1.95514761165191,
5.05534157407363));
#11483=CARTESIAN_POINT('Ctrl Pts',(-0.436684424850211,-1.94664275471185,
5.05264743723274));
#11484=CARTESIAN_POINT('Ctrl Pts',(-0.468748965751537,-1.93917134262347,
5.05050807205476));
#11485=CARTESIAN_POINT('Ctrl Pts',(-0.555096263771183,-1.91678473440005,
5.04464375120731));
#11486=CARTESIAN_POINT('Ctrl Pts',(-0.608953148288937,-1.90036066774255,
5.04087326678573));
#11487=CARTESIAN_POINT('Ctrl Pts',(-0.830828305511239,-1.82229748065257,
5.02487353074236));
#11488=CARTESIAN_POINT('Ctrl Pts',(-0.990790867277254,-1.74049751837718,
5.01210349646804));
#11489=CARTESIAN_POINT('Ctrl Pts',(-1.13766281679009,-1.63852094212837,
5.));
#11490=CARTESIAN_POINT('',(1.16034898466907,-1.62253437445173,5.));
#11491=CARTESIAN_POINT('Origin',(0.,0.,5.));
#11492=CARTESIAN_POINT('',(-1.99474961218969,0.00124385252382927,5.52095488142951));
#11493=CARTESIAN_POINT('Ctrl Pts',(1.16034898466907,-1.62253437445173,5.00000000000001));
#11494=CARTESIAN_POINT('Ctrl Pts',(1.21844063257987,-1.58099036420922,5.00455858344228));
#11495=CARTESIAN_POINT('Ctrl Pts',(1.2743420855766,-1.53629197585398,5.00911716688455));
#11496=CARTESIAN_POINT('Ctrl Pts',(1.32770815537402,-1.48869695259086,5.01367575032681));
#11497=CARTESIAN_POINT('Ctrl Pts',(1.38306156050821,-1.43932950591443,5.01840409395556));
#11498=CARTESIAN_POINT('Ctrl Pts',(1.43568659918061,-1.38684571252913,5.02313243758431));
#11499=CARTESIAN_POINT('Ctrl Pts',(1.48523547325909,-1.33157919459296,5.02786078121306));
#11500=CARTESIAN_POINT('Ctrl Pts',(1.53297087618727,-1.27833541153662,5.03241606914843));
#11501=CARTESIAN_POINT('Ctrl Pts',(1.57785107762913,-1.22250944870469,5.03697135708381));
#11502=CARTESIAN_POINT('Ctrl Pts',(1.61960376883367,-1.16443599844722,5.04152664501918));
#11503=CARTESIAN_POINT('Ctrl Pts',(1.66135728082582,-1.1063614065635,5.04608202250385));
#11504=CARTESIAN_POINT('Ctrl Pts',(1.6999828936299,-1.04603961018101,5.05063739998851));
#11505=CARTESIAN_POINT('Ctrl Pts',(1.73525066685647,-0.983835700548712,
5.05519277747318));
#11506=CARTESIAN_POINT('Ctrl Pts',(1.77052858039765,-0.921613905828823,
5.05974946473605));
#11507=CARTESIAN_POINT('Ctrl Pts',(1.80244651005969,-0.857509319488621,
5.06430615199893));
#11508=CARTESIAN_POINT('Ctrl Pts',(1.83082032737691,-0.79191192146824,5.0688628392618));
#11509=CARTESIAN_POINT('Ctrl Pts',(1.85920990629121,-0.726278084228345,
5.07342205775507));
#11510=CARTESIAN_POINT('Ctrl Pts',(1.88405127804513,-0.659150205705004,
5.07798127624833));
#11511=CARTESIAN_POINT('Ctrl Pts',(1.90520884064975,-0.590937252176608,
5.0825404947416));
#11512=CARTESIAN_POINT('Ctrl Pts',(1.92639922177238,-0.522618490238898,
5.08710678525904));
#11513=CARTESIAN_POINT('Ctrl Pts',(1.94389425381641,-0.453211730812403,
5.09167307577648));
#11514=CARTESIAN_POINT('Ctrl Pts',(1.95760863540901,-0.383139652179284,
5.09623936629392));
#11515=CARTESIAN_POINT('Ctrl Pts',(1.97133530670789,-0.313004780684608,
5.10080974874718));
#11516=CARTESIAN_POINT('Ctrl Pts',(1.98127451558112,-0.242203854129323,
5.10538013120044));
#11517=CARTESIAN_POINT('Ctrl Pts',(1.98739272978761,-0.171165709437767,
5.10995051365369));
#11518=CARTESIAN_POINT('Ctrl Pts',(1.99352228814312,-0.0999958486486999,
5.114529370328));
#11519=CARTESIAN_POINT('Ctrl Pts',(1.99581669271177,-0.0285883473734132,
5.1191082270023));
#11520=CARTESIAN_POINT('Ctrl Pts',(1.99429447824322,0.0426274154575889,
5.12368708367661));
#11521=CARTESIAN_POINT('Ctrl Pts',(1.9939100714607,0.0606116238725119,5.12484338825665));
#11522=CARTESIAN_POINT('Ctrl Pts',(1.99328252909201,0.0785836332191591,
5.12599969283669));
#11523=CARTESIAN_POINT('Ctrl Pts',(1.99241266991592,0.0965366006161332,
5.12715599741674));
#11524=CARTESIAN_POINT('Ctrl Pts',(1.98909632330557,0.16498246427945,5.13156441992923));
#11525=CARTESIAN_POINT('Ctrl Pts',(1.98224070223774,0.233421908887211,5.13597284244173));
#11526=CARTESIAN_POINT('Ctrl Pts',(1.97184014003056,0.301453188180601,5.14038126495422));
#11527=CARTESIAN_POINT('Ctrl Pts',(1.96145700103407,0.369370500239447,5.14478230239726));
#11528=CARTESIAN_POINT('Ctrl Pts',(1.94754077282591,0.4368805132556,5.14918333984031));
#11529=CARTESIAN_POINT('Ctrl Pts',(1.93013775644399,0.503582966003958,5.15358437728335));
#11530=CARTESIAN_POINT('Ctrl Pts',(1.9127587100587,0.570193546312947,5.1579793529696));
#11531=CARTESIAN_POINT('Ctrl Pts',(1.89190253429834,0.635998292760284,5.16237432865586));
#11532=CARTESIAN_POINT('Ctrl Pts',(1.86766684366622,0.700605540636004,5.16676930434212));
#11533=CARTESIAN_POINT('Ctrl Pts',(1.84344930507931,0.76516439898147,5.17116098827991));
#11534=CARTESIAN_POINT('Ctrl Pts',(1.81585744398091,0.828527069005353,5.1755526722177));
#11535=CARTESIAN_POINT('Ctrl Pts',(1.78503868383535,0.890317055723046,5.1799443561555));
#11536=CARTESIAN_POINT('Ctrl Pts',(1.7542319931214,0.952082843867704,5.18433432019513));
#11537=CARTESIAN_POINT('Ctrl Pts',(1.72020113315709,1.01227672231106,5.18872428423476));
#11538=CARTESIAN_POINT('Ctrl Pts',(1.68314085352376,1.07054398774609,5.19311424827439));
#11539=CARTESIAN_POINT('Ctrl Pts',(1.64608184473292,1.12880925512505,5.19750406177677));
#11540=CARTESIAN_POINT('Ctrl Pts',(1.60599389321954,1.18514761905863,5.20189387527914));
#11541=CARTESIAN_POINT('Ctrl Pts',(1.56311569278322,1.23923238074012,5.20628368878152));
#11542=CARTESIAN_POINT('Ctrl Pts',(1.52019395217665,1.29337206216423,5.21067795986899));
#11543=CARTESIAN_POINT('Ctrl Pts',(1.47447661880384,1.34525317987349,5.21507223095646));
#11544=CARTESIAN_POINT('Ctrl Pts',(1.42624270807061,1.39458212385481,5.21946650204393));
#11545=CARTESIAN_POINT('Ctrl Pts',(1.37798275764808,1.44393769869305,5.22386314543446));
#11546=CARTESIAN_POINT('Ctrl Pts',(1.32720389605377,1.49073801954655,5.22825978882499));
#11547=CARTESIAN_POINT('Ctrl Pts',(1.27421986522253,1.53472841166516,5.23265643221552));
#11548=CARTESIAN_POINT('Ctrl Pts',(1.22114023463785,1.57879817620174,5.23706100852503));
#11549=CARTESIAN_POINT('Ctrl Pts',(1.16584789491828,1.62004759307619,5.24146558483455));
#11550=CARTESIAN_POINT('Ctrl Pts',(1.10868660112007,1.65826462996617,5.24587016114406));
#11551=CARTESIAN_POINT('Ctrl Pts',(1.0721680575412,1.68268028668746,5.2486841057072));
#11552=CARTESIAN_POINT('Ctrl Pts',(1.03488724876347,1.70585917353192,5.25149805027034));
#11553=CARTESIAN_POINT('Ctrl Pts',(0.996938583639457,1.72775606581223,5.25431199483347));
#11554=CARTESIAN_POINT('Ctrl Pts',(0.936781371479421,1.76246758966287,5.25877273303172));
#11555=CARTESIAN_POINT('Ctrl Pts',(0.874692054691213,1.79410108641791,5.26323347122997));
#11556=CARTESIAN_POINT('Ctrl Pts',(0.81101789861186,1.82243725012172,5.26769420942822));
#11557=CARTESIAN_POINT('Ctrl Pts',(0.747439221880839,1.85073092376972,5.27214825875296));
#11558=CARTESIAN_POINT('Ctrl Pts',(0.682280865182101,1.87573688187796,5.27660230807769));
#11559=CARTESIAN_POINT('Ctrl Pts',(0.615915837290236,1.89728101341764,5.28105635740243));
#11560=CARTESIAN_POINT('Ctrl Pts',(0.549629308337894,1.91879966178444,5.28550513831758));
#11561=CARTESIAN_POINT('Ctrl Pts',(0.482139405117496,1.93686446734296,5.28995391923274));
#11562=CARTESIAN_POINT('Ctrl Pts',(0.413838670673521,1.95134956303456,5.2944027001479));
#11563=CARTESIAN_POINT('Ctrl Pts',(0.345581263020212,1.9658254700591,5.29884865896457));
#11564=CARTESIAN_POINT('Ctrl Pts',(0.276514520753651,1.97672607152122,5.30329461778123));
#11565=CARTESIAN_POINT('Ctrl Pts',(0.20704423956589,1.98397586814018,5.3077405765979));
#11566=CARTESIAN_POINT('Ctrl Pts',(0.137594622853645,1.99122350825075,5.31218521292953));
#11567=CARTESIAN_POINT('Ctrl Pts',(0.0677421904907084,1.99482244894574,
5.31662984926117));
#11568=CARTESIAN_POINT('Ctrl Pts',(-0.00210077107298254,1.99474889378611,
5.32107448559281));
#11569=CARTESIAN_POINT('Ctrl Pts',(-0.0719464861410047,1.99467533572662,
5.32551929715076));
#11570=CARTESIAN_POINT('Ctrl Pts',(-0.14178224182859,1.99092899721851,5.32996410870872));
#11571=CARTESIAN_POINT('Ctrl Pts',(-0.211196141989236,1.98353819023201,
5.33440892026668));
#11572=CARTESIAN_POINT('Ctrl Pts',(-0.280681757242118,1.97613974742036,
5.33885832398947));
#11573=CARTESIAN_POINT('Ctrl Pts',(-0.349744160958529,1.96508937225319,
5.34330772771225));
#11574=CARTESIAN_POINT('Ctrl Pts',(-0.417977924856529,1.95046712785236,
5.34775713143504));
#11575=CARTESIAN_POINT('Ctrl Pts',(-0.486250650610277,1.93583653406928,
5.35220907579191));
#11576=CARTESIAN_POINT('Ctrl Pts',(-0.553693323397087,1.91763013788569,
5.35666102014877));
#11577=CARTESIAN_POINT('Ctrl Pts',(-0.619914716242915,1.89597819267139,
5.36111296450564));
#11578=CARTESIAN_POINT('Ctrl Pts',(-0.686249234273024,1.87428925970755,
5.36557251406385));
#11579=CARTESIAN_POINT('Ctrl Pts',(-0.751357852414863,1.84914320335359,
5.37003206362206));
#11580=CARTESIAN_POINT('Ctrl Pts',(-0.814869132399808,1.82071850091166,
5.37449161318027));
#11581=CARTESIAN_POINT('Ctrl Pts',(-0.847987482030452,1.80589626407684,
5.37681707287025));
#11582=CARTESIAN_POINT('Ctrl Pts',(-0.88067189007166,1.79018327490047,5.37914253256023));
#11583=CARTESIAN_POINT('Ctrl Pts',(-0.912872628507629,1.77360963197136,
5.38146799225021));
#11584=CARTESIAN_POINT('Ctrl Pts',(-0.974655985131309,1.74180988633263,
5.38592983729844));
#11585=CARTESIAN_POINT('Ctrl Pts',(-1.03489322914811,1.70671752778341,5.39039168234667));
#11586=CARTESIAN_POINT('Ctrl Pts',(-1.09321210451729,1.66850677464519,5.3948535273949));
#11587=CARTESIAN_POINT('Ctrl Pts',(-1.15144567010817,1.63035191680429,5.39930884558525));
#11588=CARTESIAN_POINT('Ctrl Pts',(-1.20776603278464,1.5890879845105,5.40376416377559));
#11589=CARTESIAN_POINT('Ctrl Pts',(-1.26182512641187,1.54493524552185,5.40821948196593));
#11590=CARTESIAN_POINT('Ctrl Pts',(-1.31582315400275,1.50083238218932,5.41266976735598));
#11591=CARTESIAN_POINT('Ctrl Pts',(-1.36756461026547,1.45384750082595,5.41712005274602));
#11592=CARTESIAN_POINT('Ctrl Pts',(-1.41673151392217,1.40424334784246,5.42157033813607));
#11593=CARTESIAN_POINT('Ctrl Pts',(-1.46586884463928,1.35466903079556,5.4260179467657));
#11594=CARTESIAN_POINT('Ctrl Pts',(-1.51243435264932,1.30247891342531,5.43046555539534));
#11595=CARTESIAN_POINT('Ctrl Pts',(-1.55614533347603,1.24797406367311,5.43491316402498));
#11596=CARTESIAN_POINT('Ctrl Pts',(-1.59984472482338,1.1934836652743,5.43935959342076));
#11597=CARTESIAN_POINT('Ctrl Pts',(-1.64069078681985,1.13668013322742,5.44380602281655));
#11598=CARTESIAN_POINT('Ctrl Pts',(-1.67844085819717,1.07789788386208,5.44825245221233));
#11599=CARTESIAN_POINT('Ctrl Pts',(-1.71619361699196,1.01911144980415,5.45269919814823));
#11600=CARTESIAN_POINT('Ctrl Pts',(-1.75084968610701,0.958346430253622,
5.45714594408413));
#11601=CARTESIAN_POINT('Ctrl Pts',(-1.78221049605736,0.895965016193699,
5.46159269002003));
#11602=CARTESIAN_POINT('Ctrl Pts',(-1.8136051237754,0.833516333457627,5.46604423108148));
#11603=CARTESIAN_POINT('Ctrl Pts',(-1.84169718062978,0.769448213746021,
5.47049577214293));
#11604=CARTESIAN_POINT('Ctrl Pts',(-1.86633515606672,0.704145331397873,
5.47494731320438));
#11605=CARTESIAN_POINT('Ctrl Pts',(-1.89098784905164,0.638803440231542,
5.47940151340352));
#11606=CARTESIAN_POINT('Ctrl Pts',(-1.91218220563635,0.572225782930733,
5.48385571360267));
#11607=CARTESIAN_POINT('Ctrl Pts',(-1.92981663893441,0.504812145844266,
5.48830991380181));
#11608=CARTESIAN_POINT('Ctrl Pts',(-1.94748182379731,0.437280950410659,
5.49277188139692));
#11609=CARTESIAN_POINT('Ctrl Pts',(-1.9615745946863,0.368911342533814,5.49723384899204));
#11610=CARTESIAN_POINT('Ctrl Pts',(-1.97204464136655,0.300112470513115,
5.50169581658715));
#11611=CARTESIAN_POINT('Ctrl Pts',(-1.97746364796756,0.264504077063874,
5.50400520761375));
#11612=CARTESIAN_POINT('Ctrl Pts',(-1.98191304825906,0.22878076537244,5.50631459864035));
#11613=CARTESIAN_POINT('Ctrl Pts',(-1.98539134842953,0.192999368084864,
5.50862398966694));
#11614=CARTESIAN_POINT('Ctrl Pts',(-1.9915820919786,0.12931496950562,5.5127342869097));
#11615=CARTESIAN_POINT('Ctrl Pts',(-1.99470965376256,0.0653246187217622,
5.51684458415246));
#11616=CARTESIAN_POINT('Ctrl Pts',(-1.99474961218935,0.00124385305840679,
5.52095488139522));
#11617=CARTESIAN_POINT('',(-1.99474967239247,0.00114323669999672,6.32095488134804));
#11618=CARTESIAN_POINT('Ctrl Pts',(-1.99474961218969,0.00124385252382661,
5.52095488142951));
#11619=CARTESIAN_POINT('Ctrl Pts',(-1.9947923012447,-0.067216012531803,
5.52534606483161));
#11620=CARTESIAN_POINT('Ctrl Pts',(-1.99130645198071,-0.135821349700975,
5.52973724823371));
#11621=CARTESIAN_POINT('Ctrl Pts',(-1.9842735171274,-0.204171917086737,
5.5341284316358));
#11622=CARTESIAN_POINT('Ctrl Pts',(-1.97725128635011,-0.272418455402859,
5.5385129316885));
#11623=CARTESIAN_POINT('Ctrl Pts',(-1.96669273659649,-0.340410496159951,
5.54289743174119));
#11624=CARTESIAN_POINT('Ctrl Pts',(-1.95263133344811,-0.40774800813326,
5.54728193179388));
#11625=CARTESIAN_POINT('Ctrl Pts',(-1.93858172148399,-0.475029054261563,
5.55166275522572));
#11626=CARTESIAN_POINT('Ctrl Pts',(-1.92103517909631,-0.541656167923529,
5.55604357865757));
#11627=CARTESIAN_POINT('Ctrl Pts',(-1.90007676440551,-0.607236240573879,
5.56042440208941));
#11628=CARTESIAN_POINT('Ctrl Pts',(-1.87912834776242,-0.672785028763785,
5.56480313568372));
#11629=CARTESIAN_POINT('Ctrl Pts',(-1.85477143901977,-0.737287286775999,
5.56918186927803));
#11630=CARTESIAN_POINT('Ctrl Pts',(-1.82714130271717,-0.800363806281255,
5.57356060287234));
#11631=CARTESIAN_POINT('Ctrl Pts',(-1.79951436007353,-0.863433035019276,
5.57793883034602));
#11632=CARTESIAN_POINT('Ctrl Pts',(-1.76861514440305,-0.925076391265085,
5.5823170578197));
#11633=CARTESIAN_POINT('Ctrl Pts',(-1.73462677544328,-0.984935283363958,
5.58669528529339));
#11634=CARTESIAN_POINT('Ctrl Pts',(-1.70060673917722,-1.04484994659657,
5.59107759200579));
#11635=CARTESIAN_POINT('Ctrl Pts',(-1.66349205160161,-1.10297638629838,
5.59545989871818));
#11636=CARTESIAN_POINT('Ctrl Pts',(-1.62351090162258,-1.15898227545232,
5.59984220543058));
#11637=CARTESIAN_POINT('Ctrl Pts',(-1.58351074586159,-1.21501478804552,
5.60422659535384));
#11638=CARTESIAN_POINT('Ctrl Pts',(-1.54064173061988,-1.26892434962013,
5.6086109852771));
#11639=CARTESIAN_POINT('Ctrl Pts',(-1.49517250870967,-1.32041157663012,
5.61299537520035));
#11640=CARTESIAN_POINT('Ctrl Pts',(-1.44962193118818,-1.37199092694133,
5.61738760987457));
#11641=CARTESIAN_POINT('Ctrl Pts',(-1.40146221209025,-1.42113892980289,
5.6217798445488));
#11642=CARTESIAN_POINT('Ctrl Pts',(-1.3509984143541,-1.46759355644289,5.62617207922302));
#11643=CARTESIAN_POINT('Ctrl Pts',(-1.31420229917125,-1.50146634979783,
5.62937471517657));
#11644=CARTESIAN_POINT('Ctrl Pts',(-1.27618192583642,-1.53390795235667,
5.63257735113012));
#11645=CARTESIAN_POINT('Ctrl Pts',(-1.23706539739349,-1.56483122574663,
5.63577998708368));
#11646=CARTESIAN_POINT('Ctrl Pts',(-1.18264856416134,-1.60785003845923,
5.64023532383071));
#11647=CARTESIAN_POINT('Ctrl Pts',(-1.1258777518735,-1.64811182099942,5.64469066057773));
#11648=CARTESIAN_POINT('Ctrl Pts',(-1.06706373825887,-1.6853493824703,5.64914599732476));
#11649=CARTESIAN_POINT('Ctrl Pts',(-1.00833802735375,-1.72253103587825,
5.65359464487847));
#11650=CARTESIAN_POINT('Ctrl Pts',(-0.947575613746329,-1.75669722063681,
5.65804329243219));
#11651=CARTESIAN_POINT('Ctrl Pts',(-0.885119358305062,-1.78762168370537,
5.6624919399859));
#11652=CARTESIAN_POINT('Ctrl Pts',(-0.822736679037341,-1.81850971641728,
5.66693534684015));
#11653=CARTESIAN_POINT('Ctrl Pts',(-0.75866455749729,-1.84616339634459,
5.6713787536944));
#11654=CARTESIAN_POINT('Ctrl Pts',(-0.693272231122471,-1.87040134090373,
5.67582216054865));
#11655=CARTESIAN_POINT('Ctrl Pts',(-0.627921132954196,-1.89462400405234,
5.68026276594735));
#11656=CARTESIAN_POINT('Ctrl Pts',(-0.56125193886616,-1.91543503440923,
5.68470337134605));
#11657=CARTESIAN_POINT('Ctrl Pts',(-0.493654338107925,-1.93270094866413,
5.68914397674475));
#11658=CARTESIAN_POINT('Ctrl Pts',(-0.426076423290402,-1.94996183469671,
5.69358328893935));
#11659=CARTESIAN_POINT('Ctrl Pts',(-0.357571112320087,-1.96367953317274,
5.69802260113395));
#11660=CARTESIAN_POINT('Ctrl Pts',(-0.288542033082598,-1.97377077130161,
5.70246191332854));
#11661=CARTESIAN_POINT('Ctrl Pts',(-0.219509639122772,-1.98386249400383,
5.70690143869544));
#11662=CARTESIAN_POINT('Ctrl Pts',(-0.149953911393263,-1.99032734221718,
5.71134096406233));
#11663=CARTESIAN_POINT('Ctrl Pts',(-0.0802856487958224,-1.9931336576099,
5.71578048942923));
#11664=CARTESIAN_POINT('Ctrl Pts',(-0.0105438244567896,-1.9959429361517,
5.7202247024287));
#11665=CARTESIAN_POINT('Ctrl Pts',(0.0593102821093654,-1.99508595175291,
5.72466891542818));
#11666=CARTESIAN_POINT('Ctrl Pts',(0.128864772078434,-1.99058318917275,
5.72911312842766));
#11667=CARTESIAN_POINT('Ctrl Pts',(0.198459756193018,-1.9860778051152,5.73355992881737));
#11668=CARTESIAN_POINT('Ctrl Pts',(0.267754290470471,-1.977922475244,5.73800672920708));
#11669=CARTESIAN_POINT('Ctrl Pts',(0.336343287961951,-1.96618939961107,
5.74245352959679));
#11670=CARTESIAN_POINT('Ctrl Pts',(0.405051579770993,-1.95443591707176,
5.74690806414266));
#11671=CARTESIAN_POINT('Ctrl Pts',(0.473051408038398,-1.93909237483016,
5.75136259868854));
#11672=CARTESIAN_POINT('Ctrl Pts',(0.539950309985821,-1.92028154843143,
5.75581713323441));
#11673=CARTESIAN_POINT('Ctrl Pts',(0.575587653455228,-1.91026093730329,
5.75819008365642));
#11674=CARTESIAN_POINT('Ctrl Pts',(0.610912875599195,-1.89925723901571,
5.76056303407842));
#11675=CARTESIAN_POINT('Ctrl Pts',(0.645869037961982,-1.88729455790612,
5.76293598450042));
#11676=CARTESIAN_POINT('Ctrl Pts',(0.711495626231272,-1.86483585836044,
5.76739095409096));
#11677=CARTESIAN_POINT('Ctrl Pts',(0.776078710937367,-1.83890579026429,
5.7718459236815));
#11678=CARTESIAN_POINT('Ctrl Pts',(0.839225447637288,-1.80962101295768,
5.77630089327204));
#11679=CARTESIAN_POINT('Ctrl Pts',(0.902277588112757,-1.78038010536647,
5.78074918914791));
#11680=CARTESIAN_POINT('Ctrl Pts',(0.963897210932753,-1.74779466727024,
5.78519748502378));
#11681=CARTESIAN_POINT('Ctrl Pts',(1.02370852762626,-1.71203049416921,5.78964578089965));
#11682=CARTESIAN_POINT('Ctrl Pts',(1.08344971310567,-1.6763082560233,5.79408886096674));
#11683=CARTESIAN_POINT('Ctrl Pts',(1.1413863857378,-1.63741493552949,5.79853194103383));
#11684=CARTESIAN_POINT('Ctrl Pts',(1.19716620747039,-1.59556279543958,5.80297502110093));
#11685=CARTESIAN_POINT('Ctrl Pts',(1.25291105510323,-1.5537368967552,5.80741531534475));
#11686=CARTESIAN_POINT('Ctrl Pts',(1.30650134413439,-1.50895615180086,5.81185560958857));
#11687=CARTESIAN_POINT('Ctrl Pts',(1.35761394400723,-1.46147594627388,5.81629590383239));
#11688=CARTESIAN_POINT('Ctrl Pts',(1.408711843642,-1.41400939629028,5.82073492102549));
#11689=CARTESIAN_POINT('Ctrl Pts',(1.45733311043558,-1.36384525986239,5.82517393821859));
#11690=CARTESIAN_POINT('Ctrl Pts',(1.50318929080677,-1.31127781896281,5.82961295541169));
#11691=CARTESIAN_POINT('Ctrl Pts',(1.54904784572592,-1.25870765598936,5.83405220246823));
#11692=CARTESIAN_POINT('Ctrl Pts',(1.59214071008936,-1.20373431177558,5.83849144952477));
#11693=CARTESIAN_POINT('Ctrl Pts',(1.63221895130854,-1.14668603265639,5.84293069658131));
#11694=CARTESIAN_POINT('Ctrl Pts',(1.67233976145668,-1.08957715995656,5.84737465876473));
#11695=CARTESIAN_POINT('Ctrl Pts',(1.70943927566257,-1.03038935471185,5.85181862094815));
#11696=CARTESIAN_POINT('Ctrl Pts',(1.74331181171396,-0.969480009922113,
5.85626258313157));
#11697=CARTESIAN_POINT('Ctrl Pts',(1.77720418540061,-0.908534993242815,
5.86070914794565));
#11698=CARTESIAN_POINT('Ctrl Pts',(1.80786560417123,-0.845866869904689,
5.86515571275973));
#11699=CARTESIAN_POINT('Ctrl Pts',(1.83513756064359,-0.781855290968285,
5.86960227757381));
#11700=CARTESIAN_POINT('Ctrl Pts',(1.86245711540089,-0.717731991357304,
5.8740566030654));
#11701=CARTESIAN_POINT('Ctrl Pts',(1.88637523117278,-0.652261015143535,
5.87851092855698));
#11702=CARTESIAN_POINT('Ctrl Pts',(1.90678276159614,-0.585838768416548,
5.88296525404856));
#11703=CARTESIAN_POINT('Ctrl Pts',(1.91766648320351,-0.550414529083512,
5.88534083000476));
#11704=CARTESIAN_POINT('Ctrl Pts',(1.92755255690717,-0.514719928244699,
5.88771640596095));
#11705=CARTESIAN_POINT('Ctrl Pts',(1.93643040487919,-0.478816091583604,
5.89009198191715));
#11706=CARTESIAN_POINT('Ctrl Pts',(1.95307244233698,-0.411512281417537,
5.89454513589899));
#11707=CARTESIAN_POINT('Ctrl Pts',(1.96623450191741,-0.343205993838856,
5.89899828988084));
#11708=CARTESIAN_POINT('Ctrl Pts',(1.97580171301588,-0.274290272054082,
5.90345144386268));
#11709=CARTESIAN_POINT('Ctrl Pts',(1.98535451082555,-0.205478373859169,
5.90789788903527));
#11710=CARTESIAN_POINT('Ctrl Pts',(1.99132314210793,-0.136059344847672,
5.91234433420785));
#11711=CARTESIAN_POINT('Ctrl Pts',(1.9936432686362,-0.0664385424402738,
5.91679077938043));
#11712=CARTESIAN_POINT('Ctrl Pts',(1.99596065109929,0.00309991789794359,
5.92123196564356));
#11713=CARTESIAN_POINT('Ctrl Pts',(1.99463808295563,0.0728391905275966,
5.92567315190669));
#11714=CARTESIAN_POINT('Ctrl Pts',(1.98966298447894,0.142368432927878,5.93011433816982));
#11715=CARTESIAN_POINT('Ctrl Pts',(1.98469103545918,0.211853660248919,5.93455271296602));
#11716=CARTESIAN_POINT('Ctrl Pts',(1.97607117780648,0.281128633700857,5.93899108776222));
#11717=CARTESIAN_POINT('Ctrl Pts',(1.9638429012161,0.349783678640308,5.94342946255843));
#11718=CARTESIAN_POINT('Ctrl Pts',(1.95161820583892,0.418418617037978,5.94786653751762));
#11719=CARTESIAN_POINT('Ctrl Pts',(1.93578727518894,0.486433505382848,5.95230361247682));
#11720=CARTESIAN_POINT('Ctrl Pts',(1.91644108088272,0.55342673047576,5.95674068743601));
#11721=CARTESIAN_POINT('Ctrl Pts',(1.89709397134644,0.62042312488517,5.96117797230441));
#11722=CARTESIAN_POINT('Ctrl Pts',(1.87423140617596,0.686397290190647,5.96561525717282));
#11723=CARTESIAN_POINT('Ctrl Pts',(1.84799431799466,0.750962424598896,5.97005254204122));
#11724=CARTESIAN_POINT('Ctrl Pts',(1.82172945025819,0.815595919897694,5.97449452506054));
#11725=CARTESIAN_POINT('Ctrl Pts',(1.79208311290496,0.87881695194219,5.97893650807985));
#11726=CARTESIAN_POINT('Ctrl Pts',(1.75924416903776,0.940259281372236,5.98337849109917));
#11727=CARTESIAN_POINT('Ctrl Pts',(1.72638607747854,1.00173743652206,5.98782306414462));
#11728=CARTESIAN_POINT('Ctrl Pts',(1.69033192755659,1.0614344054251,5.99226763719007));
#11729=CARTESIAN_POINT('Ctrl Pts',(1.65131484610172,1.11901154665359,5.99671221023552));
#11730=CARTESIAN_POINT('Ctrl Pts',(1.61222962352486,1.17668924309682,6.00116454547596));
#11731=CARTESIAN_POINT('Ctrl Pts',(1.57017143564818,1.23223933126419,6.0056168807164));
#11732=CARTESIAN_POINT('Ctrl Pts',(1.52541422963819,1.28535558913373,6.01006921595683));
#11733=CARTESIAN_POINT('Ctrl Pts',(1.50135933304927,1.31390308358541,6.01246213708252));
#11734=CARTESIAN_POINT('Ctrl Pts',(1.47652545867745,1.34174817175601,6.01485505820821));
#11735=CARTESIAN_POINT('Ctrl Pts',(1.4509593153368,1.3688479198718,6.01724797933389));
#11736=CARTESIAN_POINT('Ctrl Pts',(1.40336940591118,1.41929254662303,6.02170226475804));
#11737=CARTESIAN_POINT('Ctrl Pts',(1.35305152644983,1.46735223801887,6.0261565501822));
#11738=CARTESIAN_POINT('Ctrl Pts',(1.30027421093083,1.51271760050851,6.03061083560635));
#11739=CARTESIAN_POINT('Ctrl Pts',(1.24757620065672,1.55801479524185,6.03505842784815));
#11740=CARTESIAN_POINT('Ctrl Pts',(1.1924264574792,1.6006253800914,6.03950602008996));
#11741=CARTESIAN_POINT('Ctrl Pts',(1.13513120857,1.64027580053795,6.04395361233177));
#11742=CARTESIAN_POINT('Ctrl Pts',(1.07790348008118,1.67987949436915,6.04839596324373));
#11743=CARTESIAN_POINT('Ctrl Pts',(1.0185356681765,1.71652967510947,6.0528383141557));
#11744=CARTESIAN_POINT('Ctrl Pts',(0.957366616645845,1.74999334965367,6.05728066506767));
#11745=CARTESIAN_POINT('Ctrl Pts',(0.896236136705961,1.7834359228872,6.0617202147503));
#11746=CARTESIAN_POINT('Ctrl Pts',(0.833307098785434,1.81369574159731,6.06615976443293));
#11747=CARTESIAN_POINT('Ctrl Pts',(0.768945538335652,1.84058423376212,6.07059931411557));
#11748=CARTESIAN_POINT('Ctrl Pts',(0.704602699117713,1.86746490471047,6.07503757243984));
#11749=CARTESIAN_POINT('Ctrl Pts',(0.638828615998939,1.89097600724552,6.07947583076412));
#11750=CARTESIAN_POINT('Ctrl Pts',(0.572010404389035,1.91097662460081,6.0839140890884));
#11751=CARTESIAN_POINT('Ctrl Pts',(0.505188931272009,1.93097821821921,6.08835256405138));
#11752=CARTESIAN_POINT('Ctrl Pts',(0.437323698104091,1.94746884838247,6.09279103901437));
#11753=CARTESIAN_POINT('Ctrl Pts',(0.368816404675191,1.96035762608318,6.09722951397736));
#11754=CARTESIAN_POINT('Ctrl Pts',(0.300236563836182,1.97326005265826,6.10167268916783));
#11755=CARTESIAN_POINT('Ctrl Pts',(0.231013787655493,1.98255292298725,6.10611586435829));
#11756=CARTESIAN_POINT('Ctrl Pts',(0.161558428550818,1.98819678016644,6.11055903954876));
#11757=CARTESIAN_POINT('Ctrl Pts',(0.0920625359450201,1.99384393104815,
6.11500480773492));
#11758=CARTESIAN_POINT('Ctrl Pts',(0.0223342797007121,1.99583781617353,
6.11945057592108));
#11759=CARTESIAN_POINT('Ctrl Pts',(-0.0472152311563271,1.99419113538468,
6.12389634410723));
#11760=CARTESIAN_POINT('Ctrl Pts',(-0.116886046268897,1.99254158254994,
6.12834986634649));
#11761=CARTESIAN_POINT('Ctrl Pts',(-0.186377005639694,1.9872388259532,6.13280338858574));
#11762=CARTESIAN_POINT('Ctrl Pts',(-0.255282160080176,1.97834743693943,
6.137256910825));
#11763=CARTESIAN_POINT('Ctrl Pts',(-0.292142099617515,1.9735911010149,6.13963926613354));
#11764=CARTESIAN_POINT('Ctrl Pts',(-0.32883457540803,1.96780872561293,6.14202162144208));
#11765=CARTESIAN_POINT('Ctrl Pts',(-0.365299029972776,1.96101610936804,
6.14440397675062));
#11766=CARTESIAN_POINT('Ctrl Pts',(-0.433474361558249,1.94831637560385,
6.14885811887486));
#11767=CARTESIAN_POINT('Ctrl Pts',(-0.50112157463356,1.93203206395733,6.15331226099909));
#11768=CARTESIAN_POINT('Ctrl Pts',(-0.567835177170299,1.91222142391198,
6.15776640312333));
#11769=CARTESIAN_POINT('Ctrl Pts',(-0.634448541320298,1.89244054970933,
6.16221385281898));
#11770=CARTESIAN_POINT('Ctrl Pts',(-0.700130613620823,1.86914400129941,
6.16666130251463));
#11771=CARTESIAN_POINT('Ctrl Pts',(-0.764485625150959,1.84244112292294,
6.17110875221028));
#11772=CARTESIAN_POINT('Ctrl Pts',(-0.828764820816398,1.81576970288617,
6.17555096241896));
#11773=CARTESIAN_POINT('Ctrl Pts',(-0.891719610835551,1.78570010983387,
6.17999317262764));
#11774=CARTESIAN_POINT('Ctrl Pts',(-0.952970668561464,1.75239107146821,
6.18443538283632));
#11775=CARTESIAN_POINT('Ctrl Pts',(-1.01418311864234,1.71910302838946,6.18887479303988));
#11776=CARTESIAN_POINT('Ctrl Pts',(-1.07369353773084,1.68257982395457,6.19331420324345));
#11777=CARTESIAN_POINT('Ctrl Pts',(-1.13114522433883,1.64302709775446,6.19775361344701));
#11778=CARTESIAN_POINT('Ctrl Pts',(-1.18858021774735,1.60348586402023,6.20219173373266));
#11779=CARTESIAN_POINT('Ctrl Pts',(-1.24395726316132,1.560917133434,6.2066298540183));
#11780=CARTESIAN_POINT('Ctrl Pts',(-1.29694831277892,1.51557006980209,6.21106797430394));
#11781=CARTESIAN_POINT('Ctrl Pts',(-1.3499419688548,1.47022077569484,6.21550631288637));
#11782=CARTESIAN_POINT('Ctrl Pts',(-1.40054902575009,1.42209319732952,6.21994465146879));
#11783=CARTESIAN_POINT('Ctrl Pts',(-1.44847560118041,1.3714758456805,6.22438299005121));
#11784=CARTESIAN_POINT('Ctrl Pts',(-1.49645296876867,1.32080485021286,6.22882603234534));
#11785=CARTESIAN_POINT('Ctrl Pts',(-1.54174384764662,1.26763917104718,6.23326907463948));
#11786=CARTESIAN_POINT('Ctrl Pts',(-1.58409291328415,1.2123024394032,6.23771211693362));
#11787=CARTESIAN_POINT('Ctrl Pts',(-1.6264667111397,1.15693339063269,6.24215775400261));
#11788=CARTESIAN_POINT('Ctrl Pts',(-1.66589499939298,1.09939116969751,6.2466033910716));
#11789=CARTESIAN_POINT('Ctrl Pts',(-1.70216589599974,1.04002828086327,6.2510490281406));
#11790=CARTESIAN_POINT('Ctrl Pts',(-1.73850009042253,0.980561795438689,
6.25550242347155));
#11791=CARTESIAN_POINT('Ctrl Pts',(-1.77166566112311,0.9192687301121,6.2599558188025));
#11792=CARTESIAN_POINT('Ctrl Pts',(-1.80149713174049,0.856525333443663,
6.26440921413346));
#11793=CARTESIAN_POINT('Ctrl Pts',(-1.81746380226121,0.822943243079948,
6.26679280081142));
#11794=CARTESIAN_POINT('Ctrl Pts',(-1.83247618130686,0.788946008594228,
6.26917638748939));
#11795=CARTESIAN_POINT('Ctrl Pts',(-1.84651473762329,0.75459319254815,6.27155997416736));
#11796=CARTESIAN_POINT('Ctrl Pts',(-1.87590422211887,0.682676142688478,
6.276549973291));
#11797=CARTESIAN_POINT('Ctrl Pts',(-1.90112125185148,0.608959762926832,
6.28153997241463));
#11798=CARTESIAN_POINT('Ctrl Pts',(-1.92196856688165,0.533914216348369,
6.28652997153827));
#11799=CARTESIAN_POINT('Ctrl Pts',(-1.94274065878641,0.459139455746603,
6.29150196530585));
#11800=CARTESIAN_POINT('Ctrl Pts',(-1.95917436280922,0.383045343934298,
6.29647395907343));
#11801=CARTESIAN_POINT('Ctrl Pts',(-1.97112115201587,0.306119203212767,
6.30144595284101));
#11802=CARTESIAN_POINT('Ctrl Pts',(-1.98299656103722,0.229652684075272,
6.30638823972833));
#11803=CARTESIAN_POINT('Ctrl Pts',(-1.99043838878741,0.152364307798669,
6.31133052661565));
#11804=CARTESIAN_POINT('Ctrl Pts',(-1.99334890400618,0.0747509825847146,
6.31627281350298));
#11805=CARTESIAN_POINT('Ctrl Pts',(-1.9942679947044,0.0502420280178952,
6.31783350278466));
#11806=CARTESIAN_POINT('Ctrl Pts',(-1.99473559789568,0.0257007914548224,
6.31939419206635));
#11807=CARTESIAN_POINT('Ctrl Pts',(-1.99474967239247,0.00114323669999672,
6.32095488134804));
#11808=CARTESIAN_POINT('',(-1.99475051923913,-0.000231578174347214,7.92279770353672));
#11809=CARTESIAN_POINT('Ctrl Pts',(-1.99474972256478,0.00105205880370748,
6.31944091739086));
#11810=CARTESIAN_POINT('Ctrl Pts',(-1.99477744461827,-0.0515101728021833,
6.32260645846605));
#11811=CARTESIAN_POINT('Ctrl Pts',(-1.99272763490246,-0.104049755308175,
6.32582344761956));
#11812=CARTESIAN_POINT('Ctrl Pts',(-1.98792329969081,-0.165118817176486,
6.32964937505444));
#11813=CARTESIAN_POINT('Ctrl Pts',(-1.98718416083469,-0.173788309031887,
6.33019453377832));
#11814=CARTESIAN_POINT('Ctrl Pts',(-1.98586247174082,-0.188177734492508,
6.33110285450026));
#11815=CARTESIAN_POINT('Ctrl Pts',(-1.98531186365345,-0.193900539832301,
6.33146501686582));
#11816=CARTESIAN_POINT('Ctrl Pts',(-1.98427511807121,-0.204208415796533,
6.3321190244032));
#11817=CARTESIAN_POINT('Ctrl Pts',(-1.98379780732684,-0.208794349402572,
6.33241059083647));
#11818=CARTESIAN_POINT('Ctrl Pts',(-1.982790989217,-0.218152492191368,6.33300681262577));
#11819=CARTESIAN_POINT('Ctrl Pts',(-1.98226014254585,-0.222924523958921,
6.33331150826404));
#11820=CARTESIAN_POINT('Ctrl Pts',(-1.9810783692691,-0.233209944863012,
6.33396968410619));
#11821=CARTESIAN_POINT('Ctrl Pts',(-1.98042164592977,-0.238722614918188,
6.33432334478309));
#11822=CARTESIAN_POINT('Ctrl Pts',(-1.97858702868945,-0.253593976284769,
6.33527986739594));
#11823=CARTESIAN_POINT('Ctrl Pts',(-1.97736576347493,-0.262947080739622,
6.3358840932835));
#11824=CARTESIAN_POINT('Ctrl Pts',(-1.97128705934792,-0.307061623973,6.33874669531897));
#11825=CARTESIAN_POINT('Ctrl Pts',(-1.96557928455428,-0.341697712851584,
6.34103177104202));
#11826=CARTESIAN_POINT('Ctrl Pts',(-1.95340752322231,-0.405085067763132,
6.3452860522495));
#11827=CARTESIAN_POINT('Ctrl Pts',(-1.94721438490059,-0.433878851796861,
6.34724637621284));
#11828=CARTESIAN_POINT('Ctrl Pts',(-1.89984439107361,-0.632606107181402,
6.36096895098833));
#11829=CARTESIAN_POINT('Ctrl Pts',(-1.8371160572075,-0.796610341711909,
6.37337363602623));
#11830=CARTESIAN_POINT('Ctrl Pts',(-1.72340193659099,-1.00647675563919,
6.38978603019156));
#11831=CARTESIAN_POINT('Ctrl Pts',(-1.69027884995545,-1.06116397510046,
6.39410779554719));
#11832=CARTESIAN_POINT('Ctrl Pts',(-1.65071104264968,-1.1199235205728,6.3987274612763));
#11833=CARTESIAN_POINT('Ctrl Pts',(-1.64680819589923,-1.12565465735264,
6.39917776919579));
#11834=CARTESIAN_POINT('Ctrl Pts',(-1.64093774469943,-1.13417924194797,
6.39984701510508));
#11835=CARTESIAN_POINT('Ctrl Pts',(-1.63899277010808,-1.1369880979177,6.40006744238022));
#11836=CARTESIAN_POINT('Ctrl Pts',(-1.63564679302806,-1.141793799642,6.40044440039165));
#11837=CARTESIAN_POINT('Ctrl Pts',(-1.63424933839479,-1.14379308122026,
6.40060117123368));
#11838=CARTESIAN_POINT('Ctrl Pts',(-1.63133409071118,-1.14794755773208,
6.40092682568418));
#11839=CARTESIAN_POINT('Ctrl Pts',(-1.62981569806856,-1.15010230038321,
6.40109566637637));
#11840=CARTESIAN_POINT('Ctrl Pts',(-1.62560067317879,-1.15605870876959,
6.40156224462036));
#11841=CARTESIAN_POINT('Ctrl Pts',(-1.62289495892478,-1.15985397361839,
6.4018593636531));
#11842=CARTESIAN_POINT('Ctrl Pts',(-1.61217612655929,-1.17477817502841,
6.403027201273));
#11843=CARTESIAN_POINT('Ctrl Pts',(-1.60406140500754,-1.18583416101091,
6.40389117972435));
#11844=CARTESIAN_POINT('Ctrl Pts',(-1.5938215077739,-1.19948814263535,6.40495792865003));
#11845=CARTESIAN_POINT('Ctrl Pts',(-1.59180319962261,-1.20216528687708,
6.4051670745444));
#11846=CARTESIAN_POINT('Ctrl Pts',(-1.47625948307019,-1.35462476567131,
6.4170777417854));
#11847=CARTESIAN_POINT('Ctrl Pts',(-1.34212455588771,-1.48764105505261,
6.42754694131136));
#11848=CARTESIAN_POINT('Ctrl Pts',(-1.1382817295954,-1.63942572172107,6.4424914233546));
#11849=CARTESIAN_POINT('Ctrl Pts',(-1.08330577784576,-1.67626055422912,
6.44643440691091));
#11850=CARTESIAN_POINT('Ctrl Pts',(-1.00592310602849,-1.72270953433397,
6.45194659419272));
#11851=CARTESIAN_POINT('Ctrl Pts',(-0.985018140549544,-1.73474742327056,
6.4534319114796));
#11852=CARTESIAN_POINT('Ctrl Pts',(-0.953627321074768,-1.75207311154907,
6.45565957665956));
#11853=CARTESIAN_POINT('Ctrl Pts',(-0.943304310780017,-1.75765247525431,
6.45639172496357));
#11854=CARTESIAN_POINT('Ctrl Pts',(-0.926732750150575,-1.76642100763935,
6.45756666211685));
#11855=CARTESIAN_POINT('Ctrl Pts',(-0.920515458518767,-1.76966891113723,
6.4580073874649));
#11856=CARTESIAN_POINT('Ctrl Pts',(-0.90865641228606,-1.77578465465829,
6.45884794560778));
#11857=CARTESIAN_POINT('Ctrl Pts',(-0.903017876892885,-1.77865857539385,
6.45924755939515));
#11858=CARTESIAN_POINT('Ctrl Pts',(-0.893087651142748,-1.78366054965695,
6.45995130503853));
#11859=CARTESIAN_POINT('Ctrl Pts',(-0.888801771785937,-1.78580007807172,
6.46025503192961));
#11860=CARTESIAN_POINT('Ctrl Pts',(-0.880410575884844,-1.78995130682423,
6.46084969044561));
#11861=CARTESIAN_POINT('Ctrl Pts',(-0.87630596547766,-1.79196437387208,
6.46114057199418));
#11862=CARTESIAN_POINT('Ctrl Pts',(-0.865417544050263,-1.79725813951197,
6.46191222343387));
#11863=CARTESIAN_POINT('Ctrl Pts',(-0.858622051765832,-1.80051451402988,
6.46239383521247));
#11864=CARTESIAN_POINT('Ctrl Pts',(-0.834466616022044,-1.81192186209441,
6.46410597416705));
#11865=CARTESIAN_POINT('Ctrl Pts',(-0.817008205454793,-1.81986068617312,
6.46534378488314));
#11866=CARTESIAN_POINT('Ctrl Pts',(-0.629741323994729,-1.90177836965273,
6.47862903756359));
#11867=CARTESIAN_POINT('Ctrl Pts',(-0.450563654349494,-1.95199815661323,
6.49153662801257));
#11868=CARTESIAN_POINT('Ctrl Pts',(-0.168979054343724,-1.99004403633932,
6.51132612211482));
#11869=CARTESIAN_POINT('Ctrl Pts',(-0.070003666522376,-1.99597935232476,
6.51816336057112));
#11870=CARTESIAN_POINT('Ctrl Pts',(0.0386265208164566,-1.99439915239692,
6.52528083487543));
#11871=CARTESIAN_POINT('Ctrl Pts',(0.0482383789861798,-1.99418982420783,
6.52590722540753));
#11872=CARTESIAN_POINT('Ctrl Pts',(0.0617504707858433,-1.99379780304654,
6.52678268373903));
#11873=CARTESIAN_POINT('Ctrl Pts',(0.065652062648478,-1.99367314456987,
6.52703487209125));
#11874=CARTESIAN_POINT('Ctrl Pts',(0.07231851905358,-1.99344055592961,6.52746472190555));
#11875=CARTESIAN_POINT('Ctrl Pts',(0.0750835592791098,-1.99333832494506,
6.52764270090586));
#11876=CARTESIAN_POINT('Ctrl Pts',(0.0803838822548329,-1.99313131338395,
6.52798326590869));
#11877=CARTESIAN_POINT('Ctrl Pts',(0.0829191791686259,-1.99302744858703,
6.52814590389593));
#11878=CARTESIAN_POINT('Ctrl Pts',(0.0889351559742316,-1.99276948974236,
6.52853121365268));
#11879=CARTESIAN_POINT('Ctrl Pts',(0.0924156585639026,-1.99261111301622,
6.52875364571643));
#11880=CARTESIAN_POINT('Ctrl Pts',(0.102843906927676,-1.99210920430587,
6.52941868495274));
#11881=CARTESIAN_POINT('Ctrl Pts',(0.109790378816801,-1.9917384434692,6.52985980603651));
#11882=CARTESIAN_POINT('Ctrl Pts',(0.230485184815082,-1.98466312924971,
6.53749388010856));
#11883=CARTESIAN_POINT('Ctrl Pts',(0.343474201183392,-1.96825935870635,
6.54417709211632));
#11884=CARTESIAN_POINT('Ctrl Pts',(0.554848976247106,-1.91880175393996,
6.55679790705072));
#11885=CARTESIAN_POINT('Ctrl Pts',(0.653263445867949,-1.8875655122907,6.56272897672596));
#11886=CARTESIAN_POINT('Ctrl Pts',(0.799135076962752,-1.82848501768097,
6.57205969138134));
#11887=CARTESIAN_POINT('Ctrl Pts',(0.848592900520164,-1.80606304426536,
6.57532230788499));
#11888=CARTESIAN_POINT('Ctrl Pts',(0.915859545877599,-1.7721939235694,6.57993984516027));
#11889=CARTESIAN_POINT('Ctrl Pts',(0.934495546409145,-1.76243809354769,
6.58123889245969));
#11890=CARTESIAN_POINT('Ctrl Pts',(0.962306301824172,-1.74731422744665,
6.58320935682907));
#11891=CARTESIAN_POINT('Ctrl Pts',(0.971598492456417,-1.74216439825661,
6.58387317856972));
#11892=CARTESIAN_POINT('Ctrl Pts',(0.98857238525353,-1.73257925497255,6.58509605647586));
#11893=CARTESIAN_POINT('Ctrl Pts',(0.9962665290319,-1.72816643720659,6.58565430312171));
#11894=CARTESIAN_POINT('Ctrl Pts',(1.00853840649026,-1.72101896438434,6.58655110633162));
#11895=CARTESIAN_POINT('Ctrl Pts',(1.01313511018971,-1.71831697912146,6.5868884784308));
#11896=CARTESIAN_POINT('Ctrl Pts',(1.01772689524567,-1.71559305467304,6.58722696322272));
#11897=CARTESIAN_POINT('Ctrl Pts',(1.01773290126574,-1.71558949175785,6.5872274059608));
#11898=CARTESIAN_POINT('Ctrl Pts',(1.01774493154419,-1.71558235502268,6.58722829278647));
#11899=CARTESIAN_POINT('Ctrl Pts',(1.0177509557751,-1.71557878121873,6.58722873687205));
#11900=CARTESIAN_POINT('Ctrl Pts',(1.01776302226643,-1.71557162282909,6.58722962637739));
#11901=CARTESIAN_POINT('Ctrl Pts',(1.0177690646568,-1.71556803816607,6.58723007180674));
#11902=CARTESIAN_POINT('Ctrl Pts',(1.01778116774478,-1.71556085789276,6.58723096402014));
#11903=CARTESIAN_POINT('Ctrl Pts',(1.0177872283856,-1.71555726231589,6.58723141080001));
#11904=CARTESIAN_POINT('Ctrl Pts',(1.01779936826458,-1.71555006004202,6.58723230573588));
#11905=CARTESIAN_POINT('Ctrl Pts',(1.01780544734149,-1.7155464534404,6.58723275388001));
#11906=CARTESIAN_POINT('Ctrl Pts',(1.01781762374053,-1.71553922932512,6.58723365151848));
#11907=CARTESIAN_POINT('Ctrl Pts',(1.01782372116222,-1.71553561175213,6.58723410102017));
#11908=CARTESIAN_POINT('Ctrl Pts',(1.01783593461551,-1.71552836547692,6.58723500140071));
#11909=CARTESIAN_POINT('Ctrl Pts',(1.01784205054153,-1.71552473683709,6.58723545227179));
#11910=CARTESIAN_POINT('Ctrl Pts',(1.01785430099153,-1.7155174684345,6.58723635539026));
#11911=CARTESIAN_POINT('Ctrl Pts',(1.01786043549049,-1.71551382868632,6.58723680763582));
#11912=CARTESIAN_POINT('Ctrl Pts',(1.01787272299974,-1.71550653811761,6.58723771349691));
#11913=CARTESIAN_POINT('Ctrl Pts',(1.01787887607784,-1.71550288725659,6.58723816711746));
#11914=CARTESIAN_POINT('Ctrl Pts',(1.01789120095963,-1.71549557433426,6.58723907574439));
#11915=CARTESIAN_POINT('Ctrl Pts',(1.01789737274825,-1.71549191228163,6.58723953074967));
#11916=CARTESIAN_POINT('Ctrl Pts',(1.01790973488439,-1.71548457707418,6.5872404421338));
#11917=CARTESIAN_POINT('Ctrl Pts',(1.01791592533307,-1.71548090385907,6.58724089852013));
#11918=CARTESIAN_POINT('Ctrl Pts',(1.01792832521644,-1.71547354607239,6.5872418126979));
#11919=CARTESIAN_POINT('Ctrl Pts',(1.0179345345215,-1.71546986157747,6.58724227047981));
#11920=CARTESIAN_POINT('Ctrl Pts',(1.01794697194665,-1.71546248133181,6.58724318743618));
#11921=CARTESIAN_POINT('Ctrl Pts',(1.01795320009879,-1.71545878556177,6.58724364661302));
#11922=CARTESIAN_POINT('Ctrl Pts',(1.01796567538871,-1.71545138266381,6.5872445663719));
#11923=CARTESIAN_POINT('Ctrl Pts',(1.01797192249516,-1.71544767555419,6.58724502695164));
#11924=CARTESIAN_POINT('Ctrl Pts',(1.01798443565261,-1.7154402500006,6.58724594951333));
#11925=CARTESIAN_POINT('Ctrl Pts',(1.0179907017328,-1.71543653153903,6.58724641149744));
#11926=CARTESIAN_POINT('Ctrl Pts',(1.0180032530666,-1.71542908314486,6.58724733688481));
#11927=CARTESIAN_POINT('Ctrl Pts',(1.01800953826952,-1.71542535324207,6.58724780028434));
#11928=CARTESIAN_POINT('Ctrl Pts',(1.01802212759982,-1.71541788211236,6.58724872848423));
#11929=CARTESIAN_POINT('Ctrl Pts',(1.0180284318443,-1.71541414081568,6.58724919329324));
#11930=CARTESIAN_POINT('Ctrl Pts',(1.01804105978887,-1.71540664658209,6.5872501243513));
#11931=CARTESIAN_POINT('Ctrl Pts',(1.01804738333042,-1.71540289373901,6.58725059058867));
#11932=CARTESIAN_POINT('Ctrl Pts',(1.01806004947274,-1.71539537664701,6.58725152447429));
#11933=CARTESIAN_POINT('Ctrl Pts',(1.01806639220496,-1.71539161231981,6.58725199213225));
#11934=CARTESIAN_POINT('Ctrl Pts',(1.01807909713451,-1.71538407201784,6.58725292888899));
#11935=CARTESIAN_POINT('Ctrl Pts',(1.01808545923271,-1.71538029610161,6.5872533979805));
#11936=CARTESIAN_POINT('Ctrl Pts',(1.01809820282943,-1.71537273265916,6.58725433759963));
#11937=CARTESIAN_POINT('Ctrl Pts',(1.0181045843219,-1.71536894513624,6.58725480812682));
#11938=CARTESIAN_POINT('Ctrl Pts',(1.01811736682391,-1.71536135841022,6.58725575062599));
#11939=CARTESIAN_POINT('Ctrl Pts',(1.01812376780242,-1.71535755922525,6.5872562225957));
#11940=CARTESIAN_POINT('Ctrl Pts',(1.01813658926401,-1.71534994918168,6.58725716797902));
#11941=CARTESIAN_POINT('Ctrl Pts',(1.01814300976267,-1.71534613831354,6.5872576413938));
#11942=CARTESIAN_POINT('Ctrl Pts',(1.01815587046537,-1.71533850478353,6.58725858968213));
#11943=CARTESIAN_POINT('Ctrl Pts',(1.01816231062961,-1.71533468214499,6.58725906455277));
#11944=CARTESIAN_POINT('Ctrl Pts',(1.01817521039148,-1.71532702523475,6.58726001573281));
#11945=CARTESIAN_POINT('Ctrl Pts',(1.01818167012497,-1.7153231908821,6.58726049205225));
#11946=CARTESIAN_POINT('Ctrl Pts',(1.01819460961073,-1.71531551019526,6.58726144617312));
#11947=CARTESIAN_POINT('Ctrl Pts',(1.01820108917981,-1.7153116639695,6.58726192396105));
#11948=CARTESIAN_POINT('Ctrl Pts',(1.01821406800295,-1.71530395973367,6.58726288099435));
#11949=CARTESIAN_POINT('Ctrl Pts',(1.01822056734699,-1.71530010166988,6.58726336024637));
#11950=CARTESIAN_POINT('Ctrl Pts',(1.01823358593542,-1.71529237362922,6.58726432022377));
#11951=CARTESIAN_POINT('Ctrl Pts',(1.01824010515381,-1.71528850366748,6.58726480094725));
#11952=CARTESIAN_POINT('Ctrl Pts',(1.01825316354293,-1.71528075179914,6.58726576387146));
#11953=CARTESIAN_POINT('Ctrl Pts',(1.01825970266175,-1.71527686992306,6.58726624606838));
#11954=CARTESIAN_POINT('Ctrl Pts',(1.02242340091638,-1.71280510396838,6.58757328055461));
#11955=CARTESIAN_POINT('Ctrl Pts',(1.0265715439348,-1.71032213323363,6.58788038147212));
#11956=CARTESIAN_POINT('Ctrl Pts',(1.03598579856819,-1.70464041706431,6.58858013785632));
#11957=CARTESIAN_POINT('Ctrl Pts',(1.04124617837504,-1.70143231453255,6.58897313421463));
#11958=CARTESIAN_POINT('Ctrl Pts',(1.05720190257521,-1.69159982630021,6.59017130689509));
#11959=CARTESIAN_POINT('Ctrl Pts',(1.06784935454139,-1.68489868511379,6.59097930486818));
#11960=CARTESIAN_POINT('Ctrl Pts',(1.20950777495385,-1.59386163002618,6.60184464060991));
#11961=CARTESIAN_POINT('Ctrl Pts',(1.33023408679994,-1.49457731321874,6.61249972469336));
#11962=CARTESIAN_POINT('Ctrl Pts',(1.50166672770224,-1.31621559577668,6.62974270148864));
#11963=CARTESIAN_POINT('Ctrl Pts',(1.56054694475119,-1.24584145932417,6.63616419091552));
#11964=CARTESIAN_POINT('Ctrl Pts',(1.63469017815413,-1.14368311722831,6.64477894588772));
#11965=CARTESIAN_POINT('Ctrl Pts',(1.65426947702844,-1.11517525407169,6.64711285809053));
#11966=CARTESIAN_POINT('Ctrl Pts',(1.68359869975836,-1.06999757466042,6.65068759613698));
#11967=CARTESIAN_POINT('Ctrl Pts',(1.69386392789966,-1.05367189086545,6.65195505129884));
#11968=CARTESIAN_POINT('Ctrl Pts',(1.70652987241577,-1.03286451614205,6.65353747910869));
#11969=CARTESIAN_POINT('Ctrl Pts',(1.70915197346041,-1.02851973590306,6.65386611384148));
#11970=CARTESIAN_POINT('Ctrl Pts',(1.71330806898991,-1.02157336679463,6.65438862007934));
#11971=CARTESIAN_POINT('Ctrl Pts',(1.71485276292102,-1.0189782553177,6.65458317988249));
#11972=CARTESIAN_POINT('Ctrl Pts',(1.71777250611696,-1.01404759507408,6.65495160330142));
#11973=CARTESIAN_POINT('Ctrl Pts',(1.7191486720879,-1.01171278097614,6.65512553678619));
#11974=CARTESIAN_POINT('Ctrl Pts',(1.72229150130787,-1.00635570342453,6.65552342332095));
#11975=CARTESIAN_POINT('Ctrl Pts',(1.72405496824476,-1.00333159235627,6.65574716747327));
#11976=CARTESIAN_POINT('Ctrl Pts',(1.72959916945345,-0.993766248438064,
6.65645219698094));
#11977=CARTESIAN_POINT('Ctrl Pts',(1.73335076322023,-0.987208073068833,
6.65693163291302));
#11978=CARTESIAN_POINT('Ctrl Pts',(1.7975572137286,-0.873474105764137,6.66518099619098));
#11979=CARTESIAN_POINT('Ctrl Pts',(1.84801506115116,-0.760933180365182,
6.67235561461449));
#11980=CARTESIAN_POINT('Ctrl Pts',(1.92011243192427,-0.549736608298843,
6.68531074385638));
#11981=CARTESIAN_POINT('Ctrl Pts',(1.94526936378461,-0.452733932616914,
6.69108317192942));
#11982=CARTESIAN_POINT('Ctrl Pts',(1.97199907273376,-0.304617246401701,
6.70003379705962));
#11983=CARTESIAN_POINT('Ctrl Pts',(1.97907069257955,-0.254657856555056,
6.70307389550469));
#11984=CARTESIAN_POINT('Ctrl Pts',(1.98734264182223,-0.174390859627053,
6.70802810825));
#11985=CARTESIAN_POINT('Ctrl Pts',(1.98975893393945,-0.144229604993428,
6.70990520348969));
#11986=CARTESIAN_POINT('Ctrl Pts',(1.99198379047747,-0.105372108024621,
6.71234787109334));
#11987=CARTESIAN_POINT('Ctrl Pts',(1.99242287791246,-0.0967149131407915,
6.71289362678897));
#11988=CARTESIAN_POINT('Ctrl Pts',(1.99304068217451,-0.0827331927704075,
6.71377764369478));
#11989=CARTESIAN_POINT('Ctrl Pts',(1.99325452252908,-0.0774102674565435,
6.71411480202458));
#11990=CARTESIAN_POINT('Ctrl Pts',(1.99362210987647,-0.0672451882657548,
6.71475985265493));
#11991=CARTESIAN_POINT('Ctrl Pts',(1.99377954458275,-0.0624031990861622,
6.71506762702889));
#11992=CARTESIAN_POINT('Ctrl Pts',(1.99409953282732,-0.0513187172266358,
6.71577339458607));
#11993=CARTESIAN_POINT('Ctrl Pts',(1.99425041397984,-0.0450759629419817,
6.71617175061494));
#11994=CARTESIAN_POINT('Ctrl Pts',(1.99462511715923,-0.0258319168961299,
6.71740246806978));
#11995=CARTESIAN_POINT('Ctrl Pts',(1.99475112292412,-0.0128292717293726,
6.71823788038833));
#11996=CARTESIAN_POINT('Ctrl Pts',(1.9947388541967,0.128286842604169,6.72734782198812));
#11997=CARTESIAN_POINT('Ctrl Pts',(1.98238600886794,0.256076005755822,6.73601469384028));
#11998=CARTESIAN_POINT('Ctrl Pts',(1.92826886430591,0.533605755829806,6.75561488815851));
#11999=CARTESIAN_POINT('Ctrl Pts',(1.88110249869077,0.68147895752933,6.766588682889));
#12000=CARTESIAN_POINT('Ctrl Pts',(1.80985798105033,0.838909550587931,6.77804094487477));
#12001=CARTESIAN_POINT('Ctrl Pts',(1.80217138918023,0.855297308823046,6.7792294736845));
#12002=CARTESIAN_POINT('Ctrl Pts',(1.79209328911896,0.876044435110608,6.78072746105763));
#12003=CARTESIAN_POINT('Ctrl Pts',(1.78990740758255,0.880501949323029,6.7810489044153));
#12004=CARTESIAN_POINT('Ctrl Pts',(1.78637598200101,0.88763584091704,6.78156265246885));
#12005=CARTESIAN_POINT('Ctrl Pts',(1.78504102913085,0.89031739270955,6.78175560640357));
#12006=CARTESIAN_POINT('Ctrl Pts',(1.78248373307362,0.895425421542024,6.78212284322593));
#12007=CARTESIAN_POINT('Ctrl Pts',(1.78126248785867,0.897852378535421,6.78229718825098));
#12008=CARTESIAN_POINT('Ctrl Pts',(1.77843517971906,0.903442559927139,6.78269846193021));
#12009=CARTESIAN_POINT('Ctrl Pts',(1.77682563488174,0.906603999137742,6.78292516938992));
#12010=CARTESIAN_POINT('Ctrl Pts',(1.7724843988219,0.915075008697134,6.78353206370028));
#12011=CARTESIAN_POINT('Ctrl Pts',(1.76973726086726,0.920376686624943,6.78391129962796));
#12012=CARTESIAN_POINT('Ctrl Pts',(1.74953795691009,0.958934318166979,6.78666560948518));
#12013=CARTESIAN_POINT('Ctrl Pts',(1.73117213129009,0.991706399218336,6.78898616812232));
#12014=CARTESIAN_POINT('Ctrl Pts',(1.66830589966521,1.09681002703077,6.79642544126453));
#12015=CARTESIAN_POINT('Ctrl Pts',(1.62010955898059,1.16682657540779,6.80137882115103));
#12016=CARTESIAN_POINT('Ctrl Pts',(1.50528263557822,1.31274692867956,6.81216106285884));
#12017=CARTESIAN_POINT('Ctrl Pts',(1.43706274274468,1.38709403816706,6.81796951597042));
#12018=CARTESIAN_POINT('Ctrl Pts',(1.32607580268801,1.49103403342782,6.82700590066267));
#12019=CARTESIAN_POINT('Ctrl Pts',(1.28729359631978,1.52464229070176,6.83009591377815));
#12020=CARTESIAN_POINT('Ctrl Pts',(1.22335770152675,1.57586854469316,6.83512432904677));
#12021=CARTESIAN_POINT('Ctrl Pts',(1.19901728102899,1.59446641119766,6.837024267462));
#12022=CARTESIAN_POINT('Ctrl Pts',(1.16722155833814,1.61762084333542,6.83949265876285));
#12023=CARTESIAN_POINT('Ctrl Pts',(1.1601504069946,1.62269972216716,6.8400407708087));
#12024=CARTESIAN_POINT('Ctrl Pts',(1.14869230958585,1.63081636324019,6.84092768801521));
#12025=CARTESIAN_POINT('Ctrl Pts',(1.1443259729406,1.63388313519194,6.84126537702318));
#12026=CARTESIAN_POINT('Ctrl Pts',(1.13597343610338,1.63969977931773,6.84191083315588));
#12027=CARTESIAN_POINT('Ctrl Pts',(1.1319894179478,1.64245273015748,6.84221847978438));
#12028=CARTESIAN_POINT('Ctrl Pts',(1.12285832735404,1.64871329673649,6.84292309309018));
#12029=CARTESIAN_POINT('Ctrl Pts',(1.11770479145757,1.65221135326027,6.84332041835098));
#12030=CARTESIAN_POINT('Ctrl Pts',(1.10181042283158,1.66289154877919,6.84454480659798));
#12031=CARTESIAN_POINT('Ctrl Pts',(1.09101629209933,1.66999339764401,6.8453748750289));
#12032=CARTESIAN_POINT('Ctrl Pts',(0.987393192092796,1.73673734789289,6.8533312104813));
#12033=CARTESIAN_POINT('Ctrl Pts',(0.889851419589409,1.78867518848476,6.86074375154518));
#12034=CARTESIAN_POINT('Ctrl Pts',(0.630523920453439,1.90027829728847,6.88019768047408));
#12035=CARTESIAN_POINT('Ctrl Pts',(0.464388405942447,1.94755291589205,6.89247013574457));
#12036=CARTESIAN_POINT('Ctrl Pts',(0.275845800696351,1.97567276133391,6.90511150412131));
#12037=CARTESIAN_POINT('Ctrl Pts',(0.257404482929136,1.97815994281335,6.90633384367969));
#12038=CARTESIAN_POINT('Ctrl Pts',(0.233953680755479,1.98098923890008,6.90786808080435));
#12039=CARTESIAN_POINT('Ctrl Pts',(0.228974786452716,1.98157090155009,6.90819266838026));
#12040=CARTESIAN_POINT('Ctrl Pts',(0.221006445941902,1.98247137455274,6.90871025032497));
#12041=CARTESIAN_POINT('Ctrl Pts',(0.21801842097341,1.98280220104763,6.90890391085958));
#12042=CARTESIAN_POINT('Ctrl Pts',(0.212331536604923,1.98341882777876,6.90927166533526));
#12043=CARTESIAN_POINT('Ctrl Pts',(0.209632875255926,1.98370587172527,6.90944582481277));
#12044=CARTESIAN_POINT('Ctrl Pts',(0.203425952773704,1.98435326532506,6.90984558718963));
#12045=CARTESIAN_POINT('Ctrl Pts',(0.199917318455736,1.98470981912138,6.91007097438661));
#12046=CARTESIAN_POINT('Ctrl Pts',(0.188751890948206,1.98581456126663,6.91078639524413));
#12047=CARTESIAN_POINT('Ctrl Pts',(0.181091590339512,1.98652777191804,6.91127450121112));
#12048=CARTESIAN_POINT('Ctrl Pts',(0.0585558306538583,1.99722174846652,
6.91904154560142));
#12049=CARTESIAN_POINT('Ctrl Pts',(-0.0569880609261623,1.9972692312399,
6.925798700472));
#12050=CARTESIAN_POINT('Ctrl Pts',(-0.274174718596705,1.97848259156458,
6.93846928754536));
#12051=CARTESIAN_POINT('Ctrl Pts',(-0.375606069714301,1.96175541427916,
6.94437674922504));
#12052=CARTESIAN_POINT('Ctrl Pts',(-0.546187912683751,1.91990474241444,
6.95479462237053));
#12053=CARTESIAN_POINT('Ctrl Pts',(-0.616062822790427,1.89863642479476,
6.95920524830631));
#12054=CARTESIAN_POINT('Ctrl Pts',(-0.700140637813496,1.86791435743031,
6.96477102059672));
#12055=CARTESIAN_POINT('Ctrl Pts',(-0.715599497257305,1.86204680203107,
6.96580525195011));
#12056=CARTESIAN_POINT('Ctrl Pts',(-0.737388336406335,1.85346523907365,
6.9672791772467));
#12057=CARTESIAN_POINT('Ctrl Pts',(-0.743780236237131,1.85090948168201,
6.9677135547612));
#12058=CARTESIAN_POINT('Ctrl Pts',(-0.754743830501469,1.84645980164953,
6.96846209750261));
#12059=CARTESIAN_POINT('Ctrl Pts',(-0.75932197194156,1.84458184719259,6.96877572113332));
#12060=CARTESIAN_POINT('Ctrl Pts',(-0.768043538058219,1.84096628790879,
6.96937521434914));
#12061=CARTESIAN_POINT('Ctrl Pts',(-0.772188177967852,1.83923167840067,
6.96966098075384));
#12062=CARTESIAN_POINT('Ctrl Pts',(-0.78184452241162,1.83515192391297,6.97032883639506));
#12063=CARTESIAN_POINT('Ctrl Pts',(-0.787351571854947,1.83279593574103,
6.97071129301806));
#12064=CARTESIAN_POINT('Ctrl Pts',(-0.806243720121482,1.82461276525473,
6.97202880811448));
#12065=CARTESIAN_POINT('Ctrl Pts',(-0.819575156000233,1.81866358191567,
6.97296802383439));
#12066=CARTESIAN_POINT('Ctrl Pts',(-0.930510687918328,1.76769087960372,
6.98086496092724));
#12067=CARTESIAN_POINT('Ctrl Pts',(-1.02437783155736,1.71499982243722,6.9880919074526));
#12068=CARTESIAN_POINT('Ctrl Pts',(-1.25623949497343,1.55899788585439,7.00734832448742));
#12069=CARTESIAN_POINT('Ctrl Pts',(-1.38592543961186,1.44493033539489,7.01961954560327));
#12070=CARTESIAN_POINT('Ctrl Pts',(-1.51166442290954,1.30163191360699,7.03226239542534));
#12071=CARTESIAN_POINT('Ctrl Pts',(-1.52376125153095,1.28744967909363,7.03348688447422));
#12072=CARTESIAN_POINT('Ctrl Pts',(-1.53885912746847,1.26923808039028,7.0350234177662));
#12073=CARTESIAN_POINT('Ctrl Pts',(-1.54204568694168,1.26536469826562,7.03534819782987));
#12074=CARTESIAN_POINT('Ctrl Pts',(-1.5471191920912,1.25915003445405,7.03586601183961));
#12075=CARTESIAN_POINT('Ctrl Pts',(-1.54901548589635,1.25681646573801,7.03605971301805));
#12076=CARTESIAN_POINT('Ctrl Pts',(-1.55261313177231,1.25236871157321,7.0364274949243));
#12077=CARTESIAN_POINT('Ctrl Pts',(-1.55431542511603,1.25025536831757,7.03660164139576));
#12078=CARTESIAN_POINT('Ctrl Pts',(-1.55821927877015,1.2453885617818,7.03700130685573));
#12079=CARTESIAN_POINT('Ctrl Pts',(-1.5604178545082,1.24263273349234,7.03722661048264));
#12080=CARTESIAN_POINT('Ctrl Pts',(-1.56738662798207,1.23384999036367,7.03794150362382));
#12081=CARTESIAN_POINT('Ctrl Pts',(-1.57212937496593,1.22780123524641,7.03842916944329));
#12082=CARTESIAN_POINT('Ctrl Pts',(-1.64775113496999,1.13019891928993,7.04622590443198));
#12083=CARTESIAN_POINT('Ctrl Pts',(-1.71057367642031,1.03265662672429,7.05300881891232));
#12084=CARTESIAN_POINT('Ctrl Pts',(-1.81237929514299,0.839531986095422,
7.06569672327122));
#12085=CARTESIAN_POINT('Ctrl Pts',(-1.85311402592373,0.745318816234449,
7.07159587099584));
#12086=CARTESIAN_POINT('Ctrl Pts',(-1.90382021315251,0.597795063367899,
7.08084994018711));
#12087=CARTESIAN_POINT('Ctrl Pts',(-1.9191679968745,0.546519776918832,7.0840675044448));
#12088=CARTESIAN_POINT('Ctrl Pts',(-1.94026607927825,0.464103544249463,
7.08928498010321));
#12089=CARTESIAN_POINT('Ctrl Pts',(-1.94736888644038,0.43333451757863,7.09124259108606));
#12090=CARTESIAN_POINT('Ctrl Pts',(-1.95551325494937,0.393792961562603,
7.09377581024684));
#12091=CARTESIAN_POINT('Ctrl Pts',(-1.95723127799705,0.38516322162594,7.09432972066377));
#12092=CARTESIAN_POINT('Ctrl Pts',(-1.95990318425386,0.371262389593682,
7.09522375683155));
#12093=CARTESIAN_POINT('Ctrl Pts',(-1.96089304246371,0.365998263219489,
7.09556273333203));
#12094=CARTESIAN_POINT('Ctrl Pts',(-1.9627365468652,0.355972210274397,7.0962091591243));
#12095=CARTESIAN_POINT('Ctrl Pts',(-1.96359409667029,0.351211033044341,
7.09651648161124));
#12096=CARTESIAN_POINT('Ctrl Pts',(-1.96550931660985,0.340351288999826,
7.09721826504437));
#12097=CARTESIAN_POINT('Ctrl Pts',(-1.96655593439504,0.334250847526576,
7.09761307429341));
#12098=CARTESIAN_POINT('Ctrl Pts',(-1.96966706715817,0.31559637624988,7.09882219456842));
#12099=CARTESIAN_POINT('Ctrl Pts',(-1.97163985158742,0.303027575170243,
7.09963940331373));
#12100=CARTESIAN_POINT('Ctrl Pts',(-1.9877290618664,0.193704402903063,7.10677064894761));
#12101=CARTESIAN_POINT('Ctrl Pts',(-1.99483182184317,0.0960674158499719,
7.11330712457486));
#12102=CARTESIAN_POINT('Ctrl Pts',(-1.9945866700246,-0.194289774984962,
7.13320902369089));
#12103=CARTESIAN_POINT('Ctrl Pts',(-1.9665315913241,-0.385843753873489,
7.14703282624318));
#12104=CARTESIAN_POINT('Ctrl Pts',(-1.90798583330162,-0.582035259283457,
7.16050168284247));
#12105=CARTESIAN_POINT('Ctrl Pts',(-1.90440764541565,-0.593638375583651,
7.16129512512014));
#12106=CARTESIAN_POINT('Ctrl Pts',(-1.89938014469388,-0.609427794194555,
7.16236986835138));
#12107=CARTESIAN_POINT('Ctrl Pts',(-1.89802260062614,-0.613642712680085,
7.1626562810746));
#12108=CARTESIAN_POINT('Ctrl Pts',(-1.89584893660257,-0.620315305104654,
7.16310888888343));
#12109=CARTESIAN_POINT('Ctrl Pts',(-1.89504205724023,-0.622775938555268,
7.16327562102889));
#12110=CARTESIAN_POINT('Ctrl Pts',(-1.89337435221628,-0.62782846675722,
7.1636176100584));
#12111=CARTESIAN_POINT('Ctrl Pts',(-1.89251299685581,-0.630420159979779,
7.1637928313699));
#12112=CARTESIAN_POINT('Ctrl Pts',(-1.8904715829434,-0.636520588967075,
7.16420481309576));
#12113=CARTESIAN_POINT('Ctrl Pts',(-1.88928706785623,-0.640027844601951,
7.16444131035098));
#12114=CARTESIAN_POINT('Ctrl Pts',(-1.88537086808901,-0.651517794793943,
7.16521497170818));
#12115=CARTESIAN_POINT('Ctrl Pts',(-1.88259825426532,-0.659486592935013,
7.16574977148564));
#12116=CARTESIAN_POINT('Ctrl Pts',(-1.84700096143439,-0.759742994455694,
7.1724586506003));
#12117=CARTESIAN_POINT('Ctrl Pts',(-1.80746730943883,-0.849523101789957,
7.17826050963938));
#12118=CARTESIAN_POINT('Ctrl Pts',(-1.72508194445567,-1.00455938966159,
7.18850896035907));
#12119=CARTESIAN_POINT('Ctrl Pts',(-1.68470758033952,-1.07089113462028,
7.19297744615205));
#12120=CARTESIAN_POINT('Ctrl Pts',(-1.57257247560681,-1.23301790181466,
7.20447462146601));
#12121=CARTESIAN_POINT('Ctrl Pts',(-1.49588371763748,-1.32500682946709,
7.21157044691108));
#12122=CARTESIAN_POINT('Ctrl Pts',(-1.40224357760754,-1.41877042545384,
7.21984136981117));
#12123=CARTESIAN_POINT('Ctrl Pts',(-1.39296748642958,-1.42787889545759,
7.22065663746208));
#12124=CARTESIAN_POINT('Ctrl Pts',(-1.37910531737959,-1.44122693392285,
7.22186937015431));
#12125=CARTESIAN_POINT('Ctrl Pts',(-1.37458716874236,-1.44553680879389,
7.22226377534085));
#12126=CARTESIAN_POINT('Ctrl Pts',(-1.3665277547429,-1.45315275454438,7.22296582116136));
#12127=CARTESIAN_POINT('Ctrl Pts',(-1.36299452494478,-1.45646728655837,
7.22327309401369));
#12128=CARTESIAN_POINT('Ctrl Pts',(-1.35555046928034,-1.46339976483327,
7.22391944718087));
#12129=CARTESIAN_POINT('Ctrl Pts',(-1.35163715840075,-1.46701497524824,
7.22425864082987));
#12130=CARTESIAN_POINT('Ctrl Pts',(-1.34131760137602,-1.47647208657606,
7.22515159113617));
#12131=CARTESIAN_POINT('Ctrl Pts',(-1.33488772411706,-1.48228792421194,
7.22570644482831));
#12132=CARTESIAN_POINT('Ctrl Pts',(-1.30583911040822,-1.50822016130144,
7.22820654577537));
#12133=CARTESIAN_POINT('Ctrl Pts',(-1.28280317585141,-1.52786114609097,
7.23017145725435));
#12134=CARTESIAN_POINT('Ctrl Pts',(-1.22018484864454,-1.57883639412306,
7.23546966910293));
#12135=CARTESIAN_POINT('Ctrl Pts',(-1.17984700709602,-1.60920344953893,
7.23883919118132));
#12136=CARTESIAN_POINT('Ctrl Pts',(-1.05616927384214,-1.69515867901641,
7.24904047659767));
#12137=CARTESIAN_POINT('Ctrl Pts',(-0.969754322193277,-1.74603256559661,
7.25600943872138));
#12138=CARTESIAN_POINT('Ctrl Pts',(-0.769562514334622,-1.84442805855687,
7.27157312375087));
#12139=CARTESIAN_POINT('Ctrl Pts',(-0.65444006442421,-1.88834768232673,
7.28014732982795));
#12140=CARTESIAN_POINT('Ctrl Pts',(-0.528717325381184,-1.92341951351136,
7.28866878727077));
#12141=CARTESIAN_POINT('Ctrl Pts',(-0.521428903465127,-1.92540814846505,
7.28915982412871));
#12142=CARTESIAN_POINT('Ctrl Pts',(-0.510746864418605,-1.92825762214947,
7.28987497815223));
#12143=CARTESIAN_POINT('Ctrl Pts',(-0.507362108399073,-1.92915098121202,
7.29010092298121));
#12144=CARTESIAN_POINT('Ctrl Pts',(-0.501352673830008,-1.93072017763888,
7.29050087953229));
#12145=CARTESIAN_POINT('Ctrl Pts',(-0.498728951708093,-1.93139958086799,
7.29067509653724));
#12146=CARTESIAN_POINT('Ctrl Pts',(-0.493178541450453,-1.93282477481158,
7.29104278676217));
#12147=CARTESIAN_POINT('Ctrl Pts',(-0.490251549938585,-1.93356926484485,
7.29123618407431));
#12148=CARTESIAN_POINT('Ctrl Pts',(-0.482401561484502,-1.93554696464492,
7.29175354268274));
#12149=CARTESIAN_POINT('Ctrl Pts',(-0.477475489111115,-1.93676804949092,
7.2920768093821));
#12150=CARTESIAN_POINT('Ctrl Pts',(-0.45380645602142,-1.94253938509753,
7.29362363067294));
#12151=CARTESIAN_POINT('Ctrl Pts',(-0.435002038710527,-1.9468366278307,
7.29483322377454));
#12152=CARTESIAN_POINT('Ctrl Pts',(-0.382311522558341,-1.95807602382593,
7.2981763187303));
#12153=CARTESIAN_POINT('Ctrl Pts',(-0.348301574264663,-1.96441088430794,
7.30028117018476));
#12154=CARTESIAN_POINT('Ctrl Pts',(-0.223538339647063,-1.98430743217364,
7.30786615025344));
#12155=CARTESIAN_POINT('Ctrl Pts',(-0.132039425032454,-1.99248920695555,
7.31317080884233));
#12156=CARTESIAN_POINT('Ctrl Pts',(0.115340367407889,-1.99748769174982,
7.32752115855705));
#12157=CARTESIAN_POINT('Ctrl Pts',(0.270785521303748,-1.9824042001089,7.33659109858792));
#12158=CARTESIAN_POINT('Ctrl Pts',(0.435177562778028,-1.94674246144229,
7.34709544743529));
#12159=CARTESIAN_POINT('Ctrl Pts',(0.447442143776204,-1.94396019474529,
7.34788438196233));
#12160=CARTESIAN_POINT('Ctrl Pts',(0.465674161534954,-1.93964251621462,
7.34906533275389));
#12161=CARTESIAN_POINT('Ctrl Pts',(0.471662282310595,-1.93819508963639,
7.34945451977796));
#12162=CARTESIAN_POINT('Ctrl Pts',(0.482337316233643,-1.93556235946276,
7.35015071420359));
#12163=CARTESIAN_POINT('Ctrl Pts',(0.487026826562608,-1.93438770765701,
7.35045737589868));
#12164=CARTESIAN_POINT('Ctrl Pts',(0.496918666775499,-1.93187169979591,
7.35110599939883));
#12165=CARTESIAN_POINT('Ctrl Pts',(0.502119932709991,-1.93052635260604,
7.35144808813377));
#12166=CARTESIAN_POINT('Ctrl Pts',(0.515895166759187,-1.92690384754689,
7.35235686498088));
#12167=CARTESIAN_POINT('Ctrl Pts',(0.524459411377618,-1.92459049732045,
7.35292472175721));
#12168=CARTESIAN_POINT('Ctrl Pts',(0.564159956717498,-1.91358202795201,
7.35557061230818));
#12169=CARTESIAN_POINT('Ctrl Pts',(0.59509586627981,-1.90418836792565,7.35767123299051));
#12170=CARTESIAN_POINT('Ctrl Pts',(0.678283802698345,-1.87670328919761,
7.3634298160512));
#12171=CARTESIAN_POINT('Ctrl Pts',(0.730030982862083,-1.85718550045609,
7.36713222951314));
#12172=CARTESIAN_POINT('Ctrl Pts',(0.876531237683069,-1.79485981503344,
7.37795721683183));
#12173=CARTESIAN_POINT('Ctrl Pts',(0.968832756592229,-1.74676518811115,
7.38521460075528));
#12174=CARTESIAN_POINT('Ctrl Pts',(1.11743386317596,-1.65392076745725,7.3974335506059));
#12175=CARTESIAN_POINT('Ctrl Pts',(1.17584254626516,-1.61291904942451,7.40238922845445));
#12176=CARTESIAN_POINT('Ctrl Pts',(1.23889348613665,-1.56340935694367,7.40782663950981));
#12177=CARTESIAN_POINT('Ctrl Pts',(1.24581779177863,-1.55789727578309,7.4084250027478));
#12178=CARTESIAN_POINT('Ctrl Pts',(1.27878078056078,-1.53129683297923,7.41127852426397));
#12179=CARTESIAN_POINT('Ctrl Pts',(1.30432389837575,-1.50959920871224,7.41350492517378));
#12180=CARTESIAN_POINT('Ctrl Pts',(1.33361065375467,-1.48342288584133,7.41606386009804));
#12181=CARTESIAN_POINT('Ctrl Pts',(1.33789470271329,-1.4795602726768,7.41643833875314));
#12182=CARTESIAN_POINT('Ctrl Pts',(1.34474229004939,-1.47333224405047,7.41703707194208));
#12183=CARTESIAN_POINT('Ctrl Pts',(1.34731644456302,-1.47097862889667,7.41726218735919));
#12184=CARTESIAN_POINT('Ctrl Pts',(1.35187856928799,-1.46678533962336,7.41766120282715));
#12185=CARTESIAN_POINT('Ctrl Pts',(1.35386897879026,-1.46494835651323,7.417835304758));
#12186=CARTESIAN_POINT('Ctrl Pts',(1.35807607523794,-1.461049657063,7.41820332760344));
#12187=CARTESIAN_POINT('Ctrl Pts',(1.36029180606423,-1.45898695305727,7.41839717038853));
#12188=CARTESIAN_POINT('Ctrl Pts',(1.36623266375402,-1.45343109549215,7.41891698177227));
#12189=CARTESIAN_POINT('Ctrl Pts',(1.36994911795889,-1.44992863839659,7.41924224425486));
#12190=CARTESIAN_POINT('Ctrl Pts',(1.3878943416308,-1.4328861246421,7.42081344153227));
#12191=CARTESIAN_POINT('Ctrl Pts',(1.40193665605217,-1.41915010929218,7.42204487728735));
#12192=CARTESIAN_POINT('Ctrl Pts',(1.44077374141241,-1.380020997941,7.42546427423165));
#12193=CARTESIAN_POINT('Ctrl Pts',(1.46509806120008,-1.35416945541063,7.427621975579));
#12194=CARTESIAN_POINT('Ctrl Pts',(1.55230838588195,-1.2563810260175,7.43548021356458));
#12195=CARTESIAN_POINT('Ctrl Pts',(1.61069559112383,-1.1806001642617,7.44099283948859));
#12196=CARTESIAN_POINT('Ctrl Pts',(1.66907656893195,-1.09238988289051,7.44712921610931));
#12197=CARTESIAN_POINT('Ctrl Pts',(1.67465777629022,-1.08381436634872,7.44772295023516));
#12198=CARTESIAN_POINT('Ctrl Pts',(1.75550845940798,-0.957471749850599,
7.45643372225907));
#12199=CARTESIAN_POINT('Ctrl Pts',(1.81825156134243,-0.832174999067098,
7.46464528927353));
#12200=CARTESIAN_POINT('Ctrl Pts',(1.87192306876504,-0.689273735359299,
7.47417382146523));
#12201=CARTESIAN_POINT('Ctrl Pts',(1.87634509248304,-0.677143514376843,
7.47498354721903));
#12202=CARTESIAN_POINT('Ctrl Pts',(1.88272469071956,-0.659100957884343,
7.47618959778913));
#12203=CARTESIAN_POINT('Ctrl Pts',(1.88477289524618,-0.653220839874413,
7.47658291199912));
#12204=CARTESIAN_POINT('Ctrl Pts',(1.88836494851416,-0.642750987722597,
7.47728372835545));
#12205=CARTESIAN_POINT('Ctrl Pts',(1.88991968551728,-0.638165019890582,
7.47759086734001));
#12206=CARTESIAN_POINT('Ctrl Pts',(1.8931527342253,-0.62851314025626,7.47823766626295));
#12207=CARTESIAN_POINT('Ctrl Pts',(1.89482744306627,-0.623446070378056,
7.47857744230303));
#12208=CARTESIAN_POINT('Ctrl Pts',(1.89918202328465,-0.610091039795128,
7.47947357806876));
#12209=CARTESIAN_POINT('Ctrl Pts',(1.90182795345701,-0.601792211534336,
7.48003104910718));
#12210=CARTESIAN_POINT('Ctrl Pts',(1.91354541720835,-0.56419178736214,7.4825598149577));
#12211=CARTESIAN_POINT('Ctrl Pts',(1.92199428672097,-0.534701995675028,
7.48455133157076));
#12212=CARTESIAN_POINT('Ctrl Pts',(1.9427742309293,-0.455300257242834,7.48993876774639));
#12213=CARTESIAN_POINT('Ctrl Pts',(1.95386073223267,-0.405089515106551,
7.49337242930983));
#12214=CARTESIAN_POINT('Ctrl Pts',(1.98092517562932,-0.255228144499492,
7.50369486797471));
#12215=CARTESIAN_POINT('Ctrl Pts',(1.99129584600062,-0.154736879579646,
7.51072053506725));
#12216=CARTESIAN_POINT('Ctrl Pts',(1.99728343870076,0.0667645588387559,
7.52618018596327));
#12217=CARTESIAN_POINT('Ctrl Pts',(1.98958588043622,0.187493772365523,7.5345905543698));
#12218=CARTESIAN_POINT('Ctrl Pts',(1.9699624920002,0.313563755208486,7.54292108234574));
#12219=CARTESIAN_POINT('Ctrl Pts',(1.96887450474531,0.320324267453869,7.54336636866715));
#12220=CARTESIAN_POINT('Ctrl Pts',(1.96718493119378,0.330488966526171,7.54403357140755));
#12221=CARTESIAN_POINT('Ctrl Pts',(1.96660928693717,0.333897324762621,7.5442569030128));
#12222=CARTESIAN_POINT('Ctrl Pts',(1.9655969214408,0.339798038862502,7.54464284884334));
#12223=CARTESIAN_POINT('Ctrl Pts',(1.9651643145003,0.342291077860937,7.54480569452101));
#12224=CARTESIAN_POINT('Ctrl Pts',(1.96424766385382,0.347514556546481,7.54514643121397));
#12225=CARTESIAN_POINT('Ctrl Pts',(1.96376266922329,0.35024481589118,7.54532426513538));
#12226=CARTESIAN_POINT('Ctrl Pts',(1.96257545985934,0.356848175993785,7.54575374694498));
#12227=CARTESIAN_POINT('Ctrl Pts',(1.96186746631204,0.360720253969869,7.54600506650521));
#12228=CARTESIAN_POINT('Ctrl Pts',(1.95935382546153,0.374241245638005,7.54688091734196));
#12229=CARTESIAN_POINT('Ctrl Pts',(1.95748838278438,0.383879100728014,7.54750213571959));
#12230=CARTESIAN_POINT('Ctrl Pts',(1.95279076986144,0.407224348149123,7.54900022816679));
#12231=CARTESIAN_POINT('Ctrl Pts',(1.949885291655,0.420916659710581,7.54987329915693));
#12232=CARTESIAN_POINT('Ctrl Pts',(1.93825608032229,0.473013595745383,7.55317779078762));
#12233=CARTESIAN_POINT('Ctrl Pts',(1.92853936526036,0.511189615960492,7.55556315091296));
#12234=CARTESIAN_POINT('Ctrl Pts',(1.89056007024004,0.643840770926139,7.5638031914185));
#12235=CARTESIAN_POINT('Ctrl Pts',(1.8564304918077,0.736489261720345,7.56947642422971));
#12236=CARTESIAN_POINT('Ctrl Pts',(1.75703781313496,0.954896110597521,7.58340853372254));
#12237=CARTESIAN_POINT('Ctrl Pts',(1.68498903147929,1.07694575235569,7.59170649840494));
#12238=CARTESIAN_POINT('Ctrl Pts',(1.59295945706711,1.20069731000528,7.60133334543289));
#12239=CARTESIAN_POINT('Ctrl Pts',(1.58516403279668,1.21097020557984,7.60214211985005));
#12240=CARTESIAN_POINT('Ctrl Pts',(1.57345963234088,1.2260877137306,7.60334702318699));
#12241=CARTESIAN_POINT('Ctrl Pts',(1.56962659733869,1.23099091786586,7.60374014991941));
#12242=CARTESIAN_POINT('Ctrl Pts',(1.56277078898525,1.23967675967138,7.60444075552367));
#12243=CARTESIAN_POINT('Ctrl Pts',(1.55975705724399,1.24346649696526,7.60474787202841));
#12244=CARTESIAN_POINT('Ctrl Pts',(1.55339176571419,1.25141123600155,7.60539474970155));
#12245=CARTESIAN_POINT('Ctrl Pts',(1.5500372696955,1.25556382594476,7.60573462745199));
#12246=CARTESIAN_POINT('Ctrl Pts',(1.54116098470617,1.26646214973071,7.60663131863999));
#12247=CARTESIAN_POINT('Ctrl Pts',(1.5356116211114,1.27318518000599,7.60718924588464));
#12248=CARTESIAN_POINT('Ctrl Pts',(1.51029214535424,1.30345326850397,7.60972303946187));
#12249=CARTESIAN_POINT('Ctrl Pts',(1.49002428157141,1.32657463127274,7.6117192262284));
#12250=CARTESIAN_POINT('Ctrl Pts',(1.43435084715314,1.38720025305192,7.61712237488871));
#12251=CARTESIAN_POINT('Ctrl Pts',(1.39801357631594,1.42381324897596,7.62056735014991));
#12252=CARTESIAN_POINT('Ctrl Pts',(1.28641579991935,1.5278634208877,7.63091109378776));
#12253=CARTESIAN_POINT('Ctrl Pts',(1.2074099424394,1.591034307249,7.63794668903852));
#12254=CARTESIAN_POINT('Ctrl Pts',(1.02458663839534,1.71572751954561,7.65338634756665));
#12255=CARTESIAN_POINT('Ctrl Pts',(0.91926443509452,1.77438970039164,7.66176633229916));
#12256=CARTESIAN_POINT('Ctrl Pts',(0.803008397587063,1.82599349694093,7.67007150315024));
#12257=CARTESIAN_POINT('Ctrl Pts',(0.796716196827393,1.82874767053753,7.67051817345978));
#12258=CARTESIAN_POINT('Ctrl Pts',(0.787231246477696,1.83284110384073,7.67118709766611));
#12259=CARTESIAN_POINT('Ctrl Pts',(0.784049111713108,1.83420460642279,7.67141077677652));
#12260=CARTESIAN_POINT('Ctrl Pts',(0.77853380724305,1.8365508658078,7.67179715877749));
#12261=CARTESIAN_POINT('Ctrl Pts',(0.776202299677492,1.83753747223605,7.67196009435165));
#12262=CARTESIAN_POINT('Ctrl Pts',(0.771368718279766,1.83957202125561,7.6722970451981));
#12263=CARTESIAN_POINT('Ctrl Pts',(0.768866380526226,1.84061930065361,7.67247101785099));
#12264=CARTESIAN_POINT('Ctrl Pts',(0.762844891113841,1.84312499463655,7.67288855335545));
#12265=CARTESIAN_POINT('Ctrl Pts',(0.759323659112666,1.84457844914495,7.6731318151839));
#12266=CARTESIAN_POINT('Ctrl Pts',(0.751798009799821,1.84765960046673,7.67364983723874));
#12267=CARTESIAN_POINT('Ctrl Pts',(0.74779241287204,1.84928438992299,7.67392442546535));
#12268=CARTESIAN_POINT('Ctrl Pts',(0.736741427233352,1.85372522192481,7.67467894707545));
#12269=CARTESIAN_POINT('Ctrl Pts',(0.729685119287649,1.85651414212947,7.67515733607856));
#12270=CARTESIAN_POINT('Ctrl Pts',(0.666922456711792,1.88090720403825,7.67938382986364));
#12271=CARTESIAN_POINT('Ctrl Pts',(0.610281647414656,1.90004085858221,7.68299927293976));
#12272=CARTESIAN_POINT('Ctrl Pts',(0.430727789222,1.951834785073,7.69409530373554));
#12273=CARTESIAN_POINT('Ctrl Pts',(0.305502023434583,1.9753118591386,7.70132961021421));
#12274=CARTESIAN_POINT('Ctrl Pts',(0.074688402749332,1.9960949308181,7.71491414429359));
#12275=CARTESIAN_POINT('Ctrl Pts',(-0.0300741819228045,1.99726419872849,
7.72117046548653));
#12276=CARTESIAN_POINT('Ctrl Pts',(-0.147248343016588,1.98934923586138,
7.72850192178656));
#12277=CARTESIAN_POINT('Ctrl Pts',(-0.160051361091155,1.98836012992434,
7.72930730650042));
#12278=CARTESIAN_POINT('Ctrl Pts',(-0.179033273300147,1.98670915086992,
7.73050812074171));
#12279=CARTESIAN_POINT('Ctrl Pts',(-0.185220237068421,1.98614189459371,
7.7309005779782));
#12280=CARTESIAN_POINT('Ctrl Pts',(-0.196222715304694,1.98508126797529,
7.73160043109354));
#12281=CARTESIAN_POINT('Ctrl Pts',(-0.201039295273785,1.98459925313573,
7.73190746743925));
#12282=CARTESIAN_POINT('Ctrl Pts',(-0.211169396991009,1.98354823622688,
7.73255462794128));
#12283=CARTESIAN_POINT('Ctrl Pts',(-0.216482474760609,1.98297540500871,
7.73289487040154));
#12284=CARTESIAN_POINT('Ctrl Pts',(-0.230481798875473,1.9814091300373,7.73379355535302));
#12285=CARTESIAN_POINT('Ctrl Pts',(-0.239163851510388,1.98037992524209,
7.73435312062968));
#12286=CARTESIAN_POINT('Ctrl Pts',(-0.278598851162377,1.9754420421766,7.73690506007576));
#12287=CARTESIAN_POINT('Ctrl Pts',(-0.309263450472154,1.97087404980394,
7.73891811286941));
#12288=CARTESIAN_POINT('Ctrl Pts',(-0.391207133474379,1.95670779418995,
7.74437813661366));
#12289=CARTESIAN_POINT('Ctrl Pts',(-0.44223403973368,1.94581003048356,7.74786411260748));
#12290=CARTESIAN_POINT('Ctrl Pts',(-0.595433162492025,1.90675411245586,
7.75858722276122));
#12291=CARTESIAN_POINT('Ctrl Pts',(-0.695838376719188,1.87244684474971,
7.76597842956949));
#12292=CARTESIAN_POINT('Ctrl Pts',(-0.897946628224816,1.78487872210169,
7.78134165407321));
#12293=CARTESIAN_POINT('Ctrl Pts',(-0.998769818620894,1.7304813526263,7.78928449099847));
#12294=CARTESIAN_POINT('Ctrl Pts',(-1.10075106228303,1.66356022475537,7.79725028667874));
#12295=CARTESIAN_POINT('Ctrl Pts',(-1.10709229512563,1.65934691282602,7.79774525247533));
#12296=CARTESIAN_POINT('Ctrl Pts',(-1.11636798956632,1.6531070107846,7.79846856928922));
#12297=CARTESIAN_POINT('Ctrl Pts',(-1.11932129240937,1.65110875537549,7.79869876244862));
#12298=CARTESIAN_POINT('Ctrl Pts',(-1.12445516726062,1.6476149824771,7.79909871353418));
#12299=CARTESIAN_POINT('Ctrl Pts',(-1.12663814375659,1.6461230352043,7.7992687114782));
#12300=CARTESIAN_POINT('Ctrl Pts',(-1.12882584223643,1.6446214702738,7.79943900766025));
#12301=CARTESIAN_POINT('Ctrl Pts',(-1.12883350313277,1.64461621200567,7.79943960400361));
#12302=CARTESIAN_POINT('Ctrl Pts',(-1.12884878447753,1.64460572307439,7.79944079354019));
#12303=CARTESIAN_POINT('Ctrl Pts',(-1.12885639273591,1.64460050077967,7.79944138578447));
#12304=CARTESIAN_POINT('Ctrl Pts',(-1.12887155391961,1.64459009401593,7.79944256596414));
#12305=CARTESIAN_POINT('Ctrl Pts',(-1.12887910629555,1.64458490992518,7.79944315385677));
#12306=CARTESIAN_POINT('Ctrl Pts',(-1.1288941564389,1.64457457907543,7.79944432538958));
#12307=CARTESIAN_POINT('Ctrl Pts',(-1.1289016535973,1.64456943273561,7.79944490898237));
#12308=CARTESIAN_POINT('Ctrl Pts',(-1.12891659392282,1.64455917696735,7.79944607196355));
#12309=CARTESIAN_POINT('Ctrl Pts',(-1.12892403648006,1.64455406795867,7.79944665130449));
#12310=CARTESIAN_POINT('Ctrl Pts',(-1.12893886834671,1.64454388634561,7.79944780583991));
#12311=CARTESIAN_POINT('Ctrl Pts',(-1.12894625698808,1.64453881420089,7.7994483809824));
#12312=CARTESIAN_POINT('Ctrl Pts',(-1.12896098144157,1.64452870603161,7.79944952715351));
#12313=CARTESIAN_POINT('Ctrl Pts',(-1.12896831670578,1.64452367038424,7.7994500981395));
#12314=CARTESIAN_POINT('Ctrl Pts',(-1.12898293515746,1.64451363469618,7.79945123605625));
#12315=CARTESIAN_POINT('Ctrl Pts',(-1.12899021768419,1.64450863511014,7.79945180293558));
#12316=CARTESIAN_POINT('Ctrl Pts',(-1.12900473129285,1.64449867111398,7.79945293268822));
#12317=CARTESIAN_POINT('Ctrl Pts',(-1.12901196169899,1.64449370716885,7.79945349550894));
#12318=CARTESIAN_POINT('Ctrl Pts',(-1.12902637157479,1.64448381410851,7.79945461718396));
#12319=CARTESIAN_POINT('Ctrl Pts',(-1.12903355041035,1.64447888542969,7.79945517598891));
#12320=CARTESIAN_POINT('Ctrl Pts',(-1.12904785782266,1.64446906243968,7.79945628968519));
#12321=CARTESIAN_POINT('Ctrl Pts',(-1.12905498568997,1.64446416861658,7.79945684452129));
#12322=CARTESIAN_POINT('Ctrl Pts',(-1.1290691917274,1.64445441495536,7.79945795032362));
#12323=CARTESIAN_POINT('Ctrl Pts',(-1.12907626917904,1.64444955561151,7.79945850123392));
#12324=CARTESIAN_POINT('Ctrl Pts',(-1.12909037504845,1.64443987045622,7.7994595992363));
#12325=CARTESIAN_POINT('Ctrl Pts',(-1.12909740268166,1.64443504518442,7.79946014626732));
#12326=CARTESIAN_POINT('Ctrl Pts',(-1.12911140940098,1.64442542784179,7.79946123654905));
#12327=CARTESIAN_POINT('Ctrl Pts',(-1.12911838773864,1.64442063628581,7.79946177974152));
#12328=CARTESIAN_POINT('Ctrl Pts',(-1.12913229651027,1.64441108593581,7.79946286239626));
#12329=CARTESIAN_POINT('Ctrl Pts',(-1.12913922613612,1.6444063276976,7.79946340179564));
#12330=CARTESIAN_POINT('Ctrl Pts',(-1.12915303793578,1.64439684367569,7.7994644768994));
#12331=CARTESIAN_POINT('Ctrl Pts',(-1.12915991935299,1.64439211841245,7.79946501254489));
#12332=CARTESIAN_POINT('Ctrl Pts',(-1.1291736353442,1.64438269992505,7.79946608018829));
#12333=CARTESIAN_POINT('Ctrl Pts',(-1.12918046910672,1.64437800725904,7.79946661212303));
#12334=CARTESIAN_POINT('Ctrl Pts',(-1.12919409029006,1.64436865362434,7.79946767238401));
#12335=CARTESIAN_POINT('Ctrl Pts',(-1.12920087691404,1.64436399320373,7.79946820064823));
#12336=CARTESIAN_POINT('Ctrl Pts',(-1.12921440430238,1.64435470373135,7.79946925360569));
#12337=CARTESIAN_POINT('Ctrl Pts',(-1.12922114426384,1.64435007523182,7.79946977823644));
#12338=CARTESIAN_POINT('Ctrl Pts',(-1.12923457904166,1.64434084911344,7.79947082398263));
#12339=CARTESIAN_POINT('Ctrl Pts',(-1.12924127293075,1.64433625213223,7.79947134502589));
#12340=CARTESIAN_POINT('Ctrl Pts',(-1.12925461583179,1.64432708886894,7.79947238361798));
#12341=CARTESIAN_POINT('Ctrl Pts',(-1.12926126403854,1.64432252314068,7.79947290110413));
#12342=CARTESIAN_POINT('Ctrl Pts',(-1.12927451638761,1.64431342182757,7.79947393264529));
#12343=CARTESIAN_POINT('Ctrl Pts',(-1.12928111951491,1.64430888694064,7.79947444662129));
#12344=CARTESIAN_POINT('Ctrl Pts',(-1.12929428204093,1.6442998470819,7.79947547116831));
#12345=CARTESIAN_POINT('Ctrl Pts',(-1.12930084054295,1.64429534272677,7.79947598166954));
#12346=CARTESIAN_POINT('Ctrl Pts',(-1.12931391423852,1.64428636364544,7.79947699929973));
#12347=CARTESIAN_POINT('Ctrl Pts',(-1.12932042855701,1.64428188952106,7.79947750636059));
#12348=CARTESIAN_POINT('Ctrl Pts',(-1.12933341448615,1.64427297049101,7.79947851715683));
#12349=CARTESIAN_POINT('Ctrl Pts',(-1.12933988513022,1.64426852625001,7.79947902081697));
#12350=CARTESIAN_POINT('Ctrl Pts',(-1.12935278414045,1.64425966669371,7.79948002484528));
#12351=CARTESIAN_POINT('Ctrl Pts',(-1.12935921155788,1.6442552520308,7.79948052513959));
#12352=CARTESIAN_POINT('Ctrl Pts',(-1.129372024619,1.64424645128663,7.79948152247549));
#12353=CARTESIAN_POINT('Ctrl Pts',(-1.12937840927727,1.64424206588296,7.79948201944037));
#12354=CARTESIAN_POINT('Ctrl Pts',(-1.12939113730432,1.64423332332683,7.79948301015514));
#12355=CARTESIAN_POINT('Ctrl Pts',(-1.12939747967533,1.64422896686044,7.79948350382736));
#12356=CARTESIAN_POINT('Ctrl Pts',(-1.12941012345138,1.64422028195881,7.79948448798199));
#12357=CARTESIAN_POINT('Ctrl Pts',(-1.12941642390336,1.64421595417894,7.79948497839023));
#12358=CARTESIAN_POINT('Ctrl Pts',(-1.12942898457574,1.64420732614796,7.79948595607408));
#12359=CARTESIAN_POINT('Ctrl Pts',(-1.12943524365278,1.64420302668297,7.7994864432607));
#12360=CARTESIAN_POINT('Ctrl Pts',(-1.12944772185695,1.64419445509034,7.79948741452328));
#12361=CARTESIAN_POINT('Ctrl Pts',(-1.12945393996183,1.64419018366563,7.79948789851966));
#12362=CARTESIAN_POINT('Ctrl Pts',(-1.12946633655248,1.64418166792836,7.79948886342754));
#12363=CARTESIAN_POINT('Ctrl Pts',(-1.12947251404302,1.64417742430017,7.79948934426156));
#12364=CARTESIAN_POINT('Ctrl Pts',(-1.12948483010306,1.6441689636784,7.79949030289906));
#12365=CARTESIAN_POINT('Ctrl Pts',(-1.1294909674934,1.64416474749555,7.79949078061075));
#12366=CARTESIAN_POINT('Ctrl Pts',(-1.12950320365697,1.64415634155764,7.79949173302728));
#12367=CARTESIAN_POINT('Ctrl Pts',(-1.129509301343,1.64415215255014,7.79949220764749));
#12368=CARTESIAN_POINT('Ctrl Pts',(-1.12952145844548,1.6441438007261,7.79949315390811));
#12369=CARTESIAN_POINT('Ctrl Pts',(-1.12952751680522,1.6441396386362,7.79949362546628));
#12370=CARTESIAN_POINT('Ctrl Pts',(-1.12953959574272,1.64413134031427,7.79949456564078));
#12371=CARTESIAN_POINT('Ctrl Pts',(-1.12954561519649,1.6441272048551,7.79949503416964));
#12372=CARTESIAN_POINT('Ctrl Pts',(-1.1295576167294,1.64411895951666,7.79949596831725));
#12373=CARTESIAN_POINT('Ctrl Pts',(-1.12956359766323,1.6441148504249,7.79949643384687));
#12374=CARTESIAN_POINT('Ctrl Pts',(-1.12957553990149,1.64410664563144,7.79949736337723));
#12375=CARTESIAN_POINT('Ctrl Pts',(-1.12958150011876,1.64410255067646,7.7994978272935));
#12376=CARTESIAN_POINT('Ctrl Pts',(-1.12959331502839,1.64409443317423,7.7994987469112));
#12377=CARTESIAN_POINT('Ctrl Pts',(-1.12959922053442,1.6440903757152,7.79949920656787));
#12378=CARTESIAN_POINT('Ctrl Pts',(-1.12961099424549,1.64408228633193,7.7995001229769));
#12379=CARTESIAN_POINT('Ctrl Pts',(-1.12961686242387,1.64407825442658,7.79950057972719));
#12380=CARTESIAN_POINT('Ctrl Pts',(-1.1321026690405,1.6423702879494,7.79969406254519));
#12381=CARTESIAN_POINT('Ctrl Pts',(-1.13457876906356,1.64066073064219,7.7998867032622));
#12382=CARTESIAN_POINT('Ctrl Pts',(-1.13967656474752,1.63712403371453,7.80028315440653));
#12383=CARTESIAN_POINT('Ctrl Pts',(-1.1422977591648,1.63529618227094,7.80048691606186));
#12384=CARTESIAN_POINT('Ctrl Pts',(-1.14887621928734,1.63068525484135,7.80099811394823));
#12385=CARTESIAN_POINT('Ctrl Pts',(-1.15282780041494,1.6278940479461,7.80130501243175));
#12386=CARTESIAN_POINT('Ctrl Pts',(-1.1640207951718,1.61992665889257,7.80217394976679));
#12387=CARTESIAN_POINT('Ctrl Pts',(-1.17123787698936,1.6147162704329,7.80273379357753));
#12388=CARTESIAN_POINT('Ctrl Pts',(-1.24450432988161,1.56107170669042,7.80841548203265));
#12389=CARTESIAN_POINT('Ctrl Pts',(-1.30755434317338,1.50865530586343,7.81329181922092));
#12390=CARTESIAN_POINT('Ctrl Pts',(-1.44818887621015,1.3762792306951,7.82460687486772));
#12391=CARTESIAN_POINT('Ctrl Pts',(-1.52265231535625,1.2934163807026,7.83096862600547));
#12392=CARTESIAN_POINT('Ctrl Pts',(-1.59495836704808,1.19800153550023,7.83801163344411));
#12393=CARTESIAN_POINT('Ctrl Pts',(-1.60005083122588,1.19119150737489,7.8385128050549));
#12394=CARTESIAN_POINT('Ctrl Pts',(-1.62756465856201,1.15390315248315,7.84124956555442));
#12395=CARTESIAN_POINT('Ctrl Pts',(-1.64915803002073,1.1228253570584,7.84350391461993));
#12396=CARTESIAN_POINT('Ctrl Pts',(-1.69851187560312,1.04729637387332,7.84894666167827));
#12397=CARTESIAN_POINT('Ctrl Pts',(-1.72542882828057,1.00233073420163,7.8521589330171));
#12398=CARTESIAN_POINT('Ctrl Pts',(-1.75526152709308,0.947724318018689,
7.85605225274669));
#12399=CARTESIAN_POINT('Ctrl Pts',(-1.75991572893285,0.939053264177024,
7.85667022954452));
#12400=CARTESIAN_POINT('Ctrl Pts',(-1.76738783374599,0.924881613775711,
7.85767998412094));
#12401=CARTESIAN_POINT('Ctrl Pts',(-1.77024470947094,0.919401664979605,
7.85807038084249));
#12402=CARTESIAN_POINT('Ctrl Pts',(-1.77529200205676,0.909609401506133,
7.85876792543009));
#12403=CARTESIAN_POINT('Ctrl Pts',(-1.77749229614253,0.905302210509712,
7.85907472247838));
#12404=CARTESIAN_POINT('Ctrl Pts',(-1.78209865543059,0.896203488400793,
7.85972278901815));
#12405=CARTESIAN_POINT('Ctrl Pts',(-1.78450110669329,0.891410180328937,
7.86006418220649));
#12406=CARTESIAN_POINT('Ctrl Pts',(-1.79080568035827,0.878703829739025,
7.86096915678257));
#12407=CARTESIAN_POINT('Ctrl Pts',(-1.79467464395518,0.870774553714571,
7.86153388946256));
#12408=CARTESIAN_POINT('Ctrl Pts',(-1.81225485171914,0.834129780455785,
7.86414396085249));
#12409=CARTESIAN_POINT('Ctrl Pts',(-1.82532968640814,0.805115817549437,
7.86621114827469));
#12410=CARTESIAN_POINT('Ctrl Pts',(-1.85873901079451,0.725976562968527,
7.87185508999053));
#12411=CARTESIAN_POINT('Ctrl Pts',(-1.87773676530586,0.67531951160803,7.87547415614104));
#12412=CARTESIAN_POINT('Ctrl Pts',(-1.92440635302603,0.533606801034589,
7.8856092143321));
#12413=CARTESIAN_POINT('Ctrl Pts',(-1.94765785277755,0.441250752980717,
7.89223205196852));
#12414=CARTESIAN_POINT('Ctrl Pts',(-1.98454972412004,0.232778735486161,
7.90700343017225));
#12415=CARTESIAN_POINT('Ctrl Pts',(-1.99476344435805,0.116390624358837,
7.91513345943431));
#12416=CARTESIAN_POINT('Ctrl Pts',(-1.99474998671859,-0.000230187268986486,
7.92279853500751));
#12417=CARTESIAN_POINT('',(-1.99474934551713,-0.00070464336927533,9.51915475821937));
#12418=CARTESIAN_POINT('Ctrl Pts',(-1.99474998656462,-0.000231517709445007,
7.92279862245266));
#12419=CARTESIAN_POINT('Ctrl Pts',(-1.99474919835786,-0.00702268470821122,
7.92324498174364));
#12420=CARTESIAN_POINT('Ctrl Pts',(-1.9947137291373,-0.0138139320109587,
7.92368967326531));
#12421=CARTESIAN_POINT('Ctrl Pts',(-1.99458019797554,-0.0267402687567622,
7.92453274020215));
#12422=CARTESIAN_POINT('Ctrl Pts',(-1.99448851188337,-0.0328753170553419,
7.92493143649948));
#12423=CARTESIAN_POINT('Ctrl Pts',(-1.99431154685697,-0.0419225873353665,
7.9255171731148));
#12424=CARTESIAN_POINT('Ctrl Pts',(-1.99424819438127,-0.0448351282615908,
7.92570539763462));
#12425=CARTESIAN_POINT('Ctrl Pts',(-1.99411820777729,-0.0502640251753199,
7.92605559865818));
#12426=CARTESIAN_POINT('Ctrl Pts',(-1.99405319072349,-0.0527804088123176,
7.92621766454593));
#12427=CARTESIAN_POINT('Ctrl Pts',(-1.99390931282479,-0.0579686071675126,
7.92655126521432));
#12428=CARTESIAN_POINT('Ctrl Pts',(-1.9938298451588,-0.060640381030368,
7.92672276224302));
#12429=CARTESIAN_POINT('Ctrl Pts',(-1.99363054664146,-0.0669164489115221,
7.92712492753491));
#12430=CARTESIAN_POINT('Ctrl Pts',(-1.99350631081618,-0.0705206130981336,
7.92735534875611));
#12431=CARTESIAN_POINT('Ctrl Pts',(-1.99307033130641,-0.0822450767397962,
7.92810324740931));
#12432=CARTESIAN_POINT('Ctrl Pts',(-1.99271873610237,-0.0903639440833199,
7.92861854138705));
#12433=CARTESIAN_POINT('Ctrl Pts',(-1.99112077054334,-0.122691678963774,
7.93066076785591));
#12434=CARTESIAN_POINT('Ctrl Pts',(-1.98948272109989,-0.146880213706721,
7.93216743237205));
#12435=CARTESIAN_POINT('Ctrl Pts',(-1.96990370952836,-0.374386901190947,
7.94618719422936));
#12436=CARTESIAN_POINT('Ctrl Pts',(-1.92129704506945,-0.573870850494195,
7.9574542476288));
#12437=CARTESIAN_POINT('Ctrl Pts',(-1.82542117175168,-0.805630745843469,
7.97241777499219));
#12438=CARTESIAN_POINT('Ctrl Pts',(-1.80608487406229,-0.848092158331292,
7.97523691016454));
#12439=CARTESIAN_POINT('Ctrl Pts',(-1.77684988749654,-0.906746435730694,
7.97926637794183));
#12440=CARTESIAN_POINT('Ctrl Pts',(-1.76818095249556,-0.923537061250847,
7.98043587306774));
#12441=CARTESIAN_POINT('Ctrl Pts',(-1.75256448426842,-0.9527580954185,7.98250096788063));
#12442=CARTESIAN_POINT('Ctrl Pts',(-1.74571986294223,-0.965242147521277,
7.98339295341556));
#12443=CARTESIAN_POINT('Ctrl Pts',(-1.73556681296389,-0.983299232066698,
7.98469781058864));
#12444=CARTESIAN_POINT('Ctrl Pts',(-1.73236382907274,-0.988931293951964,
7.98510690084292));
#12445=CARTESIAN_POINT('Ctrl Pts',(-1.72670129708155,-0.99877624631566,
7.98582573690936));
#12446=CARTESIAN_POINT('Ctrl Pts',(-1.72425361484388,-1.00299592748575,
7.98613505222859));
#12447=CARTESIAN_POINT('Ctrl Pts',(-1.71947348729546,-1.01116741736087,
7.98673642439877));
#12448=CARTESIAN_POINT('Ctrl Pts',(-1.71714283365613,-1.01512024297024,
7.98702841475435));
#12449=CARTESIAN_POINT('Ctrl Pts',(-1.71090263653403,-1.02562073265587,
7.98780699131351));
#12450=CARTESIAN_POINT('Ctrl Pts',(-1.70696917877913,-1.0321540287064,7.98829444805345));
#12451=CARTESIAN_POINT('Ctrl Pts',(-1.69271464262985,-1.05552582146159,
7.9900492905339));
#12452=CARTESIAN_POINT('Ctrl Pts',(-1.68218136141572,-1.07223292328785,
7.99132444840849));
#12453=CARTESIAN_POINT('Ctrl Pts',(-1.66884153951536,-1.09271107114892,
7.99291382923818));
#12454=CARTESIAN_POINT('Ctrl Pts',(-1.66626718369475,-1.09663268278067,
7.99321941368867));
#12455=CARTESIAN_POINT('Ctrl Pts',(-1.66090678184472,-1.10473592887662,
7.99385337348201));
#12456=CARTESIAN_POINT('Ctrl Pts',(-1.65811872343561,-1.10891618653504,
7.99418182144609));
#12457=CARTESIAN_POINT('Ctrl Pts',(-1.54641487542538,-1.27503549262519,
8.00729026365598));
#12458=CARTESIAN_POINT('Ctrl Pts',(-1.41435187244186,-1.42010220360328,
8.02102892779902));
#12459=CARTESIAN_POINT('Ctrl Pts',(-1.21893814355199,-1.58003710125661,
8.03852744183577));
#12460=CARTESIAN_POINT('Ctrl Pts',(-1.17292969788131,-1.6144857948274,8.04246923023262));
#12461=CARTESIAN_POINT('Ctrl Pts',(-1.11059261661262,-1.65708702467915,
8.04752320495543));
#12462=CARTESIAN_POINT('Ctrl Pts',(-1.09555200119732,-1.66706905417847,
8.04872166226926));
#12463=CARTESIAN_POINT('Ctrl Pts',(-1.07361269850618,-1.68120435789523,
8.05043747729061));
#12464=CARTESIAN_POINT('Ctrl Pts',(-1.06682156507247,-1.68552189923614,
8.05096418717117));
#12465=CARTESIAN_POINT('Ctrl Pts',(-1.05618823450231,-1.69219214897676,
8.05178181791416));
#12466=CARTESIAN_POINT('Ctrl Pts',(-1.05236396941016,-1.69457308269347,
8.05207446212659));
#12467=CARTESIAN_POINT('Ctrl Pts',(-1.04593049403554,-1.69854829581648,
8.05256435595975));
#12468=CARTESIAN_POINT('Ctrl Pts',(-1.04332564768817,-1.70014955364336,
8.0527620474876));
#12469=CARTESIAN_POINT('Ctrl Pts',(-1.03823511504251,-1.70326271392913,
8.05314708246664));
#12470=CARTESIAN_POINT('Ctrl Pts',(-1.03574978391139,-1.70477517936031,
8.05333446225131));
#12471=CARTESIAN_POINT('Ctrl Pts',(-1.0310057685985,-1.70764797882935,8.0536909700158));
#12472=CARTESIAN_POINT('Ctrl Pts',(-1.02874770181923,-1.7090092687151,8.05386015889986));
#12473=CARTESIAN_POINT('Ctrl Pts',(-1.02344977615187,-1.71218885201387,
8.05425594981016));
#12474=CARTESIAN_POINT('Ctrl Pts',(-1.02040774598619,-1.71400354190723,
8.05448231577532));
#12475=CARTESIAN_POINT('Ctrl Pts',(-1.01067197355746,-1.7197762050327,8.05520398229661));
#12476=CARTESIAN_POINT('Ctrl Pts',(-1.00395981102077,-1.72370320419505,
8.05569730724738));
#12477=CARTESIAN_POINT('Ctrl Pts',(-0.902753986074565,-1.78212267676023,
8.0630751798442));
#12478=CARTESIAN_POINT('Ctrl Pts',(-0.803953758096544,-1.82882250889825,
8.06949343634463));
#12479=CARTESIAN_POINT('Ctrl Pts',(-0.629559763123477,-1.8943707784932,
8.08033655778919));
#12480=CARTESIAN_POINT('Ctrl Pts',(-0.555788473304771,-1.91731198279,8.084785291036));
#12481=CARTESIAN_POINT('Ctrl Pts',(-0.454905773957928,-1.94237077750035,
8.09086659107214));
#12482=CARTESIAN_POINT('Ctrl Pts',(-0.428811250243471,-1.9482978100742,
8.09243907652897));
#12483=CARTESIAN_POINT('Ctrl Pts',(-0.346881013560604,-1.96518148219439,
8.09738878169408));
#12484=CARTESIAN_POINT('Ctrl Pts',(-0.290694259826521,-1.97427474120783,
8.10080208088731));
#12485=CARTESIAN_POINT('Ctrl Pts',(-0.201428744960775,-1.98482818203363,
8.10630827741049));
#12486=CARTESIAN_POINT('Ctrl Pts',(-0.168569171068974,-1.98788849989265,
8.10835258875764));
#12487=CARTESIAN_POINT('Ctrl Pts',(-0.126736832157239,-1.99073985135108,
8.11098304894076));
#12488=CARTESIAN_POINT('Ctrl Pts',(-0.117819566576094,-1.99128750458934,
8.11154537490469));
#12489=CARTESIAN_POINT('Ctrl Pts',(-0.10352060763326,-1.99206929103457,
8.11244974942427));
#12490=CARTESIAN_POINT('Ctrl Pts',(-0.0981410516170769,-1.99234156447808,
8.11279060004348));
#12491=CARTESIAN_POINT('Ctrl Pts',(-0.0879340962046485,-1.99281672561594,
8.11343849411302));
#12492=CARTESIAN_POINT('Ctrl Pts',(-0.0831069257959719,-1.99302386974665,
8.11374540174689));
#12493=CARTESIAN_POINT('Ctrl Pts',(-0.0721477659788656,-1.9934542666989,
8.11444333136067));
#12494=CARTESIAN_POINT('Ctrl Pts',(-0.066015425865769,-1.99366676646652,
8.11483468753223));
#12495=CARTESIAN_POINT('Ctrl Pts',(-0.0501893533174395,-1.99414207830848,
8.11584684511366));
#12496=CARTESIAN_POINT('Ctrl Pts',(-0.0404945990617473,-1.9943625000474,
8.11646896763902));
#12497=CARTESIAN_POINT('Ctrl Pts',(0.0192962539183146,-1.995285775576,8.12031909035055));
#12498=CARTESIAN_POINT('Ctrl Pts',(0.0693984906723488,-1.99417170078574,
8.1236035006446));
#12499=CARTESIAN_POINT('Ctrl Pts',(0.157490198662347,-1.9888892159616,8.12948643175581));
#12500=CARTESIAN_POINT('Ctrl Pts',(0.195502802759619,-1.98551299168738,
8.13206050013074));
#12501=CARTESIAN_POINT('Ctrl Pts',(0.353603103501263,-1.96688671612717,
8.14290707675554));
#12502=CARTESIAN_POINT('Ctrl Pts',(0.472267963639652,-1.94181288727138,
8.15140849277079));
#12503=CARTESIAN_POINT('Ctrl Pts',(0.666995965587714,-1.88175251228524,
8.16556739914724));
#12504=CARTESIAN_POINT('Ctrl Pts',(0.744491046033528,-1.85246115360052,
8.17125478951414));
#12505=CARTESIAN_POINT('Ctrl Pts',(0.828106081501254,-1.81475836849115,
8.17729682884523));
#12506=CARTESIAN_POINT('Ctrl Pts',(0.836237958919359,-1.81102559375437,
8.17788338092407));
#12507=CARTESIAN_POINT('Ctrl Pts',(0.848743913290462,-1.80518279142026,
8.17878348906329));
#12508=CARTESIAN_POINT('Ctrl Pts',(0.853135743192,-1.80311135142817,8.17909921553368));
#12509=CARTESIAN_POINT('Ctrl Pts',(0.860411922989664,-1.79964694990149,
8.17962162341749));
#12510=CARTESIAN_POINT('Ctrl Pts',(0.863300530292969,-1.79826305535526,
8.17982883999635));
#12511=CARTESIAN_POINT('Ctrl Pts',(0.868898882039267,-1.79556435876297,
8.18023008086414));
#12512=CARTESIAN_POINT('Ctrl Pts',(0.87160900456911,-1.79425036634199,8.18042415384803));
#12513=CARTESIAN_POINT('Ctrl Pts',(0.876673319000713,-1.79178077110302,
8.18078648815098));
#12514=CARTESIAN_POINT('Ctrl Pts',(0.879028181403468,-1.79062667698948,
8.18095483752522));
#12515=CARTESIAN_POINT('Ctrl Pts',(0.884450720555287,-1.7879558708462,8.18134219662372));
#12516=CARTESIAN_POINT('Ctrl Pts',(0.887516769138473,-1.78643590932066,
8.18156100046291));
#12517=CARTESIAN_POINT('Ctrl Pts',(0.896806920125838,-1.78180059344639,
8.18222335731854));
#12518=CARTESIAN_POINT('Ctrl Pts',(0.903018725144317,-1.77866050506421,
8.18266539126806));
#12519=CARTESIAN_POINT('Ctrl Pts',(0.949219373216593,-1.75500149881257,
8.18594765862068));
#12520=CARTESIAN_POINT('Ctrl Pts',(0.988524499290065,-1.73316696214508,
8.18870991705859));
#12521=CARTESIAN_POINT('Ctrl Pts',(1.17079741718341,-1.62369139993394,8.20153503873979));
#12522=CARTESIAN_POINT('Ctrl Pts',(1.30308454601846,-1.51957919992771,8.21094222012277));
#12523=CARTESIAN_POINT('Ctrl Pts',(1.46158788443693,-1.35873700728124,8.22429201143942));
#12524=CARTESIAN_POINT('Ctrl Pts',(1.50055068185925,-1.31558056302475,8.22777573484626));
#12525=CARTESIAN_POINT('Ctrl Pts',(1.55891495756934,-1.2449634990721,8.23338540779656));
#12526=CARTESIAN_POINT('Ctrl Pts',(1.57960303742029,-1.21860740033364,8.23546039011382));
#12527=CARTESIAN_POINT('Ctrl Pts',(1.60498204194526,-1.18454246710169,8.23812518954213));
#12528=CARTESIAN_POINT('Ctrl Pts',(1.61029857038343,-1.17730485487386,8.23869040722485));
#12529=CARTESIAN_POINT('Ctrl Pts',(1.61873149171826,-1.16566077635638,8.23959833417471));
#12530=CARTESIAN_POINT('Ctrl Pts',(1.62187923050394,-1.16127707655951,8.23993982858464));
#12531=CARTESIAN_POINT('Ctrl Pts',(1.62781016057328,-1.15294621279992,8.24058823902225));
#12532=CARTESIAN_POINT('Ctrl Pts',(1.63059688608532,-1.14900160264908,8.24089501617111));
#12533=CARTESIAN_POINT('Ctrl Pts',(1.63688136977162,-1.14003700741539,8.24159168032751));
#12534=CARTESIAN_POINT('Ctrl Pts',(1.64037039961539,-1.13501099010945,8.2419818968755));
#12535=CARTESIAN_POINT('Ctrl Pts',(1.6506119211806,-1.12011201199589,8.24313760703068));
#12536=CARTESIAN_POINT('Ctrl Pts',(1.65729870030194,-1.11019441602274,8.2439055781069));
#12537=CARTESIAN_POINT('Ctrl Pts',(1.70571082979594,-1.03697912895236,8.24956610100389));
#12538=CARTESIAN_POINT('Ctrl Pts',(1.74388153957281,-0.971416387937629,
8.25459007936603));
#12539=CARTESIAN_POINT('Ctrl Pts',(1.80497645631379,-0.851218525839171,
8.26372797321559));
#12540=CARTESIAN_POINT('Ctrl Pts',(1.82937581102105,-0.797431070722207,
8.26779211780525));
#12541=CARTESIAN_POINT('Ctrl Pts',(1.8887550277339,-0.649403382013918,8.27886396084816));
#12542=CARTESIAN_POINT('Ctrl Pts',(1.9190598748867,-0.55347067261022,8.28592632842845));
#12543=CARTESIAN_POINT('Ctrl Pts',(1.95193545864888,-0.413356824994963,
8.29581951877102));
#12544=CARTESIAN_POINT('Ctrl Pts',(1.96047756787429,-0.37073459189691,8.29877347965395));
#12545=CARTESIAN_POINT('Ctrl Pts',(1.97133790974497,-0.305558174233478,
8.30317515152615));
#12546=CARTESIAN_POINT('Ctrl Pts',(1.9746754281152,-0.283189007121508,8.3046653631025));
#12547=CARTESIAN_POINT('Ctrl Pts',(1.97833151175884,-0.255461594712451,
8.30648332639868));
#12548=CARTESIAN_POINT('Ctrl Pts',(1.97900970236519,-0.250153545529075,
8.30683003181563));
#12549=CARTESIAN_POINT('Ctrl Pts',(1.9800447757931,-0.241784499837728,8.30737452503285));
#12550=CARTESIAN_POINT('Ctrl Pts',(1.98041593330107,-0.238725344173639,
8.30757310324985));
#12551=CARTESIAN_POINT('Ctrl Pts',(1.9810987587589,-0.232986158452578,8.30794478724546));
#12552=CARTESIAN_POINT('Ctrl Pts',(1.98141207480238,-0.230306387072146,
8.30811798165558));
#12553=CARTESIAN_POINT('Ctrl Pts',(1.98211423392382,-0.224193363413962,
8.30851226908235));
#12554=CARTESIAN_POINT('Ctrl Pts',(1.98249959365815,-0.220759738421593,
8.3087331636315));
#12555=CARTESIAN_POINT('Ctrl Pts',(1.98365243526449,-0.210241201841807,
8.30940814395487));
#12556=CARTESIAN_POINT('Ctrl Pts',(1.98439088432201,-0.203153067406235,
8.30986062437608));
#12557=CARTESIAN_POINT('Ctrl Pts',(1.98994114960749,-0.146957375157954,
8.31343027016316));
#12558=CARTESIAN_POINT('Ctrl Pts',(1.99296780040644,-0.0976858818530874,
8.31645327444844));
#12559=CARTESIAN_POINT('Ctrl Pts',(1.99451998299925,-0.0336649519246329,
8.3203011941513));
#12560=CARTESIAN_POINT('Ctrl Pts',(1.9947138020683,-0.0189777777130987,
8.32117848838709));
#12561=CARTESIAN_POINT('Ctrl Pts',(1.99486315799158,0.0504767434801115,
8.32530672653474));
#12562=CARTESIAN_POINT('Ctrl Pts',(1.9927254450652,0.105226956036382,8.32850142798983));
#12563=CARTESIAN_POINT('Ctrl Pts',(1.98018545881007,0.261236509058774,8.33759394038254));
#12564=CARTESIAN_POINT('Ctrl Pts',(1.96428684639156,0.361877236430052,8.34345376848755));
#12565=CARTESIAN_POINT('Ctrl Pts',(1.92864216957015,0.511984217938865,8.35261311640273));
#12566=CARTESIAN_POINT('Ctrl Pts',(1.91448811627231,0.562603826910618,8.35577507977248));
#12567=CARTESIAN_POINT('Ctrl Pts',(1.88878231313883,0.642261770431691,8.36091023176004));
#12568=CARTESIAN_POINT('Ctrl Pts',(1.87851806472765,0.671690792713433,8.36284281731794));
#12569=CARTESIAN_POINT('Ctrl Pts',(1.86449153788505,0.709066702808122,8.36534792026673));
#12570=CARTESIAN_POINT('Ctrl Pts',(1.86136004999609,0.717246850263437,8.3658993342113));
#12571=CARTESIAN_POINT('Ctrl Pts',(1.85623016925888,0.730387374603764,8.36679030446632));
#12572=CARTESIAN_POINT('Ctrl Pts',(1.85426550304053,0.735360864863523,8.36712872581784));
#12573=CARTESIAN_POINT('Ctrl Pts',(1.85048463770983,0.744820509920601,8.36777472869912));
#12574=CARTESIAN_POINT('Ctrl Pts',(1.84867206084681,0.749308078939836,8.36808218612897));
#12575=CARTESIAN_POINT('Ctrl Pts',(1.84449796102807,0.759534956826287,8.36878516797642));
#12576=CARTESIAN_POINT('Ctrl Pts',(1.8421259579232,0.765269908322834,8.36918104506223));
#12577=CARTESIAN_POINT('Ctrl Pts',(1.83477734615351,0.782804996250314,8.37039663610397));
#12578=CARTESIAN_POINT('Ctrl Pts',(1.82971390730288,0.79456817002563,8.37121929320982));
#12579=CARTESIAN_POINT('Ctrl Pts',(1.78312360124049,0.899997554589512,8.37865871515974));
#12580=CARTESIAN_POINT('Ctrl Pts',(1.73455774807666,0.990367994491398,8.38552067686724));
#12581=CARTESIAN_POINT('Ctrl Pts',(1.60645029012431,1.19018971634929,8.40182385625274));
#12582=CARTESIAN_POINT('Ctrl Pts',(1.52229322252373,1.29609212985326,8.41136305929429));
#12583=CARTESIAN_POINT('Ctrl Pts',(1.39927749418973,1.42223542577928,8.42345559862231));
#12584=CARTESIAN_POINT('Ctrl Pts',(1.36954868653589,1.45088523872937,8.42625671105926));
#12585=CARTESIAN_POINT('Ctrl Pts',(1.32277093468428,1.4932451421116,8.43045705871768));
#12586=CARTESIAN_POINT('Ctrl Pts',(1.30635126125194,1.50763075048331,8.4318945924608));
#12587=CARTESIAN_POINT('Ctrl Pts',(1.28566244582949,1.52516478469197,8.43365719966969));
#12588=CARTESIAN_POINT('Ctrl Pts',(1.28161330237793,1.5285689025361,8.43399990147263));
#12589=CARTESIAN_POINT('Ctrl Pts',(1.27519441749139,1.53392182740926,8.43453952770088));
#12590=CARTESIAN_POINT('Ctrl Pts',(1.27283367601301,1.53588131329318,8.43473721941486));
#12591=CARTESIAN_POINT('Ctrl Pts',(1.26838664679261,1.53955518518983,8.43510815487782));
#12592=CARTESIAN_POINT('Ctrl Pts',(1.26630142340231,1.54127076115827,8.43528148317324));
#12593=CARTESIAN_POINT('Ctrl Pts',(1.26152339202232,1.54518554912742,8.43567727277348));
#12594=CARTESIAN_POINT('Ctrl Pts',(1.25882831884873,1.54738195477544,8.43589952983252));
#12595=CARTESIAN_POINT('Ctrl Pts',(1.25050661791335,1.55412776709656,8.43658280770704));
#12596=CARTESIAN_POINT('Ctrl Pts',(1.24486088992064,1.55865367754036,8.4370421651381));
#12597=CARTESIAN_POINT('Ctrl Pts',(1.19807788950323,1.59574102996418,8.44081526606513));
#12598=CARTESIAN_POINT('Ctrl Pts',(1.15569117061557,1.62670190499935,8.44402244164942));
#12599=CARTESIAN_POINT('Ctrl Pts',(1.05512066905209,1.69424428359257,8.45128273539682));
#12600=CARTESIAN_POINT('Ctrl Pts',(0.996170117816534,1.72956338474557,8.4552871836776));
#12601=CARTESIAN_POINT('Ctrl Pts',(0.846411451135171,1.80908614897429,8.46513389694844));
#12602=CARTESIAN_POINT('Ctrl Pts',(0.753851595048748,1.84957068237211,8.47094876518043));
#12603=CARTESIAN_POINT('Ctrl Pts',(0.610060098383983,1.89986895498957,8.48000046845443));
#12604=CARTESIAN_POINT('Ctrl Pts',(0.560853055406495,1.91497222164778,8.48309942273978));
#12605=CARTESIAN_POINT('Ctrl Pts',(0.481448291601828,1.93602101458039,8.48814111088676));
#12606=CARTESIAN_POINT('Ctrl Pts',(0.451600521548301,1.9432001016132,8.49004511829261));
#12607=CARTESIAN_POINT('Ctrl Pts',(0.413084316541226,1.95152884204975,8.49251808416927));
#12608=CARTESIAN_POINT('Ctrl Pts',(0.40455656351681,1.95331447979062,8.49306660735261));
#12609=CARTESIAN_POINT('Ctrl Pts',(0.3907865517942,1.95610375975275,8.493954027109));
#12610=CARTESIAN_POINT('Ctrl Pts',(0.385551420483809,1.95714234261121,8.49429180517637));
#12611=CARTESIAN_POINT('Ctrl Pts',(0.375558802752016,1.95908310071585,8.4949373234207));
#12612=CARTESIAN_POINT('Ctrl Pts',(0.370802069172672,1.9599889884009,8.4952449426467));
#12613=CARTESIAN_POINT('Ctrl Pts',(0.359922145165043,1.96201997215704,8.49594934072553));
#12614=CARTESIAN_POINT('Ctrl Pts',(0.353796915157029,1.96313373540777,8.49634647740351));
#12615=CARTESIAN_POINT('Ctrl Pts',(0.334958041792395,1.96646821504985,8.49756972961547));
#12616=CARTESIAN_POINT('Ctrl Pts',(0.322228179310622,1.96859419840775,8.49839884256805));
#12617=CARTESIAN_POINT('Ctrl Pts',(0.17002543558183,1.99249738076289,8.50834383411671));
#12618=CARTESIAN_POINT('Ctrl Pts',(0.0286703205075798,1.99952930955107,
8.51794241227215));
#12619=CARTESIAN_POINT('Ctrl Pts',(-0.210506504120044,1.98605295207319,
8.53460073779848));
#12620=CARTESIAN_POINT('Ctrl Pts',(-0.308253603338334,1.97324599557256,
8.54151624800528));
#12621=CARTESIAN_POINT('Ctrl Pts',(-0.461585935940137,1.94148036013177,
8.5522492392706));
#12622=CARTESIAN_POINT('Ctrl Pts',(-0.517978582685788,1.92720191624104,
8.55616880575215));
#12623=CARTESIAN_POINT('Ctrl Pts',(-0.580203651643638,1.90851717021064,
8.56040474559539));
#12624=CARTESIAN_POINT('Ctrl Pts',(-0.586724945791023,1.90652246449761,
8.56084756144487));
#12625=CARTESIAN_POINT('Ctrl Pts',(-0.596476185128885,1.90348502504609,
8.56150788968686));
#12626=CARTESIAN_POINT('Ctrl Pts',(-0.599713822617182,1.90246745343574,
8.56172683405279));
#12627=CARTESIAN_POINT('Ctrl Pts',(-0.605271364915361,1.90070515168517,
8.56210212663698));
#12628=CARTESIAN_POINT('Ctrl Pts',(-0.607592510685936,1.8999644312538,8.56225870893541));
#12629=CARTESIAN_POINT('Ctrl Pts',(-0.612431897141488,1.89841031833551,
8.56258482913751));
#12630=CARTESIAN_POINT('Ctrl Pts',(-0.614949867764217,1.89759617035238,
8.56275432120036));
#12631=CARTESIAN_POINT('Ctrl Pts',(-0.621947430236766,1.89531822281732,
8.56322483628384));
#12632=CARTESIAN_POINT('Ctrl Pts',(-0.62642350324943,1.8938435435362,8.56352522298788));
#12633=CARTESIAN_POINT('Ctrl Pts',(-0.644327565861596,1.88787448163442,
8.56472457188317));
#12634=CARTESIAN_POINT('Ctrl Pts',(-0.657713158802765,1.88325290351226,
8.56561631395642));
#12635=CARTESIAN_POINT('Ctrl Pts',(-0.78716585736158,1.83700877640986,8.57420279605515));
#12636=CARTESIAN_POINT('Ctrl Pts',(-0.899204661235883,1.78484488547056,
8.58134932864037));
#12637=CARTESIAN_POINT('Ctrl Pts',(-1.07576225874995,1.68176725401699,8.59320782759595));
#12638=CARTESIAN_POINT('Ctrl Pts',(-1.14324302575928,1.63664296192731,8.59790231384253));
#12639=CARTESIAN_POINT('Ctrl Pts',(-1.25290082780132,1.5532161200711,8.60605640141695));
#12640=CARTESIAN_POINT('Ctrl Pts',(-1.29652772255488,1.51698908462148,8.60945757932838));
#12641=CARTESIAN_POINT('Ctrl Pts',(-1.36295167933405,1.45687110856619,8.61494594452384));
#12642=CARTESIAN_POINT('Ctrl Pts',(-1.38680132096748,1.434187089192,8.61698494925403));
#12643=CARTESIAN_POINT('Ctrl Pts',(-1.41639142011538,1.4046147446235,8.61960946504547));
#12644=CARTESIAN_POINT('Ctrl Pts',(-1.42266243464717,1.3982627895587,8.62017128627684));
#12645=CARTESIAN_POINT('Ctrl Pts',(-1.43264775950447,1.38801187108157,8.62107504074794));
#12646=CARTESIAN_POINT('Ctrl Pts',(-1.43638932989371,1.38413953383203,8.62141577899471));
#12647=CARTESIAN_POINT('Ctrl Pts',(-1.44345859753185,1.37676366444645,8.62206358356379));
#12648=CARTESIAN_POINT('Ctrl Pts',(-1.44678933840303,1.37326309210471,8.62237051460594));
#12649=CARTESIAN_POINT('Ctrl Pts',(-1.4543229337111,1.36528753614966,8.62306866814696));
#12650=CARTESIAN_POINT('Ctrl Pts',(-1.45851789878658,1.36080519892093,8.62346022565939));
#12651=CARTESIAN_POINT('Ctrl Pts',(-1.46929254426302,1.3491853902312,8.62447324254151));
#12652=CARTESIAN_POINT('Ctrl Pts',(-1.47584087316181,1.34201919114791,8.62509602677348));
#12653=CARTESIAN_POINT('Ctrl Pts',(-1.51597328106713,1.29745110171667,8.62895756103816));
#12654=CARTESIAN_POINT('Ctrl Pts',(-1.54818324441548,1.25884162454708,8.63225310633331));
#12655=CARTESIAN_POINT('Ctrl Pts',(-1.58164999819233,1.21549624204324,8.63590407090433));
#12656=CARTESIAN_POINT('Ctrl Pts',(-1.58438928193606,1.21192344394325,8.63620465163962));
#12657=CARTESIAN_POINT('Ctrl Pts',(-1.7025774672363,1.05668717812211,8.64924935851054));
#12658=CARTESIAN_POINT('Ctrl Pts',(-1.79569805930562,0.889271865546751,
8.66282020358993));
#12659=CARTESIAN_POINT('Ctrl Pts',(-1.88362460343772,0.658883452183352,
8.67970186574406));
#12660=CARTESIAN_POINT('Ctrl Pts',(-1.90139572804824,0.605693548269844,
8.68347600624639));
#12661=CARTESIAN_POINT('Ctrl Pts',(-1.9187777646919,0.5453121310817,8.68757229660485));
#12662=CARTESIAN_POINT('Ctrl Pts',(-1.92061818691374,0.538794222212334,
8.68801204673621));
#12663=CARTESIAN_POINT('Ctrl Pts',(-1.92332844537685,0.529005394061882,
8.68866871405302));
#12664=CARTESIAN_POINT('Ctrl Pts',(-1.92422318826357,0.525741512444485,
8.68888704017161));
#12665=CARTESIAN_POINT('Ctrl Pts',(-1.92574748824871,0.520125085498782,
8.68926163709257));
#12666=CARTESIAN_POINT('Ctrl Pts',(-1.92638104583876,0.517773656662664,
8.68941813947184));
#12667=CARTESIAN_POINT('Ctrl Pts',(-1.92769521524748,0.512860356998419,
8.68974445796068));
#12668=CARTESIAN_POINT('Ctrl Pts',(-1.92837502451171,0.510298298752017,
8.68991422698065));
#12669=CARTESIAN_POINT('Ctrl Pts',(-1.93025483735156,0.503156279105541,
8.69038640768047));
#12670=CARTESIAN_POINT('Ctrl Pts',(-1.93144365521974,0.498573350816465,
8.69068817547325));
#12671=CARTESIAN_POINT('Ctrl Pts',(-1.93616370910622,0.480107140939406,
8.69189934263267));
#12672=CARTESIAN_POINT('Ctrl Pts',(-1.93956177019794,0.466189814427429,
8.69280134190122));
#12673=CARTESIAN_POINT('Ctrl Pts',(-1.97718139401264,0.304575808395203,
8.70316365221341));
#12674=CARTESIAN_POINT('Ctrl Pts',(-1.99461257593291,0.153453720322189,
8.71179798766024));
#12675=CARTESIAN_POINT('Ctrl Pts',(-1.9948712195267,-0.133668063256788,
8.72848308371536));
#12676=CARTESIAN_POINT('Ctrl Pts',(-1.98119470638394,-0.268771511709406,
8.73645960938413));
#12677=CARTESIAN_POINT('Ctrl Pts',(-1.95133019285738,-0.414132864749555,
8.74572228903352));
#12678=CARTESIAN_POINT('Ctrl Pts',(-1.94859819806634,-0.426802766026727,
8.74653511835288));
#12679=CARTESIAN_POINT('Ctrl Pts',(-1.94436908514981,-0.445528131973983,
8.7477449112978));
#12680=CARTESIAN_POINT('Ctrl Pts',(-1.94296668538109,-0.451604820314016,
8.74813883678131));
#12681=CARTESIAN_POINT('Ctrl Pts',(-1.94042451116146,-0.462389164508565,
8.74884034143957));
#12682=CARTESIAN_POINT('Ctrl Pts',(-1.93929603772199,-0.467099454472853,
8.74914755486349));
#12683=CARTESIAN_POINT('Ctrl Pts',(-1.93688937959648,-0.476985869411982,
8.74979410163906));
#12684=CARTESIAN_POINT('Ctrl Pts',(-1.93560757738012,-0.482161066336755,
8.75013354953625));
#12685=CARTESIAN_POINT('Ctrl Pts',(-1.93218260533877,-0.495755400451982,
8.75102789131757));
#12686=CARTESIAN_POINT('Ctrl Pts',(-1.93000517328316,-0.504165711438824,
8.75158388846695));
#12687=CARTESIAN_POINT('Ctrl Pts',(-1.91994969820836,-0.541984929848783,
8.75409647391396));
#12688=CARTESIAN_POINT('Ctrl Pts',(-1.91145427515081,-0.571224029081828,
8.75607296827559));
#12689=CARTESIAN_POINT('Ctrl Pts',(-1.88698279356925,-0.648777507387629,
8.76140996467395));
#12690=CARTESIAN_POINT('Ctrl Pts',(-1.86982252687338,-0.696691679811968,
8.76480734494315));
#12691=CARTESIAN_POINT('Ctrl Pts',(-1.81338344907362,-0.837115270440164,
8.77506133297987));
#12692=CARTESIAN_POINT('Ctrl Pts',(-1.76892982573233,-0.927364797288488,
8.78205501589821));
#12693=CARTESIAN_POINT('Ctrl Pts',(-1.655881647942,-1.11890972469254,8.79757326434299));
#12694=CARTESIAN_POINT('Ctrl Pts',(-1.58437979116762,-1.21805214954246,
8.80607587102078));
#12695=CARTESIAN_POINT('Ctrl Pts',(-1.49928347115201,-1.3157636743316,8.81453558878648));
#12696=CARTESIAN_POINT('Ctrl Pts',(-1.49427466625688,-1.32144928007537,
8.81502809347339));
#12697=CARTESIAN_POINT('Ctrl Pts',(-1.48690171831705,-1.32972295103032,
8.81574497790965));
#12698=CARTESIAN_POINT('Ctrl Pts',(-1.4845630329989,-1.33233345974091,8.81597119772909));
#12699=CARTESIAN_POINT('Ctrl Pts',(-1.48040331329187,-1.33695210871287,
8.81637146659798));
#12700=CARTESIAN_POINT('Ctrl Pts',(-1.47858505316461,-1.33896271490548,
8.81654572205943));
#12701=CARTESIAN_POINT('Ctrl Pts',(-1.47473391977586,-1.3432038325526,8.81691330412691));
#12702=CARTESIAN_POINT('Ctrl Pts',(-1.47270008733336,-1.34543343313088,
8.81710655555436));
#12703=CARTESIAN_POINT('Ctrl Pts',(-1.4672394448791,-1.35139247642033,8.81762311138456));
#12704=CARTESIAN_POINT('Ctrl Pts',(-1.46380344945119,-1.35511352906802,
8.81794572494267));
#12705=CARTESIAN_POINT('Ctrl Pts',(-1.44729277991712,-1.37285788345148,
8.81948465836798));
#12706=CARTESIAN_POINT('Ctrl Pts',(-1.43403000936744,-1.3867058653566,8.82068718836113));
#12707=CARTESIAN_POINT('Ctrl Pts',(-1.39649112352568,-1.42478645771653,
8.82400573882597));
#12708=CARTESIAN_POINT('Ctrl Pts',(-1.37178574784152,-1.44858829811479,
8.82609361627723));
#12709=CARTESIAN_POINT('Ctrl Pts',(-1.27943561048134,-1.53307819133598,
8.83361080412467));
#12710=CARTESIAN_POINT('Ctrl Pts',(-1.20827651075083,-1.58976549836233,
8.83886715203368));
#12711=CARTESIAN_POINT('Ctrl Pts',(-1.00427656197088,-1.73064050114208,
8.85324523900114));
#12712=CARTESIAN_POINT('Ctrl Pts',(-0.864994015592043,-1.80429043552511,
8.86238813070886));
#12713=CARTESIAN_POINT('Ctrl Pts',(-0.706829196491486,-1.86536250943538,
8.87297601545846));
#12714=CARTESIAN_POINT('Ctrl Pts',(-0.695089226714996,-1.86976890552744,
8.87376268101761));
#12715=CARTESIAN_POINT('Ctrl Pts',(-0.677527657379335,-1.87617208685013,
8.87494088959773));
#12716=CARTESIAN_POINT('Ctrl Pts',(-0.671736943825578,-1.87825315197675,
8.87532962284469));
#12717=CARTESIAN_POINT('Ctrl Pts',(-0.661380480805454,-1.88192103595676,
8.87602531193258));
#12718=CARTESIAN_POINT('Ctrl Pts',(-0.656818398393524,-1.88351812224486,
8.876331923984));
#12719=CARTESIAN_POINT('Ctrl Pts',(-0.647169572322146,-1.88685664919923,
8.87698076170768));
#12720=CARTESIAN_POINT('Ctrl Pts',(-0.642081510127311,-1.88859413410776,
8.87732311553629));
#12721=CARTESIAN_POINT('Ctrl Pts',(-0.628562330140101,-1.89314975243665,
8.87823334129869));
#12722=CARTESIAN_POINT('Ctrl Pts',(-0.620119367098661,-1.89593210699305,
8.87880238854272));
#12723=CARTESIAN_POINT('Ctrl Pts',(-0.580702202905509,-1.90863046183729,
8.88146206344512));
#12724=CARTESIAN_POINT('Ctrl Pts',(-0.549508575655639,-1.9178439472601,
8.88357556558254));
#12725=CARTESIAN_POINT('Ctrl Pts',(-0.464265935569141,-1.94077125358747,
8.88937853642262));
#12726=CARTESIAN_POINT('Ctrl Pts',(-0.409847888416812,-1.95298737070563,
8.89311330066537));
#12727=CARTESIAN_POINT('Ctrl Pts',(-0.252367966201468,-1.98146775926962,
8.9039984746494));
#12728=CARTESIAN_POINT('Ctrl Pts',(-0.148451749659453,-1.99194952987044,
8.9112833732864));
#12729=CARTESIAN_POINT('Ctrl Pts',(0.0322676069675566,-1.99595513025144,
8.9238876027556));
#12730=CARTESIAN_POINT('Ctrl Pts',(0.108777153001586,-1.9932504154117,8.92919992888788));
#12731=CARTESIAN_POINT('Ctrl Pts',(0.220691514846194,-1.98282918575057,
8.93678782057855));
#12732=CARTESIAN_POINT('Ctrl Pts',(0.256342683274169,-1.97853611292099,
8.93917699825019));
#12733=CARTESIAN_POINT('Ctrl Pts',(0.297687922397998,-1.97242088751557,
8.94190050405145));
#12734=CARTESIAN_POINT('Ctrl Pts',(0.303510950166099,-1.97153325153051,
8.94228298133976));
#12735=CARTESIAN_POINT('Ctrl Pts',(0.312811277746774,-1.9700733703544,8.94289201048762));
#12736=CARTESIAN_POINT('Ctrl Pts',(0.316291085565656,-1.9695176896198,8.94311947017718));
#12737=CARTESIAN_POINT('Ctrl Pts',(0.322447807500711,-1.96851780200896,
8.94352115199808));
#12738=CARTESIAN_POINT('Ctrl Pts',(0.325125307925283,-1.96807735109432,
8.94369558562817));
#12739=CARTESIAN_POINT('Ctrl Pts',(0.33076873336208,-1.96713717204483,8.94406270022442));
#12740=CARTESIAN_POINT('Ctrl Pts',(0.33373442177827,-1.96663620037476,8.94425530925021));
#12741=CARTESIAN_POINT('Ctrl Pts',(0.341646133624258,-1.96528132180977,
8.94476833043426));
#12742=CARTESIAN_POINT('Ctrl Pts',(0.346590126967151,-1.9644154447779,8.94508806817207));
#12743=CARTESIAN_POINT('Ctrl Pts',(0.36991525599551,-1.96023954780605,8.94659277420059));
#12744=CARTESIAN_POINT('Ctrl Pts',(0.388253323196731,-1.95669001108131,
8.94776468420938));
#12745=CARTESIAN_POINT('Ctrl Pts',(0.574893587595598,-1.91783635127253,
8.95960375346688));
#12746=CARTESIAN_POINT('Ctrl Pts',(0.73803417500281,-1.8611617396097,8.96926487394913));
#12747=CARTESIAN_POINT('Ctrl Pts',(0.990543753951332,-1.73493888711216,
8.98577814694247));
#12748=CARTESIAN_POINT('Ctrl Pts',(1.08491556362824,-1.67754073427017,8.99235467400632));
#12749=CARTESIAN_POINT('Ctrl Pts',(1.18449948715099,-1.60504064125372,9.00004366418073));
#12750=CARTESIAN_POINT('Ctrl Pts',(1.19487045727827,-1.59733499083669,9.0008539606765));
#12751=CARTESIAN_POINT('Ctrl Pts',(1.21012883357632,-1.58576623823173,9.00206069960659));
#12752=CARTESIAN_POINT('Ctrl Pts',(1.21507432048008,-1.58198000949722,9.00245412638088));
#12753=CARTESIAN_POINT('Ctrl Pts',(1.22383322436455,-1.57520895507257,9.00315506948077));
#12754=CARTESIAN_POINT('Ctrl Pts',(1.2276536741217,-1.57223327433851,9.00346222216824));
#12755=CARTESIAN_POINT('Ctrl Pts',(1.23566077676945,-1.56594970459861,9.00410897452413));
#12756=CARTESIAN_POINT('Ctrl Pts',(1.2398450628347,-1.56263887441444,9.00444869000707));
#12757=CARTESIAN_POINT('Ctrl Pts',(1.25082171125663,-1.55388172254456,9.00534449447386));
#12758=CARTESIAN_POINT('Ctrl Pts',(1.2575917298175,-1.54840769764214,9.00590169328192));
#12759=CARTESIAN_POINT('Ctrl Pts',(1.28801826757867,-1.52347457808038,9.00842746164429));
#12760=CARTESIAN_POINT('Ctrl Pts',(1.31125940703234,-1.50351735659395,9.01041619430015));
#12761=CARTESIAN_POINT('Ctrl Pts',(1.37217632382544,-1.44872086972475,9.01579427062109));
#12762=CARTESIAN_POINT('Ctrl Pts',(1.40898076916794,-1.4129516827679,9.01922119512866));
#12763=CARTESIAN_POINT('Ctrl Pts',(1.51389345210909,-1.30281115691842,9.0295309384371));
#12764=CARTESIAN_POINT('Ctrl Pts',(1.57778463103721,-1.22465613256173,9.03655068356465));
#12765=CARTESIAN_POINT('Ctrl Pts',(1.6841844803214,-1.07227998251384,9.04951722788825));
#12766=CARTESIAN_POINT('Ctrl Pts',(1.72837192207188,-0.999496918901939,
9.05544466567372));
#12767=CARTESIAN_POINT('Ctrl Pts',(1.78509575959843,-0.890986942673127,
9.06372090870368));
#12768=CARTESIAN_POINT('Ctrl Pts',(1.80147845757624,-0.857379970392465,
9.06621085083126));
#12769=CARTESIAN_POINT('Ctrl Pts',(1.81936916166936,-0.817899117130282,
9.06903581628544));
#12770=CARTESIAN_POINT('Ctrl Pts',(1.8218057928042,-0.812457240554516,9.06942302624669));
#12771=CARTESIAN_POINT('Ctrl Pts',(1.82565220465214,-0.803762500479012,
9.07003813861911));
#12772=CARTESIAN_POINT('Ctrl Pts',(1.82707775378387,-0.800516715398479,
9.07026697715849));
#12773=CARTESIAN_POINT('Ctrl Pts',(1.829580404173,-0.794777004369244,9.07067023727668));
#12774=CARTESIAN_POINT('Ctrl Pts',(1.83066107256199,-0.792284658297716,
9.07084487601038));
#12775=CARTESIAN_POINT('Ctrl Pts',(1.83292318661552,-0.787038204325411,
9.07121150347618));
#12776=CARTESIAN_POINT('Ctrl Pts',(1.83410351565088,-0.784283645926796,
9.07140342378063));
#12777=CARTESIAN_POINT('Ctrl Pts',(1.83722497722179,-0.776953441193756,
9.07191265672301));
#12778=CARTESIAN_POINT('Ctrl Pts',(1.83915523892175,-0.772373145013534,
9.07222931236446));
#12779=CARTESIAN_POINT('Ctrl Pts',(1.84805788817394,-0.75102553755355,9.07369822586326));
#12780=CARTESIAN_POINT('Ctrl Pts',(1.85481850208658,-0.734170073418918,
9.07483816773641));
#12781=CARTESIAN_POINT('Ctrl Pts',(1.91739535033485,-0.571769873827472,
9.08565359998278));
#12782=CARTESIAN_POINT('Ctrl Pts',(1.95620832368073,-0.420225514296504,
9.09449394386143));
#12783=CARTESIAN_POINT('Ctrl Pts',(1.99386873050268,-0.139996348203782,
9.11095368171462));
#12784=CARTESIAN_POINT('Ctrl Pts',(1.99873350416568,-0.0129990598037182,
9.11845430159421));
#12785=CARTESIAN_POINT('Ctrl Pts',(1.99077256562081,0.126575313573216,9.12717997152477));
#12786=CARTESIAN_POINT('Ctrl Pts',(1.98990498202591,0.139552383661874,9.12799558985713));
#12787=CARTESIAN_POINT('Ctrl Pts',(1.98843306153819,0.158746732133081,9.12920874484194));
#12788=CARTESIAN_POINT('Ctrl Pts',(1.98792631274059,0.16497132736871,9.12960321850335));
#12789=CARTESIAN_POINT('Ctrl Pts',(1.98697456266756,0.176020229321791,9.1303053411172));
#12790=CARTESIAN_POINT('Ctrl Pts',(1.98654119889403,0.180845509307262,9.13061262199557));
#12791=CARTESIAN_POINT('Ctrl Pts',(1.98559442483017,0.190973088244688,9.13125894617887));
#12792=CARTESIAN_POINT('Ctrl Pts',(1.98507734474336,0.196274997973149,9.13159810264342));
#12793=CARTESIAN_POINT('Ctrl Pts',(1.9836631766378,0.210197734220782,9.13249085130298));
#12794=CARTESIAN_POINT('Ctrl Pts',(1.98273113542377,0.218814822415026,9.13304553963666));
#12795=CARTESIAN_POINT('Ctrl Pts',(1.97829470653264,0.25747303655343,9.13554384709906));
#12796=CARTESIAN_POINT('Ctrl Pts',(1.97416367201117,0.287436844290733,9.13750709589638));
#12797=CARTESIAN_POINT('Ctrl Pts',(1.96133343722684,0.367070485823468,9.14279974935694));
#12798=CARTESIAN_POINT('Ctrl Pts',(1.95142995828625,0.416521297994372,9.14616528229606));
#12799=CARTESIAN_POINT('Ctrl Pts',(1.9163036686025,0.56287421998384,9.15635900505328));
#12800=CARTESIAN_POINT('Ctrl Pts',(1.8856512087182,0.658303379924851,9.16332441021045));
#12801=CARTESIAN_POINT('Ctrl Pts',(1.8016335613901,0.865038322893551,9.17889434919384));
#12802=CARTESIAN_POINT('Ctrl Pts',(1.74483771688556,0.974537625131619,9.1874785853881));
#12803=CARTESIAN_POINT('Ctrl Pts',(1.67422003688979,1.08446848562963,9.19600888768589));
#12804=CARTESIAN_POINT('Ctrl Pts',(1.67010103560599,1.09080115673942,9.19649989473049));
#12805=CARTESIAN_POINT('Ctrl Pts',(1.66402078775315,1.10003392410547,9.19721501329284));
#12806=CARTESIAN_POINT('Ctrl Pts',(1.66208778584233,1.10295240553285,9.19744095222803));
#12807=CARTESIAN_POINT('Ctrl Pts',(1.65864457729324,1.10812141664551,9.19784090185988));
#12808=CARTESIAN_POINT('Ctrl Pts',(1.65713745643808,1.1103739724224,9.19801511781593));
#12809=CARTESIAN_POINT('Ctrl Pts',(1.65394112508214,1.11513023405453,9.19838280980742));
#12810=CARTESIAN_POINT('Ctrl Pts',(1.65225082263892,1.1176331703769,9.19857620991978));
#12811=CARTESIAN_POINT('Ctrl Pts',(1.6477048579684,1.12433181131501,9.19909358407897));
#12812=CARTESIAN_POINT('Ctrl Pts',(1.64483883290656,1.1285205075816,9.19941686345561));
#12813=CARTESIAN_POINT('Ctrl Pts',(1.63100345231419,1.14857624347236,9.20096383887248));
#12814=CARTESIAN_POINT('Ctrl Pts',(1.6198198580537,1.16429521298118,9.20217357005242));
#12815=CARTESIAN_POINT('Ctrl Pts',(1.58794877964815,1.20774288668222,9.20551714559542));
#12816=CARTESIAN_POINT('Ctrl Pts',(1.56676467253656,1.23510038531111,9.20762232956163));
#12817=CARTESIAN_POINT('Ctrl Pts',(1.48681524806204,1.33297871826151,9.21520971605896));
#12818=CARTESIAN_POINT('Ctrl Pts',(1.42391110370231,1.39997546068546,9.22051632014442));
#12819=CARTESIAN_POINT('Ctrl Pts',(1.24253094788149,1.56823430375081,9.23486528437918));
#12820=CARTESIAN_POINT('Ctrl Pts',(1.11647736803299,1.66033460837213,9.24393197198401));
#12821=CARTESIAN_POINT('Ctrl Pts',(0.970053344998273,1.74303829056393,9.25443311532393));
#12822=CARTESIAN_POINT('Ctrl Pts',(0.959036299165654,1.74912416363821,9.25522267219396));
#12823=CARTESIAN_POINT('Ctrl Pts',(0.942540368423959,1.75803390008944,9.25640437510974));
#12824=CARTESIAN_POINT('Ctrl Pts',(0.937104648719312,1.76093736854443,9.25679368656554));
#12825=CARTESIAN_POINT('Ctrl Pts',(0.927493503402662,1.76601402031382,9.25748194073597));
#12826=CARTESIAN_POINT('Ctrl Pts',(0.923323656768331,1.76819771039007,9.25778050870269));
#12827=CARTESIAN_POINT('Ctrl Pts',(0.914513441564125,1.77277183382422,9.25841128068376));
#12828=CARTESIAN_POINT('Ctrl Pts',(0.909871347485943,1.77515884916593,9.25874360236748));
#12829=CARTESIAN_POINT('Ctrl Pts',(0.900363143603138,1.78000097711915,9.25942424183463));
#12830=CARTESIAN_POINT('Ctrl Pts',(0.895496237024818,1.7824544194457,9.2597726148598));
#12831=CARTESIAN_POINT('Ctrl Pts',(0.883476063557577,1.78845221886334,9.26063299412145));
#12832=CARTESIAN_POINT('Ctrl Pts',(0.876311505848276,1.79197361466987,9.26114579746332));
#12833=CARTESIAN_POINT('Ctrl Pts',(0.856414242517697,1.80160530181083,9.26256997678239));
#12834=CARTESIAN_POINT('Ctrl Pts',(0.843637685815049,1.80762342768383,9.26348451933301));
#12835=CARTESIAN_POINT('Ctrl Pts',(0.727697535552327,1.86073764447368,9.27178508870476));
#12836=CARTESIAN_POINT('Ctrl Pts',(0.620774059034965,1.89908402303756,9.27946973697872));
#12837=CARTESIAN_POINT('Ctrl Pts',(0.378259191255245,1.9633797100866,9.2968442164919));
#12838=CARTESIAN_POINT('Ctrl Pts',(0.242041533444697,1.98478138891175,9.30657394376062));
#12839=CARTESIAN_POINT('Ctrl Pts',(0.0689674952153302,1.99387855063382,
9.31827295996429));
#12840=CARTESIAN_POINT('Ctrl Pts',(0.0331840629342068,1.99479507753941,
9.3206544067323));
#12841=CARTESIAN_POINT('Ctrl Pts',(-0.00849179740224064,1.99474060462243,
9.32337011611159));
#12842=CARTESIAN_POINT('Ctrl Pts',(-0.0143763629121435,1.99470687386591,
9.32375222428513));
#12843=CARTESIAN_POINT('Ctrl Pts',(-0.0237828037088323,1.99461132721786,
9.32436077871265));
#12844=CARTESIAN_POINT('Ctrl Pts',(-0.027304757952857,1.99456622328742,
9.32458813060584));
#12845=CARTESIAN_POINT('Ctrl Pts',(-0.0335395130969901,1.99446986068405,
9.32498968934213));
#12846=CARTESIAN_POINT('Ctrl Pts',(-0.0362523491747951,1.99442239549463,
9.32516410724176));
#12847=CARTESIAN_POINT('Ctrl Pts',(-0.0419730986466469,1.99431062596545,
9.32553126135294));
#12848=CARTESIAN_POINT('Ctrl Pts',(-0.0449809581585582,1.99424505202991,
9.32572392534565));
#12849=CARTESIAN_POINT('Ctrl Pts',(-0.0530102869146406,1.99405183059469,
9.32623724891666));
#12850=CARTESIAN_POINT('Ctrl Pts',(-0.0580314830086291,1.99391201960316,
9.32655723267571));
#12851=CARTESIAN_POINT('Ctrl Pts',(-0.0817614403357396,1.99316156307402,
9.32806483499531));
#12852=CARTESIAN_POINT('Ctrl Pts',(-0.100462285256823,1.99230653773857,
9.32923933419196));
#12853=CARTESIAN_POINT('Ctrl Pts',(-0.290792935676209,1.98091749373384,
9.34107958778681));
#12854=CARTESIAN_POINT('Ctrl Pts',(-0.460413968350718,1.94849484637778,
9.35073996135217));
#12855=CARTESIAN_POINT('Ctrl Pts',(-0.728487792859784,1.86023718996438,
9.36724926830924));
#12856=CARTESIAN_POINT('Ctrl Pts',(-0.830131529611602,1.81715528857856,
9.37382236719202));
#12857=CARTESIAN_POINT('Ctrl Pts',(-0.939139766533037,1.75988958651772,
9.38150842976427));
#12858=CARTESIAN_POINT('Ctrl Pts',(-0.950531170106828,1.75376319379863,
9.38231959699395));
#12859=CARTESIAN_POINT('Ctrl Pts',(-0.967320904204017,1.74452189973883,
9.38352738591893));
#12860=CARTESIAN_POINT('Ctrl Pts',(-0.972765669432981,1.74149170004331,
9.38392098423441));
#12861=CARTESIAN_POINT('Ctrl Pts',(-0.982303824636207,1.73612470014121,
9.38461391685686));
#12862=CARTESIAN_POINT('Ctrl Pts',(-0.986403317301261,1.73379879839836,
9.3849128577992));
#12863=CARTESIAN_POINT('Ctrl Pts',(-0.994992166194602,1.72888547933815,
9.38554154195178));
#12864=CARTESIAN_POINT('Ctrl Pts',(-0.999479755345363,1.72629505857907,
9.38587139206675));
#12865=CARTESIAN_POINT('Ctrl Pts',(-1.00862211214142,1.72097011643965,9.38654620432678));
#12866=CARTESIAN_POINT('Ctrl Pts',(-1.01327597049019,1.71823412649641,9.38689121791251));
#12867=CARTESIAN_POINT('Ctrl Pts',(-1.02467637512553,1.71146943733045,9.38774011828662));
#12868=CARTESIAN_POINT('Ctrl Pts',(-1.03141028804542,1.70741972679024,9.38824476885135));
#12869=CARTESIAN_POINT('Ctrl Pts',(-1.04991221388023,1.69614345309387,9.38964035162478));
#12870=CARTESIAN_POINT('Ctrl Pts',(-1.06162920438432,1.68883441662369,9.39053429347277));
#12871=CARTESIAN_POINT('Ctrl Pts',(-1.09871092132302,1.66516452479977,9.3933963495681));
#12872=CARTESIAN_POINT('Ctrl Pts',(-1.12377963745658,1.64835000736031,9.39538099027834));
#12873=CARTESIAN_POINT('Ctrl Pts',(-1.22435274191833,1.57753109530907,9.4035512462473));
#12874=CARTESIAN_POINT('Ctrl Pts',(-1.29641730826499,1.51886220450217,9.40990353934877));
#12875=CARTESIAN_POINT('Ctrl Pts',(-1.47601735423118,1.35052491548672,9.42699261916796));
#12876=CARTESIAN_POINT('Ctrl Pts',(-1.57544451244576,1.23309569234885,9.4378580140116));
#12877=CARTESIAN_POINT('Ctrl Pts',(-1.66832843679843,1.09357693157464,9.4489163625842));
#12878=CARTESIAN_POINT('Ctrl Pts',(-1.6760917629886,1.08164074839177,9.44984863238098));
#12879=CARTESIAN_POINT('Ctrl Pts',(-1.68625943703765,1.06563548181358,9.4510793946607));
#12880=CARTESIAN_POINT('Ctrl Pts',(-1.68877785517966,1.06163987588282,9.45138506057795));
#12881=CARTESIAN_POINT('Ctrl Pts',(-1.69268628132033,1.05538984711988,9.45186067535815));
#12882=CARTESIAN_POINT('Ctrl Pts',(-1.69408600998909,1.0531415704141,9.45203125909392));
#12883=CARTESIAN_POINT('Ctrl Pts',(-1.69676457596883,1.04882003695711,9.45235816754792));
#12884=CARTESIAN_POINT('Ctrl Pts',(-1.69804407830334,1.04674724953077,9.45251453386157));
#12885=CARTESIAN_POINT('Ctrl Pts',(-1.7010947871771,1.0417848024119,9.45288786339674));
#12886=CARTESIAN_POINT('Ctrl Pts',(-1.70286242713999,1.03889297049726,9.4531045902612));
#12887=CARTESIAN_POINT('Ctrl Pts',(-1.70815289171911,1.03018807141602,9.45375453280931));
#12888=CARTESIAN_POINT('Ctrl Pts',(-1.71165342847114,1.02436141473171,9.45418631194267));
#12889=CARTESIAN_POINT('Ctrl Pts',(-1.74429471793887,0.969395349991002,
9.45823004829396));
#12890=CARTESIAN_POINT('Ctrl Pts',(-1.77134473905288,0.919037881446591,
9.46171423789622));
#12891=CARTESIAN_POINT('Ctrl Pts',(-1.89070386374988,0.671923166784247,
9.47811141932761));
#12892=CARTESIAN_POINT('Ctrl Pts',(-1.95260856510629,0.462140879230423,
9.49014102357731));
#12893=CARTESIAN_POINT('Ctrl Pts',(-1.98309007296206,0.217355166525072,
9.5052788696862));
#12894=CARTESIAN_POINT('Ctrl Pts',(-1.9860741270961,0.188146027176488,9.507098884177));
#12895=CARTESIAN_POINT('Ctrl Pts',(-1.98916000412274,0.149526392237284,
9.50952751948987));
#12896=CARTESIAN_POINT('Ctrl Pts',(-1.98984156330218,0.14016494601869,9.51011793694034));
#12897=CARTESIAN_POINT('Ctrl Pts',(-1.99082037726254,0.125269689495495,
9.51106022337514));
#12898=CARTESIAN_POINT('Ctrl Pts',(-1.99116069055567,0.11973876985399,9.51141073964354));
#12899=CARTESIAN_POINT('Ctrl Pts',(-1.99175253953599,0.109418396779451,
9.51206597844657));
#12900=CARTESIAN_POINT('Ctrl Pts',(-1.99200985747923,0.104629304441112,
9.51237051722645));
#12901=CARTESIAN_POINT('Ctrl Pts',(-1.9924808427591,0.0952310036940479,
9.51296911607559));
#12902=CARTESIAN_POINT('Ctrl Pts',(-1.99269579357922,0.0906218874647015,
9.51326313387955));
#12903=CARTESIAN_POINT('Ctrl Pts',(-1.99314311743561,0.080257422717421,
9.51392532354307));
#12904=CARTESIAN_POINT('Ctrl Pts',(-1.99336655655012,0.0745017486757097,
9.514293773342));
#12905=CARTESIAN_POINT('Ctrl Pts',(-1.99391674533475,0.058546648621588,
9.51531716629216));
#12906=CARTESIAN_POINT('Ctrl Pts',(-1.99419015815151,0.0483456728499656,
9.51597377308197));
#12907=CARTESIAN_POINT('Ctrl Pts',(-1.99463292918793,0.0251946012443252,
9.51746929279413));
#12908=CARTESIAN_POINT('Ctrl Pts',(-1.9947544595798,0.0122442029112117,
9.51830966718299));
#12909=CARTESIAN_POINT('Ctrl Pts',(-1.99474987500506,-0.000706163778629118,
9.51915393760047));
#12910=CARTESIAN_POINT('',(-1.99474947325114,0.00144964281281663,11.1209548814577));
#12911=CARTESIAN_POINT('Ctrl Pts',(-1.99474987552157,-0.000704703254848296,
9.51915384238488));
#12912=CARTESIAN_POINT('Ctrl Pts',(-1.99466554320306,-0.239417779555123,
9.53471620625515));
#12913=CARTESIAN_POINT('Ctrl Pts',(-1.95172253893193,-0.476180383039018,
9.55181752929714));
#12914=CARTESIAN_POINT('Ctrl Pts',(-1.85711043663534,-0.728791549331281,
9.57016584446524));
#12915=CARTESIAN_POINT('Ctrl Pts',(-1.84551239464581,-0.757681017506495,
9.572260448041));
#12916=CARTESIAN_POINT('Ctrl Pts',(-1.82619143527078,-0.802728078959297,
9.57550810023716));
#12917=CARTESIAN_POINT('Ctrl Pts',(-1.81891942338838,-0.819072471240963,
9.57668252470648));
#12918=CARTESIAN_POINT('Ctrl Pts',(-1.80935781572755,-0.839807300489132,
9.57816536550759));
#12919=CARTESIAN_POINT('Ctrl Pts',(-1.80727069380295,-0.844289433714375,
9.57848547770938));
#12920=CARTESIAN_POINT('Ctrl Pts',(-1.80389427003971,-0.851470475472302,
9.57899760630593));
#12921=CARTESIAN_POINT('Ctrl Pts',(-1.80261554217607,-0.854174288701194,
9.57919026479088));
#12922=CARTESIAN_POINT('Ctrl Pts',(-1.80016304159989,-0.859329957174259,
9.57955729176092));
#12923=CARTESIAN_POINT('Ctrl Pts',(-1.79899035278767,-0.861782259212724,
9.57973172094026));
#12924=CARTESIAN_POINT('Ctrl Pts',(-1.79627169415799,-0.867437728713526,
9.5801336587595));
#12925=CARTESIAN_POINT('Ctrl Pts',(-1.79472216805457,-0.870639163144749,
9.58036094380133));
#12926=CARTESIAN_POINT('Ctrl Pts',(-1.78972313568337,-0.880897473015252,
9.58108850393134));
#12927=CARTESIAN_POINT('Ctrl Pts',(-1.7862404533854,-0.887938234317444,
9.58158675765473));
#12928=CARTESIAN_POINT('Ctrl Pts',(-1.7394767457496,-0.981089403425853,
9.58816650883814));
#12929=CARTESIAN_POINT('Ctrl Pts',(-1.69004532862152,-1.06398683709094,
9.59388492219143));
#12930=CARTESIAN_POINT('Ctrl Pts',(-1.55225840726779,-1.26106112652312,
9.60793369624107));
#12931=CARTESIAN_POINT('Ctrl Pts',(-1.45716866178045,-1.36983199556655,
9.6161427170153));
#12932=CARTESIAN_POINT('Ctrl Pts',(-1.32243864423323,-1.49389142264357,
9.62714637822894));
#12933=CARTESIAN_POINT('Ctrl Pts',(-1.29291237014169,-1.51951731184371,
9.62952262909124));
#12934=CARTESIAN_POINT('Ctrl Pts',(-1.24976377664027,-1.55479750889399,
9.63296009969196));
#12935=CARTESIAN_POINT('Ctrl Pts',(-1.23674270864199,-1.56517482665475,
9.63399303997714));
#12936=CARTESIAN_POINT('Ctrl Pts',(-1.216504699627,-1.58089355894691,9.63559269079468));
#12937=CARTESIAN_POINT('Ctrl Pts',(-1.20937885742552,-1.58635144402778,
9.6361548450625));
#12938=CARTESIAN_POINT('Ctrl Pts',(-1.19753658951515,-1.595295607261,9.63708742078457));
#12939=CARTESIAN_POINT('Ctrl Pts',(-1.1928411412951,-1.59880954720163,9.63745676081658));
#12940=CARTESIAN_POINT('Ctrl Pts',(-1.18369864920448,-1.60558883548575,
9.63817511783331));
#12941=CARTESIAN_POINT('Ctrl Pts',(-1.17925341583401,-1.60885654457168,
9.63852403884496));
#12942=CARTESIAN_POINT('Ctrl Pts',(-1.17477102588897,-1.61212301022304,
9.63887553491039));
#12943=CARTESIAN_POINT('Ctrl Pts',(-1.17474733180471,-1.61214027608537,
9.63887739292243));
#12944=CARTESIAN_POINT('Ctrl Pts',(-1.17469921836505,-1.61217533469059,
9.63888116580047));
#12945=CARTESIAN_POINT('Ctrl Pts',(-1.1746747995976,-1.61219312695551,9.63888308061977));
#12946=CARTESIAN_POINT('Ctrl Pts',(-1.17462520819229,-1.61222925905361,
9.63888696935317));
#12947=CARTESIAN_POINT('Ctrl Pts',(-1.17460003606027,-1.61224759846515,
9.63888894322695));
#12948=CARTESIAN_POINT('Ctrl Pts',(-1.17454890766215,-1.61228484674399,
9.63889295244054));
#12949=CARTESIAN_POINT('Ctrl Pts',(-1.17452295192947,-1.61230375516576,
9.63889498773782));
#12950=CARTESIAN_POINT('Ctrl Pts',(-1.17447022457372,-1.61234216442608,
9.63889912228646));
#12951=CARTESIAN_POINT('Ctrl Pts',(-1.1744434534398,-1.61236166484722,9.63890122149873));
#12952=CARTESIAN_POINT('Ctrl Pts',(-1.17438906180464,-1.61240128230557,
9.63890548650019));
#12953=CARTESIAN_POINT('Ctrl Pts',(-1.17436144176037,-1.61242139894434,
9.63890765225274));
#12954=CARTESIAN_POINT('Ctrl Pts',(-1.17430531706245,-1.61246227430653,
9.6389120530958));
#12955=CARTESIAN_POINT('Ctrl Pts',(-1.17427681281601,-1.61248303266288,
9.63891428815353));
#12956=CARTESIAN_POINT('Ctrl Pts',(-1.17421888240189,-1.61252521841843,
9.63891883053004));
#12957=CARTESIAN_POINT('Ctrl Pts',(-1.17418945666586,-1.61254664542746,
9.63892113781408));
#12958=CARTESIAN_POINT('Ctrl Pts',(-1.1741296440476,-1.61259019682035,9.63892582771611));
#12959=CARTESIAN_POINT('Ctrl Pts',(-1.17409925752153,-1.61261232086323,
9.63892821030521));
#12960=CARTESIAN_POINT('Ctrl Pts',(-1.17403748176703,-1.61265729633212,
9.63893305407281));
#12961=CARTESIAN_POINT('Ctrl Pts',(-1.17400609289531,-1.61268014741046,
9.63893551522229));
#12962=CARTESIAN_POINT('Ctrl Pts',(-1.17394226856811,-1.61272660862848,
9.63894051954815));
#12963=CARTESIAN_POINT('Ctrl Pts',(-1.17390983343254,-1.61275021844041,
9.6389430626983));
#12964=CARTESIAN_POINT('Ctrl Pts',(-1.1738438701572,-1.61279823062703,9.63894823466178));
#12965=CARTESIAN_POINT('Ctrl Pts',(-1.17381034230115,-1.61282263269283,
9.63895086345162));
#12966=CARTESIAN_POINT('Ctrl Pts',(-1.17374214439206,-1.61287226487909,
9.6389562105478));
#12967=CARTESIAN_POINT('Ctrl Pts',(-1.17370747461191,-1.61289749469037,
9.63895892883141));
#12968=CARTESIAN_POINT('Ctrl Pts',(-1.17363694074604,-1.61294881995159,
9.63896445899669));
#12969=CARTESIAN_POINT('Ctrl Pts',(-1.17360107690588,-1.61297491510326,
9.63896727085768));
#12970=CARTESIAN_POINT('Ctrl Pts',(-1.17352809965376,-1.61302801089418,
9.63897299250648));
#12971=CARTESIAN_POINT('Ctrl Pts',(-1.17349098645414,-1.61305501124951,
9.63897590227609));
#12972=CARTESIAN_POINT('Ctrl Pts',(-1.17341545188838,-1.61310995968244,
9.63898182433144));
#12973=CARTESIAN_POINT('Ctrl Pts',(-1.17337703067473,-1.61313790750888,
9.63898483660355));
#12974=CARTESIAN_POINT('Ctrl Pts',(-1.17329881764629,-1.61319479587265,
9.63899096855377));
#12975=CARTESIAN_POINT('Ctrl Pts',(-1.17325902602441,-1.61322373611755,
9.63899408821495));
#12976=CARTESIAN_POINT('Ctrl Pts',(-1.17317800601289,-1.61328265697803,
9.6390004401253));
#12977=CARTESIAN_POINT('Ctrl Pts',(-1.17313677771917,-1.61331263735867,
9.63900367236497));
#12978=CARTESIAN_POINT('Ctrl Pts',(-1.17305281379804,-1.61337368930207,
9.63901025495861));
#12979=CARTESIAN_POINT('Ctrl Pts',(-1.17301007826626,-1.61340476061573,
9.63901360530295));
#12980=CARTESIAN_POINT('Ctrl Pts',(-1.17292302472627,-1.61346804851192,
9.63902042999041));
#12981=CARTESIAN_POINT('Ctrl Pts',(-1.17287870678803,-1.61350026484818,
9.63902390432572));
#12982=CARTESIAN_POINT('Ctrl Pts',(-1.17278840833128,-1.61356590042513,
9.6390309832679));
#12983=CARTESIAN_POINT('Ctrl Pts',(-1.17274242784303,-1.61359931943089,
9.63903458786986));
#12984=CARTESIAN_POINT('Ctrl Pts',(-1.17264871880393,-1.6136674218278,9.63904193403896));
#12985=CARTESIAN_POINT('Ctrl Pts',(-1.17260099025469,-1.61370210498551,
9.63904567560322));
#12986=CARTESIAN_POINT('Ctrl Pts',(-1.17250685220924,-1.61377050639584,
9.63905305525199));
#12987=CARTESIAN_POINT('Ctrl Pts',(-1.17246044299194,-1.61380422462264,
9.63905669331673));
#12988=CARTESIAN_POINT('Ctrl Pts',(-1.16858269558852,-1.61662131384445,
9.63936067076246));
#12989=CARTESIAN_POINT('Ctrl Pts',(-1.16474148675107,-1.61939101430458,
9.63966153659612));
#12990=CARTESIAN_POINT('Ctrl Pts',(-1.15581418950967,-1.62577983999472,
9.64036022324365));
#12991=CARTESIAN_POINT('Ctrl Pts',(-1.15072092402591,-1.62938880637796,
9.64075843089691));
#12992=CARTESIAN_POINT('Ctrl Pts',(-1.13497590430505,-1.64043470664046,
9.64198821857783));
#12993=CARTESIAN_POINT('Ctrl Pts',(-1.12426854242503,-1.64779141924634,
9.64282284271778));
#12994=CARTESIAN_POINT('Ctrl Pts',(-1.00620397309347,-1.72722365243542,
9.65200895816982));
#12995=CARTESIAN_POINT('Ctrl Pts',(-0.892174803386398,-1.78878740911501,
9.66076061035555));
#12996=CARTESIAN_POINT('Ctrl Pts',(-0.679955527685574,-1.87799841786487,
9.67672343276998));
#12997=CARTESIAN_POINT('Ctrl Pts',(-0.584063729278959,-1.90999663084407,
9.68382099476163));
#12998=CARTESIAN_POINT('Ctrl Pts',(-0.44141227310467,-1.94584474734148,
9.6939505215032));
#12999=CARTESIAN_POINT('Ctrl Pts',(-0.396282315762313,-1.9555350975074,
9.69709320179769));
#13000=CARTESIAN_POINT('Ctrl Pts',(-0.327664431831805,-1.96779533980772,
9.7017413691947));
#13001=CARTESIAN_POINT('Ctrl Pts',(-0.3044021385221,-1.97152781837762,9.70329479251749));
#13002=CARTESIAN_POINT('Ctrl Pts',(-0.275710468961657,-1.97561147326816,
9.70517892479128));
#13003=CARTESIAN_POINT('Ctrl Pts',(-0.270339816057213,-1.97635354669309,
9.70553023774412));
#13004=CARTESIAN_POINT('Ctrl Pts',(-0.261896428185398,-1.97748512401847,
9.70608032898307));
#13005=CARTESIAN_POINT('Ctrl Pts',(-0.258825747960257,-1.97788937691783,
9.70627992465509));
#13006=CARTESIAN_POINT('Ctrl Pts',(-0.253080572335661,-1.97863211681487,
9.70665248638472));
#13007=CARTESIAN_POINT('Ctrl Pts',(-0.250406362052425,-1.97897233021321,
9.70682554572711));
#13008=CARTESIAN_POINT('Ctrl Pts',(-0.244326510445079,-1.9797332885553,
9.70721819472701));
#13009=CARTESIAN_POINT('Ctrl Pts',(-0.240920475976034,-1.98015066654216,
9.70743759226989));
#13010=CARTESIAN_POINT('Ctrl Pts',(-0.230783831719392,-1.98136627689524,
9.70808888482382));
#13011=CARTESIAN_POINT('Ctrl Pts',(-0.224050127246862,-1.98213900720012,
9.70851936736008));
#13012=CARTESIAN_POINT('Ctrl Pts',(-0.174984724614378,-1.98751630645788,
9.71164118067062));
#13013=CARTESIAN_POINT('Ctrl Pts',(-0.13251555437737,-1.99079907950381,
9.714262569465));
#13014=CARTESIAN_POINT('Ctrl Pts',(-0.0196481404712469,-1.99589498881153,
9.72109233456169));
#13015=CARTESIAN_POINT('Ctrl Pts',(0.0507980067771298,-1.99534553709103,
9.72521540036741));
#13016=CARTESIAN_POINT('Ctrl Pts',(0.176301232370485,-1.98771401109925,
9.73252892190659));
#13017=CARTESIAN_POINT('Ctrl Pts',(0.231366847896893,-1.98205916045819,
9.73572662113803));
#13018=CARTESIAN_POINT('Ctrl Pts',(0.402190215102142,-1.95730029580344,
9.74576944574804));
#13019=CARTESIAN_POINT('Ctrl Pts',(0.516529115322381,-1.93027818773817,
9.75268493805949));
#13020=CARTESIAN_POINT('Ctrl Pts',(0.641459484615225,-1.88885246677057,
9.76082929595517));
#13021=CARTESIAN_POINT('Ctrl Pts',(0.655044776703003,-1.88418423607092,
9.76172273408732));
#13022=CARTESIAN_POINT('Ctrl Pts',(0.676190539915999,-1.87666171634797,
9.76312617672897));
#13023=CARTESIAN_POINT('Ctrl Pts',(0.683786269615503,-1.87390746257725,
9.76363290336428));
#13024=CARTESIAN_POINT('Ctrl Pts',(0.696515014871994,-1.86920425331903,
9.76448653250431));
#13025=CARTESIAN_POINT('Ctrl Pts',(0.701657140527358,-1.86728009755925,
9.7648326106423));
#13026=CARTESIAN_POINT('Ctrl Pts',(0.711702382026279,-1.86347387004959,
9.76551112530169));
#13027=CARTESIAN_POINT('Ctrl Pts',(0.716606141283242,-1.86159361364236,
9.76584349898133));
#13028=CARTESIAN_POINT('Ctrl Pts',(0.721510347196118,-1.8596909370812,9.76617706461301));
#13029=CARTESIAN_POINT('Ctrl Pts',(0.721518314365015,-1.85968784601311,
9.76617760651293));
#13030=CARTESIAN_POINT('Ctrl Pts',(0.721534265834445,-1.85968165711234,
9.76617869148417));
#13031=CARTESIAN_POINT('Ctrl Pts',(0.721542250180477,-1.85967855926174,
9.7661792345586));
#13032=CARTESIAN_POINT('Ctrl Pts',(0.721558236253706,-1.85967235669838,
9.76618032189585));
#13033=CARTESIAN_POINT('Ctrl Pts',(0.721566237917644,-1.85966925200989,
9.76618086615439));
#13034=CARTESIAN_POINT('Ctrl Pts',(0.721582258588347,-1.85966303578485,
9.76618195585731));
#13035=CARTESIAN_POINT('Ctrl Pts',(0.721590277609264,-1.85965992424254,
9.76618250130267));
#13036=CARTESIAN_POINT('Ctrl Pts',(0.721606333131996,-1.85965369425549,
9.76618359338865));
#13037=CARTESIAN_POINT('Ctrl Pts',(0.721614369605373,-1.85965057582153,
9.76618414002736));
#13038=CARTESIAN_POINT('Ctrl Pts',(0.72163046010647,-1.85964433202189,9.76618523450508));
#13039=CARTESIAN_POINT('Ctrl Pts',(0.721638514110968,-1.85964120666497,
9.76618578234253));
#13040=CARTESIAN_POINT('Ctrl Pts',(0.721654639746199,-1.85963494899073,
9.76618687922267));
#13041=CARTESIAN_POINT('Ctrl Pts',(0.721662711354995,-1.85963181668166,
9.76618742826387));
#13042=CARTESIAN_POINT('Ctrl Pts',(0.72167887236349,-1.85962554503842,9.76618852756278));
#13043=CARTESIAN_POINT('Ctrl Pts',(0.721686961720999,-1.85962240572037,
9.76618907781761));
#13044=CARTESIAN_POINT('Ctrl Pts',(0.721703158011983,-1.85961612014178,
9.76619017952918));
#13045=CARTESIAN_POINT('Ctrl Pts',(0.721711265073703,-1.85961297383121,
9.76619073099466));
#13046=CARTESIAN_POINT('Ctrl Pts',(0.721727497148056,-1.85960667412127,
9.76619183515306));
#13047=CARTESIAN_POINT('Ctrl Pts',(0.721735622082283,-1.85960352075206,
9.76619238784066));
#13048=CARTESIAN_POINT('Ctrl Pts',(0.721751889945942,-1.85959720690685,
9.76619349444638));
#13049=CARTESIAN_POINT('Ctrl Pts',(0.721760032849961,-1.85959404644044,
9.76619404836278));
#13050=CARTESIAN_POINT('Ctrl Pts',(0.721776336582764,-1.85958771842734,
9.76619515742133));
#13051=CARTESIAN_POINT('Ctrl Pts',(0.721784497484633,-1.85958455085201,
9.76619571256846));
#13052=CARTESIAN_POINT('Ctrl Pts',(0.721800837377344,-1.85957820855654,
9.76619682409971));
#13053=CARTESIAN_POINT('Ctrl Pts',(0.721809016376319,-1.85957503383295,
9.76619738048439));
#13054=CARTESIAN_POINT('Ctrl Pts',(0.721825392549674,-1.85956867720658,
9.76619849449663));
#13055=CARTESIAN_POINT('Ctrl Pts',(0.721833589715874,-1.85956549530669,
9.76619905212366));
#13056=CARTESIAN_POINT('Ctrl Pts',(0.72185000242863,-1.85955912424732,9.76620016863459));
#13057=CARTESIAN_POINT('Ctrl Pts',(0.721858217910648,-1.85955593511261,
9.76620072751412));
#13058=CARTESIAN_POINT('Ctrl Pts',(0.721874667083772,-1.85954954964924,
9.76620184651844));
#13059=CARTESIAN_POINT('Ctrl Pts',(0.721882900847955,-1.85954635329194,
9.76620240664823));
#13060=CARTESIAN_POINT('Ctrl Pts',(0.721899387034375,-1.85953995320825,
9.76620352818366));
#13061=CARTESIAN_POINT('Ctrl Pts',(0.721907639313324,-1.85953674953721,
9.76620408957957));
#13062=CARTESIAN_POINT('Ctrl Pts',(0.726328966596836,-1.85782028336506,
9.76650487069316));
#13063=CARTESIAN_POINT('Ctrl Pts',(0.730735897212822,-1.85609132881169,
9.76680561656221));
#13064=CARTESIAN_POINT('Ctrl Pts',(0.740907818592239,-1.85205877565358,
9.76750199343696));
#13065=CARTESIAN_POINT('Ctrl Pts',(0.746668269512591,-1.84974392768006,
9.76789800166783));
#13066=CARTESIAN_POINT('Ctrl Pts',(0.764287970526054,-1.84256770165359,
9.7691143891054));
#13067=CARTESIAN_POINT('Ctrl Pts',(0.776111065680874,-1.83761895888335,
9.76993771707991));
#13068=CARTESIAN_POINT('Ctrl Pts',(0.881362334053054,-1.79236745889032,
9.77733215885068));
#13069=CARTESIAN_POINT('Ctrl Pts',(0.971611860087501,-1.74509173243757,
9.78414492592111));
#13070=CARTESIAN_POINT('Ctrl Pts',(1.17301994279952,-1.61910640238618,9.80045741338772));
#13071=CARTESIAN_POINT('Ctrl Pts',(1.28052117720835,-1.53549473839281,9.81006263172157));
#13072=CARTESIAN_POINT('Ctrl Pts',(1.42220211559756,-1.39999778009519,9.82351572832756));
#13073=CARTESIAN_POINT('Ctrl Pts',(1.46381375293885,-1.35643044474564,9.82757977430909));
#13074=CARTESIAN_POINT('Ctrl Pts',(1.50790516056004,-1.30587008931015,9.83195398429804));
#13075=CARTESIAN_POINT('Ctrl Pts',(1.51238920605761,-1.30067426980741,9.83239966016945));
#13076=CARTESIAN_POINT('Ctrl Pts',(1.51905615678763,-1.29286794856655,9.83306340158647));
#13077=CARTESIAN_POINT('Ctrl Pts',(1.52125928513371,-1.29027490393425,9.83328292075334));
#13078=CARTESIAN_POINT('Ctrl Pts',(1.52502932801671,-1.28581454845004,9.83365886170635));
#13079=CARTESIAN_POINT('Ctrl Pts',(1.52659946094424,-1.28394999529047,9.83381551989977));
#13080=CARTESIAN_POINT('Ctrl Pts',(1.52986447479925,-1.28005829279767,9.83414146230983));
#13081=CARTESIAN_POINT('Ctrl Pts',(1.53155874009731,-1.27803066083866,9.83431070183287));
#13082=CARTESIAN_POINT('Ctrl Pts',(1.53625081250909,-1.27239263794878,9.83477969726562));
#13083=CARTESIAN_POINT('Ctrl Pts',(1.53923994051465,-1.26877499606804,9.83507882373492));
#13084=CARTESIAN_POINT('Ctrl Pts',(1.55110244070676,-1.25431458613355,9.83626747254976));
#13085=CARTESIAN_POINT('Ctrl Pts',(1.55987449940735,-1.24338869028923,9.83714993568137));
#13086=CARTESIAN_POINT('Ctrl Pts',(1.66552277798042,-1.10892219239282,9.84783381853443));
#13087=CARTESIAN_POINT('Ctrl Pts',(1.74761783588492,-0.974434457931812,
9.85674701638314));
#13088=CARTESIAN_POINT('Ctrl Pts',(1.86696717975537,-0.714251545226549,
9.87339736341441));
#13089=CARTESIAN_POINT('Ctrl Pts',(1.90929294823105,-0.591874242693872,
9.88102353686478));
#13090=CARTESIAN_POINT('Ctrl Pts',(1.94271215935481,-0.452865558979571,
9.88993906177004));
#13091=CARTESIAN_POINT('Ctrl Pts',(1.94579656278178,-0.439424020398143,
9.89080337107382));
#13092=CARTESIAN_POINT('Ctrl Pts',(1.95010701342335,-0.419703591321184,
9.89207507303935));
#13093=CARTESIAN_POINT('Ctrl Pts',(1.95144267175982,-0.413448867042847,
9.89247895315575));
#13094=CARTESIAN_POINT('Ctrl Pts',(1.95374141545631,-0.402424797314688,
9.89319178354887));
#13095=CARTESIAN_POINT('Ctrl Pts',(1.95471717913912,-0.397658125598284,
9.89350032570075));
#13096=CARTESIAN_POINT('Ctrl Pts',(1.95658428145294,-0.388364264390364,
9.89410255710767));
#13097=CARTESIAN_POINT('Ctrl Pts',(1.95747737150352,-0.38383745485089,9.89439618825226));
#13098=CARTESIAN_POINT('Ctrl Pts',(1.95982977919919,-0.371692038995564,
9.89518482250007));
#13099=CARTESIAN_POINT('Ctrl Pts',(1.96126036414179,-0.364068010841824,
9.89568073804258));
#13100=CARTESIAN_POINT('Ctrl Pts',(1.96632284253102,-0.336192438968879,
9.89749723045264));
#13101=CARTESIAN_POINT('Ctrl Pts',(1.9696857203306,-0.315893949686496,9.89882630947225));
#13102=CARTESIAN_POINT('Ctrl Pts',(1.99777278921564,-0.128417222707487,
9.91116424253305));
#13103=CARTESIAN_POINT('Ctrl Pts',(2.00146629835545,0.0411853431269605,
9.92287128180867));
#13104=CARTESIAN_POINT('Ctrl Pts',(1.97677137018671,0.275378882401097,9.93929848210391));
#13105=CARTESIAN_POINT('Ctrl Pts',(1.96648131641869,0.341190042158797,9.94393224434978));
#13106=CARTESIAN_POINT('Ctrl Pts',(1.94587602771992,0.44021519068582,9.95083519303516));
#13107=CARTESIAN_POINT('Ctrl Pts',(1.93795336962955,0.47387758460321,9.95316897863299));
#13108=CARTESIAN_POINT('Ctrl Pts',(1.92425515378727,0.525967175611622,9.95674354955565));
#13109=CARTESIAN_POINT('Ctrl Pts',(1.91908079659945,0.544544149766249,9.95801096037916));
#13110=CARTESIAN_POINT('Ctrl Pts',(1.91220526349812,0.567912268300645,9.95959334549513));
#13111=CARTESIAN_POINT('Ctrl Pts',(1.91075429606123,0.572775117906503,9.95992198052444));
#13112=CARTESIAN_POINT('Ctrl Pts',(1.90841023020851,0.580523105905471,9.96044448957));
#13113=CARTESIAN_POINT('Ctrl Pts',(1.90752912185515,0.583411803812091,9.96063905186045));
#13114=CARTESIAN_POINT('Ctrl Pts',(1.90584483789668,0.588889091467024,9.96100748168583));
#13115=CARTESIAN_POINT('Ctrl Pts',(1.90504295701879,0.591478013272316,9.96118141908379));
#13116=CARTESIAN_POINT('Ctrl Pts',(1.90319319811501,0.597407288855301,9.96157931704202));
#13117=CARTESIAN_POINT('Ctrl Pts',(1.90214180251372,0.600746520352626,9.96180306868883));
#13118=CARTESIAN_POINT('Ctrl Pts',(1.89879349967892,0.611283809058716,9.962508131235));
#13119=CARTESIAN_POINT('Ctrl Pts',(1.89646444997975,0.618471700228498,9.96298759254051));
#13120=CARTESIAN_POINT('Ctrl Pts',(1.85548622121049,0.742530034692208,9.97123980166891));
#13121=CARTESIAN_POINT('Ctrl Pts',(1.80613460102611,0.85560960852316,9.97841682517459));
#13122=CARTESIAN_POINT('Ctrl Pts',(1.69833631411699,1.05104361143335,9.9913735853075));
#13123=CARTESIAN_POINT('Ctrl Pts',(1.64348820989429,1.13489393037237,9.99714519583903));
#13124=CARTESIAN_POINT('Ctrl Pts',(1.55189005821547,1.25427558029602,10.0060938429019));
#13125=CARTESIAN_POINT('Ctrl Pts',(1.51969245447149,1.29309870041465,10.0091327791738));
#13126=CARTESIAN_POINT('Ctrl Pts',(1.46588350917848,1.35319176825916,10.0140852685697));
#13127=CARTESIAN_POINT('Ctrl Pts',(1.44519755200979,1.37526226814515,10.0159618368398));
#13128=CARTESIAN_POINT('Ctrl Pts',(1.41794905463334,1.40304068640936,10.0184039171176));
#13129=CARTESIAN_POINT('Ctrl Pts',(1.4118392752602,1.40918861273704,10.0189496248935));
#13130=CARTESIAN_POINT('Ctrl Pts',(1.40191004236041,1.41905044799409,10.0198335870101));
#13131=CARTESIAN_POINT('Ctrl Pts',(1.39811539350248,1.42278926281316,10.0201707387771));
#13132=CARTESIAN_POINT('Ctrl Pts',(1.39084122867069,1.42989919586673,10.0208157921251));
#13133=CARTESIAN_POINT('Ctrl Pts',(1.38736431390615,1.43327293057874,10.0211235758412));
#13134=CARTESIAN_POINT('Ctrl Pts',(1.37937738156402,1.44096655177306,10.0218293864971));
#13135=CARTESIAN_POINT('Ctrl Pts',(1.37485931587067,1.44527797471506,10.0222277763976));
#13136=CARTESIAN_POINT('Ctrl Pts',(1.36087010217768,1.45850240713906,10.0234586782001));
#13137=CARTESIAN_POINT('Ctrl Pts',(1.35133212525532,1.46734392034201,10.0242942422111));
#13138=CARTESIAN_POINT('Ctrl Pts',(1.2516033751738,1.55799340231525,10.0329945744169));
#13139=CARTESIAN_POINT('Ctrl Pts',(1.15420554333993,1.63145767517632,10.0412116130469));
#13140=CARTESIAN_POINT('Ctrl Pts',(0.955808788950157,1.75440273624483,10.0573597662389));
#13141=CARTESIAN_POINT('Ctrl Pts',(0.85611063822225,1.80515196118373,10.0652254429485));
#13142=CARTESIAN_POINT('Ctrl Pts',(0.71208958779295,1.86383424100899,10.0759188473012));
#13143=CARTESIAN_POINT('Ctrl Pts',(0.670951447758556,1.87903548601276,10.0788999464845));
#13144=CARTESIAN_POINT('Ctrl Pts',(0.607753655898465,1.90004754720504,10.0833372034989));
#13145=CARTESIAN_POINT('Ctrl Pts',(0.586041892350024,1.90685610314944,10.0848366269482));
#13146=CARTESIAN_POINT('Ctrl Pts',(0.559074648536351,1.91480856649511,10.0866642501847));
#13147=CARTESIAN_POINT('Ctrl Pts',(0.553925856333002,1.91630437463869,10.0870116401075));
#13148=CARTESIAN_POINT('Ctrl Pts',(0.545806142506566,1.91862782415021,10.0875569651969));
#13149=CARTESIAN_POINT('Ctrl Pts',(0.542839272955747,1.91946935293457,10.087755694763));
#13150=CARTESIAN_POINT('Ctrl Pts',(0.537273423296608,1.92103412481024,10.0881275080933));
#13151=CARTESIAN_POINT('Ctrl Pts',(0.53467495742286,1.92175896773887,10.0883006811837));
#13152=CARTESIAN_POINT('Ctrl Pts',(0.528748479295534,1.92339921008778,10.0886947192377));
#13153=CARTESIAN_POINT('Ctrl Pts',(0.52541956356879,1.92431124259613,10.0889153866973));
#13154=CARTESIAN_POINT('Ctrl Pts',(0.515227879912795,1.92707506869052,10.0895889895652));
#13155=CARTESIAN_POINT('Ctrl Pts',(0.508357473466802,1.92889884945905,10.090040329153));
#13156=CARTESIAN_POINT('Ctrl Pts',(0.454202445240981,1.94296510412912,10.0935774106964));
#13157=CARTESIAN_POINT('Ctrl Pts',(0.406487882822977,1.95350499579497,10.0965709042129));
#13158=CARTESIAN_POINT('Ctrl Pts',(0.336081173830721,1.96636546643905,10.1008732233337));
#13159=CARTESIAN_POINT('Ctrl Pts',(0.313663461052419,1.97006573369058,10.1022262492787));
#13160=CARTESIAN_POINT('Ctrl Pts',(0.185685916817995,1.98894974472243,10.1098787485907));
#13161=CARTESIAN_POINT('Ctrl Pts',(0.0791032665448506,1.99603225096116,
10.1159843263449));
#13162=CARTESIAN_POINT('Ctrl Pts',(-0.145651283860061,1.99292917366836,
10.1290965099994));
#13163=CARTESIAN_POINT('Ctrl Pts',(-0.263368743202459,1.98081093067287,
10.1361096641252));
#13164=CARTESIAN_POINT('Ctrl Pts',(-0.392556735101928,1.95578852129427,
10.1443182708401));
#13165=CARTESIAN_POINT('Ctrl Pts',(-0.405773520362426,1.95308918543334,
10.1451638948004));
#13166=CARTESIAN_POINT('Ctrl Pts',(-0.425158849545157,1.94892475296259,
10.1464131620989));
#13167=CARTESIAN_POINT('Ctrl Pts',(-0.431349601427333,1.94756392960523,
10.1468134689344));
#13168=CARTESIAN_POINT('Ctrl Pts',(-0.442272711072371,1.94510822444996,
10.1475222097685));
#13169=CARTESIAN_POINT('Ctrl Pts',(-0.447007775440067,1.94402551521184,
10.1478302509018));
#13170=CARTESIAN_POINT('Ctrl Pts',(-0.45625125632837,1.94187636490389,10.148433189329));
#13171=CARTESIAN_POINT('Ctrl Pts',(-0.460760008225332,1.94081148999511,
10.1487280344726));
#13172=CARTESIAN_POINT('Ctrl Pts',(-0.472901669886414,1.93789918402654,
10.1495240596415));
#13173=CARTESIAN_POINT('Ctrl Pts',(-0.480527385301628,1.93602238258862,
10.1500261833138));
#13174=CARTESIAN_POINT('Ctrl Pts',(-0.50851484841694,1.92895871252512,10.1518771668622));
#13175=CARTESIAN_POINT('Ctrl Pts',(-0.528804771385689,1.92349539205547,
10.1532349184836));
#13176=CARTESIAN_POINT('Ctrl Pts',(-0.702168362297694,1.87386475707725,
10.1649768033311));
#13177=CARTESIAN_POINT('Ctrl Pts',(-0.849498418499253,1.81183389701955,
10.1759728743808));
#13178=CARTESIAN_POINT('Ctrl Pts',(-1.05351265350642,1.69553846678368,10.1923575302063));
#13179=CARTESIAN_POINT('Ctrl Pts',(-1.11699491278831,1.65440714573147,10.1976313981587));
#13180=CARTESIAN_POINT('Ctrl Pts',(-1.20588764102468,1.58935754766939,10.2051488853783));
#13181=CARTESIAN_POINT('Ctrl Pts',(-1.23324955553266,1.56822136492417,10.2074821561844));
#13182=CARTESIAN_POINT('Ctrl Pts',(-1.27499573129756,1.53420505111607,10.211056028605));
#13183=CARTESIAN_POINT('Ctrl Pts',(-1.28976490938993,1.52181004083861,10.2123232438763));
#13184=CARTESIAN_POINT('Ctrl Pts',(-1.30819190486062,1.50588420923139,10.2139054204633));
#13185=CARTESIAN_POINT('Ctrl Pts',(-1.31201847140064,1.50255144458737,10.2142340382317));
#13186=CARTESIAN_POINT('Ctrl Pts',(-1.31810208535009,1.49721193406086,10.2147565262599));
#13187=CARTESIAN_POINT('Ctrl Pts',(-1.32036733301462,1.49521462977877,10.214951084699));
#13188=CARTESIAN_POINT('Ctrl Pts',(-1.32465691210462,1.49141509093844,10.215319511586));
#13189=CARTESIAN_POINT('Ctrl Pts',(-1.32668208130511,1.48961389745618,10.2154934498785));
#13190=CARTESIAN_POINT('Ctrl Pts',(-1.3313148060788,1.48547659220756,10.2158913555569));
#13191=CARTESIAN_POINT('Ctrl Pts',(-1.33391988421804,1.48313774202744,10.2161151140011));
#13192=CARTESIAN_POINT('Ctrl Pts',(-1.34212809986904,1.47572925083891,10.2168202194162));
#13193=CARTESIAN_POINT('Ctrl Pts',(-1.34770867950719,1.4706345493704,10.2172997164733));
#13194=CARTESIAN_POINT('Ctrl Pts',(-1.44350882101068,1.38217204215057,10.2255358500459));
#13195=CARTESIAN_POINT('Ctrl Pts',(-1.52588224592425,1.29066286106292,10.2326992282234));
#13196=CARTESIAN_POINT('Ctrl Pts',(-1.65917091336927,1.11184906702836,10.2456466970642));
#13197=CARTESIAN_POINT('Ctrl Pts',(-1.71288827551406,1.0271655423483,10.2514228947977));
#13198=CARTESIAN_POINT('Ctrl Pts',(-1.78379974316823,0.894225624335424,
10.2603824399163));
#13199=CARTESIAN_POINT('Ctrl Pts',(-1.80587763974001,0.848755771137132,
10.2634277057106));
#13200=CARTESIAN_POINT('Ctrl Pts',(-1.83839196520735,0.774764665366407,
10.2683896100349));
#13201=CARTESIAN_POINT('Ctrl Pts',(-1.84994557992173,0.746757324311987,
10.2702690821462));
#13202=CARTESIAN_POINT('Ctrl Pts',(-1.86398024679475,0.710408623386117,
10.272714432388));
#13203=CARTESIAN_POINT('Ctrl Pts',(-1.86705115963712,0.702298181752679,
10.2732604399878));
#13204=CARTESIAN_POINT('Ctrl Pts',(-1.87192324935163,0.689172910640475,
10.2741447703062));
#13205=CARTESIAN_POINT('Ctrl Pts',(-1.87375741381474,0.68417037753718,10.2744819887589));
#13206=CARTESIAN_POINT('Ctrl Pts',(-1.87722090588861,0.674605589668786,
10.2751270912739));
#13207=CARTESIAN_POINT('Ctrl Pts',(-1.87885370165126,0.670044624057689,
10.2754348571419));
#13208=CARTESIAN_POINT('Ctrl Pts',(-1.88255262331098,0.65959241844588,10.2761405157749));
#13209=CARTESIAN_POINT('Ctrl Pts',(-1.88460773089371,0.653697359025662,
10.276538770948));
#13210=CARTESIAN_POINT('Ctrl Pts',(-1.89085516959573,0.635502286251923,
10.277768849074));
#13211=CARTESIAN_POINT('Ctrl Pts',(-1.89495494095966,0.623171073353046,
10.2786037182227));
#13212=CARTESIAN_POINT('Ctrl Pts',(-1.93511572345898,0.498314238767923,
10.2870706469722));
#13213=CARTESIAN_POINT('Ctrl Pts',(-1.96122463182681,0.382856144628593,
10.2950333271179));
#13214=CARTESIAN_POINT('Ctrl Pts',(-1.98887519146185,0.177185738021458,
10.3093737644185));
#13215=CARTESIAN_POINT('Ctrl Pts',(-1.99481690562072,0.0878868247181338,
10.3156443863969));
#13216=CARTESIAN_POINT('Ctrl Pts',(-1.99468269327559,-0.0899240165370003,
10.3279929204652));
#13217=CARTESIAN_POINT('Ctrl Pts',(-1.98873717572502,-0.178252210388867,
10.3340578020223));
#13218=CARTESIAN_POINT('Ctrl Pts',(-1.97590266073967,-0.27367445741639,
10.3403469262823));
#13219=CARTESIAN_POINT('Ctrl Pts',(-1.97481170461867,-0.281438749290134,
10.3408567158645));
#13220=CARTESIAN_POINT('Ctrl Pts',(-1.97315972090685,-0.292713015128034,
10.3415939420188));
#13221=CARTESIAN_POINT('Ctrl Pts',(-1.97263506392022,-0.296228119035658,
10.3418233676241));
#13222=CARTESIAN_POINT('Ctrl Pts',(-1.97169260976568,-0.302428837693241,
10.3422273018549));
#13223=CARTESIAN_POINT('Ctrl Pts',(-1.97127871501168,-0.305115023190094,
10.3424020300434));
#13224=CARTESIAN_POINT('Ctrl Pts',(-1.97039760539452,-0.310756806331503,
10.3427684601465));
#13225=CARTESIAN_POINT('Ctrl Pts',(-1.96992923106563,-0.313712194388884,
10.3429600951018));
#13226=CARTESIAN_POINT('Ctrl Pts',(-1.96866837529435,-0.321553874444086,
10.3434677587129));
#13227=CARTESIAN_POINT('Ctrl Pts',(-1.96786434615075,-0.32643832873687,
10.3437831375364));
#13228=CARTESIAN_POINT('Ctrl Pts',(-1.96406090146752,-0.349019339251954,
10.345237484841));
#13229=CARTESIAN_POINT('Ctrl Pts',(-1.96084078798335,-0.366678581940024,
10.3463644327846));
#13230=CARTESIAN_POINT('Ctrl Pts',(-1.95135781817718,-0.414979787523451,
10.3494242008028));
#13231=CARTESIAN_POINT('Ctrl Pts',(-1.94461185341893,-0.445522752541793,
10.3513339241093));
#13232=CARTESIAN_POINT('Ctrl Pts',(-1.91836253740937,-0.552371411078604,
10.3579660146973));
#13233=CARTESIAN_POINT('Ctrl Pts',(-1.89506143481118,-0.627672603519763,
10.3625535576307));
#13234=CARTESIAN_POINT('Ctrl Pts',(-1.81072235196523,-0.852211113602893,
10.3764766998439));
#13235=CARTESIAN_POINT('Ctrl Pts',(-1.7360267200154,-0.995581852369622,
10.3857619067119));
#13236=CARTESIAN_POINT('Ctrl Pts',(-1.63819119571098,-1.13819955652697,
10.3964640605663));
#13237=CARTESIAN_POINT('Ctrl Pts',(-1.63138533480839,-1.14793314446265,
10.3972021331043));
#13238=CARTESIAN_POINT('Ctrl Pts',(-1.61697581630869,-1.16815434130887,
10.3987519890598));
#13239=CARTESIAN_POINT('Ctrl Pts',(-1.60935613241041,-1.17862979010106,
10.3995643499355));
#13240=CARTESIAN_POINT('Ctrl Pts',(-1.59791856831349,-1.19403630024654,
10.4007735781002));
#13241=CARTESIAN_POINT('Ctrl Pts',(-1.59417861635016,-1.19902501016681,
10.4011674114112));
#13242=CARTESIAN_POINT('Ctrl Pts',(-1.58749197189173,-1.20785771527005,
10.4018688122353));
#13243=CARTESIAN_POINT('Ctrl Pts',(-1.58455453879079,-1.21170868366848,
10.4021760143881));
#13244=CARTESIAN_POINT('Ctrl Pts',(-1.57835373001984,-1.21977682363448,
10.4028225989371));
#13245=CARTESIAN_POINT('Ctrl Pts',(-1.57508741558319,-1.22399167844573,
10.4031620961127));
#13246=CARTESIAN_POINT('Ctrl Pts',(-1.56645306968251,-1.23504165009495,
10.4040567072672));
#13247=CARTESIAN_POINT('Ctrl Pts',(-1.56105724514487,-1.24185481051626,
10.404612925718));
#13248=CARTESIAN_POINT('Ctrl Pts',(-1.53653796891897,-1.27240231691258,
10.4071279336413));
#13249=CARTESIAN_POINT('Ctrl Pts',(-1.51691743770921,-1.29573064414492,
10.4091066762781));
#13250=CARTESIAN_POINT('Ctrl Pts',(-1.46308583268472,-1.3568360821527,10.4144512115272));
#13251=CARTESIAN_POINT('Ctrl Pts',(-1.42795046770521,-1.39376505465807,
10.417854010747));
#13252=CARTESIAN_POINT('Ctrl Pts',(-1.31940814578906,-1.49943198723187,
10.4281182357644));
#13253=CARTESIAN_POINT('Ctrl Pts',(-1.24218150381892,-1.56400637401052,
10.43511671074));
#13254=CARTESIAN_POINT('Ctrl Pts',(-1.06137171642551,-1.69332459510875,
10.4506264487829));
#13255=CARTESIAN_POINT('Ctrl Pts',(-0.956026066390776,-1.75495857719636,
10.4591154896717));
#13256=CARTESIAN_POINT('Ctrl Pts',(-0.838841174018736,-1.80981503931484,
10.4675632762204));
#13257=CARTESIAN_POINT('Ctrl Pts',(-0.83195936508958,-1.81298886126467,
10.4680558597143));
#13258=CARTESIAN_POINT('Ctrl Pts',(-0.821868305986221,-1.81757319952556,
10.4687728370571));
#13259=CARTESIAN_POINT('Ctrl Pts',(-0.818673263236856,-1.81901455094251,
10.4689990716429));
#13260=CARTESIAN_POINT('Ctrl Pts',(-0.813000440978043,-1.82155570711824,
10.4693993573033));
#13261=CARTESIAN_POINT('Ctrl Pts',(-0.810524201431194,-1.82265889030597,
10.4695736148504));
#13262=CARTESIAN_POINT('Ctrl Pts',(-0.805286634296978,-1.82497948092575,
10.4699411911807));
#13263=CARTESIAN_POINT('Ctrl Pts',(-0.802524798282799,-1.82619566794335,
10.4701344348243));
#13264=CARTESIAN_POINT('Ctrl Pts',(-0.795120863914019,-1.82943598415184,
10.4706509478164));
#13265=CARTESIAN_POINT('Ctrl Pts',(-0.79047376094071,-1.83144872790875,
10.4709735265204));
#13266=CARTESIAN_POINT('Ctrl Pts',(-0.768202191474188,-1.8409943830577,
10.4725120401972));
#13267=CARTESIAN_POINT('Ctrl Pts',(-0.750476698736424,-1.84829102574646,
10.473714194397));
#13268=CARTESIAN_POINT('Ctrl Pts',(-0.700761556226098,-1.86792293660586,
10.4770314407138));
#13269=CARTESIAN_POINT('Ctrl Pts',(-0.668553818667454,-1.87969118054719,
10.47911841663));
#13270=CARTESIAN_POINT('Ctrl Pts',(-0.549978698530407,-1.91958304491796,
10.4866319796354));
#13271=CARTESIAN_POINT('Ctrl Pts',(-0.462017338625488,-1.94263168315626,
10.4918857392383));
#13272=CARTESIAN_POINT('Ctrl Pts',(-0.218444923609957,-1.98896775611201,
10.50626531036));
#13273=CARTESIAN_POINT('Ctrl Pts',(-0.0612006966267063,-1.99998901408843,
10.5154120990274));
#13274=CARTESIAN_POINT('Ctrl Pts',(0.108221283271541,-1.99185162813035,
10.5260044486931));
#13275=CARTESIAN_POINT('Ctrl Pts',(0.120738291768116,-1.99113209207662,
10.5267909904844));
#13276=CARTESIAN_POINT('Ctrl Pts',(0.139386654024394,-1.98988361011119,
10.5279690494609));
#13277=CARTESIAN_POINT('Ctrl Pts',(0.145523854900972,-1.98944420062125,
10.5283577579322));
#13278=CARTESIAN_POINT('Ctrl Pts',(0.156478410912519,-1.98860891893015,
10.5290534194414));
#13279=CARTESIAN_POINT('Ctrl Pts',(0.16129656585185,-1.98822391664034,10.5293600287945));
#13280=CARTESIAN_POINT('Ctrl Pts',(0.171471354898446,-1.98737365556514,
10.5300088782808));
#13281=CARTESIAN_POINT('Ctrl Pts',(0.176827594360679,-1.98690424362226,
10.5303512466373));
#13282=CARTESIAN_POINT('Ctrl Pts',(0.191035310313647,-1.98560119767137,
10.5312615518225));
#13283=CARTESIAN_POINT('Ctrl Pts',(0.199883144178838,-1.98473003968,10.5318306643262));
#13284=CARTESIAN_POINT('Ctrl Pts',(0.241079576602884,-1.98039557265595,
10.5344910971257));
#13285=CARTESIAN_POINT('Ctrl Pts',(0.273344584231785,-1.97620052549477,
10.5366053077691));
#13286=CARTESIAN_POINT('Ctrl Pts',(0.360611388073228,-1.96267628755898,
10.542410723554));
#13287=CARTESIAN_POINT('Ctrl Pts',(0.415344465229656,-1.95182652943739,
10.5461472710146));
#13288=CARTESIAN_POINT('Ctrl Pts',(0.570926474518173,-1.91414502786993,
10.5570357615523));
#13289=CARTESIAN_POINT('Ctrl Pts',(0.670216771690477,-1.8816786353931,10.5643221754441));
#13290=CARTESIAN_POINT('Ctrl Pts',(0.83725513101289,-1.81215458047431,10.5769378764125));
#13291=CARTESIAN_POINT('Ctrl Pts',(0.906255101035868,-1.77865221175082,
10.5822601569202));
#13292=CARTESIAN_POINT('Ctrl Pts',(1.00433413343109,-1.7238375453336,10.5898440444206));
#13293=CARTESIAN_POINT('Ctrl Pts',(1.03503717104551,-1.70557948507905,10.5922204836509));
#13294=CARTESIAN_POINT('Ctrl Pts',(1.07020772134307,-1.68336495761762,10.5949311421024));
#13295=CARTESIAN_POINT('Ctrl Pts',(1.07516601240073,-1.68020242686342,10.5953130107083));
#13296=CARTESIAN_POINT('Ctrl Pts',(1.08307058966223,-1.67511135709487,10.5959212570056));
#13297=CARTESIAN_POINT('Ctrl Pts',(1.08602583433157,-1.67319689471722,10.5961485389156));
#13298=CARTESIAN_POINT('Ctrl Pts',(1.09124913802191,-1.66979347287572,10.5965500177673));
#13299=CARTESIAN_POINT('Ctrl Pts',(1.09351924558171,-1.66830770039268,10.5967244254786));
#13300=CARTESIAN_POINT('Ctrl Pts',(1.09830077468376,-1.6651642638454,10.5970916053569));
#13301=CARTESIAN_POINT('Ctrl Pts',(1.1008114722812,-1.66350555155278,10.597284305124));
#13302=CARTESIAN_POINT('Ctrl Pts',(1.10750528834206,-1.65906143810388,10.5977978255037));
#13303=CARTESIAN_POINT('Ctrl Pts',(1.11168168448165,-1.65626587624701,10.598117969386));
#13304=CARTESIAN_POINT('Ctrl Pts',(1.13138612333396,-1.64296817194723,10.5996274599238));
#13305=CARTESIAN_POINT('Ctrl Pts',(1.14677681283736,-1.63226283953755,10.6008036473113));
#13306=CARTESIAN_POINT('Ctrl Pts',(1.18902416740431,-1.60198417635024,10.6040312050764));
#13307=CARTESIAN_POINT('Ctrl Pts',(1.21554709772955,-1.58195363059456,10.6060562698114));
#13308=CARTESIAN_POINT('Ctrl Pts',(1.30962893178172,-1.507137472088,10.6132844504131));
#13309=CARTESIAN_POINT('Ctrl Pts',(1.37409103710161,-1.4486087153526,10.618326625315));
#13310=CARTESIAN_POINT('Ctrl Pts',(1.53842146773951,-1.27853110688962,10.6320431346923));
#13311=CARTESIAN_POINT('Ctrl Pts',(1.62988055822566,-1.15968298120237,10.6407137791965));
#13312=CARTESIAN_POINT('Ctrl Pts',(1.71482955068276,-1.01911955222699,10.6508737596746));
#13313=CARTESIAN_POINT('Ctrl Pts',(1.72231697876218,-1.00641405805578,10.6517908609697));
#13314=CARTESIAN_POINT('Ctrl Pts',(1.73478709289562,-0.984706624783944,
10.6533562803772));
#13315=CARTESIAN_POINT('Ctrl Pts',(1.73984233691453,-0.975746909253835,
10.6540019894891));
#13316=CARTESIAN_POINT('Ctrl Pts',(1.74785556818487,-0.96128429740752,10.6550438009375));
#13317=CARTESIAN_POINT('Ctrl Pts',(1.75085744720766,-0.955805830591612,
10.6554383311527));
#13318=CARTESIAN_POINT('Ctrl Pts',(1.75614856084709,-0.94604091261946,10.6561413947038));
#13319=CARTESIAN_POINT('Ctrl Pts',(1.75844796989653,-0.941760007962438,
10.6564495628232));
#13320=CARTESIAN_POINT('Ctrl Pts',(1.76321073800917,-0.932814708538876,
10.6570934170523));
#13321=CARTESIAN_POINT('Ctrl Pts',(1.76567128068277,-0.928148864562311,
10.657429199957));
#13322=CARTESIAN_POINT('Ctrl Pts',(1.77201715713776,-0.915998835188689,
10.6583034927319));
#13323=CARTESIAN_POINT('Ctrl Pts',(1.77587355941238,-0.908499735066821,
10.6588430174788));
#13324=CARTESIAN_POINT('Ctrl Pts',(1.7923323104568,-0.875989068056561,10.6611817766987));
#13325=CARTESIAN_POINT('Ctrl Pts',(1.80445415207244,-0.850739113194671,
10.6629976926831));
#13326=CARTESIAN_POINT('Ctrl Pts',(1.83482268135327,-0.783909782881535,
10.667805233995));
#13327=CARTESIAN_POINT('Ctrl Pts',(1.85218751341452,-0.741949931639712,
10.6708253492995));
#13328=CARTESIAN_POINT('Ctrl Pts',(1.93406376010616,-0.523269127556908,
10.6865719840826));
#13329=CARTESIAN_POINT('Ctrl Pts',(1.97476212276504,-0.33869096451433,10.7000043573005));
#13330=CARTESIAN_POINT('Ctrl Pts',(1.99234660748923,-0.107314659255958,
10.7157704787975));
#13331=CARTESIAN_POINT('Ctrl Pts',(1.99422849045971,-0.0633629374779213,
10.7187123599862));
#13332=CARTESIAN_POINT('Ctrl Pts',(1.99472308297479,-0.0124610671240032,
10.7220318806717));
#13333=CARTESIAN_POINT('Ctrl Pts',(1.99475431136252,-0.00554045743301629,
10.7224813256452));
#13334=CARTESIAN_POINT('Ctrl Pts',(1.99474715998255,0.00479442663909356,
10.7231495620163));
#13335=CARTESIAN_POINT('Ctrl Pts',(1.99473603228525,0.00820857572055919,
10.7233698357902));
#13336=CARTESIAN_POINT('Ctrl Pts',(1.99470044057599,0.0143169061739684,
10.7237630545445));
#13337=CARTESIAN_POINT('Ctrl Pts',(1.99467928378891,0.0170110717114556,
10.7239361825155));
#13338=CARTESIAN_POINT('Ctrl Pts',(1.99462195526506,0.0228141224668951,
10.7243084245484));
#13339=CARTESIAN_POINT('Ctrl Pts',(1.99458397396818,0.025922957433382,10.7245074357078));
#13340=CARTESIAN_POINT('Ctrl Pts',(1.99445903355514,0.0345066210568112,
10.725055821331));
#13341=CARTESIAN_POINT('Ctrl Pts',(1.99435679973447,0.0399812516272016,
10.725404349623));
#13342=CARTESIAN_POINT('Ctrl Pts',(1.99367813474335,0.069755786523588,10.7272935142543));
#13343=CARTESIAN_POINT('Ctrl Pts',(1.99268010159679,0.094045294378193,10.728811638043));
#13344=CARTESIAN_POINT('Ctrl Pts',(1.98837141180654,0.166562388805577,10.7332913557142));
#13345=CARTESIAN_POINT('Ctrl Pts',(1.98375149517328,0.21469653039739,10.7361952091585));
#13346=CARTESIAN_POINT('Ctrl Pts',(1.95626295608673,0.421671505889593,10.7485587241063));
#13347=CARTESIAN_POINT('Ctrl Pts',(1.91602708555336,0.577594475442474,10.7576065949878));
#13348=CARTESIAN_POINT('Ctrl Pts',(1.85427768853177,0.735365328215826,10.7677183957267));
#13349=CARTESIAN_POINT('Ctrl Pts',(1.85095449541226,0.743690369059949,10.7682547377486));
#13350=CARTESIAN_POINT('Ctrl Pts',(1.84297473249911,0.763295897262113,10.7695247313493));
#13351=CARTESIAN_POINT('Ctrl Pts',(1.83827056517342,0.774556526290826,10.7702596001816));
#13352=CARTESIAN_POINT('Ctrl Pts',(1.81403816514736,0.831098570915526,10.7739787031621));
#13353=CARTESIAN_POINT('Ctrl Pts',(1.7929402581437,0.875684819317724,10.7770068549754));
#13354=CARTESIAN_POINT('Ctrl Pts',(1.7657661801811,0.928003477347426,10.7806966048273));
#13355=CARTESIAN_POINT('Ctrl Pts',(1.76125686700291,0.936533448543688,10.7813026062099));
#13356=CARTESIAN_POINT('Ctrl Pts',(1.75378596809602,0.950420858841792,10.7822966393666));
#13357=CARTESIAN_POINT('Ctrl Pts',(1.75086125555542,0.955798039990442,10.7826833612187));
#13358=CARTESIAN_POINT('Ctrl Pts',(1.74558455320622,0.965393939784085,10.7833768169972));
#13359=CARTESIAN_POINT('Ctrl Pts',(1.74324189321838,0.969617755829501,10.7836832156246));
#13360=CARTESIAN_POINT('Ctrl Pts',(1.73825002671792,0.97854152433879,10.7843330355319));
#13361=CARTESIAN_POINT('Ctrl Pts',(1.73559705066357,0.983239313201456,10.7846765904934));
#13362=CARTESIAN_POINT('Ctrl Pts',(1.72848099785841,0.995721607690317,10.7855933838986));
#13363=CARTESIAN_POINT('Ctrl Pts',(1.72398443765877,1.00348678831569,10.7861678279731));
#13364=CARTESIAN_POINT('Ctrl Pts',(1.70249255293058,1.04003063407145,10.7888909654517));
#13365=CARTESIAN_POINT('Ctrl Pts',(1.6848289480676,1.06840806960292,10.791063882541));
#13366=CARTESIAN_POINT('Ctrl Pts',(1.6346257325426,1.14471899921039,10.7970731771369));
#13367=CARTESIAN_POINT('Ctrl Pts',(1.60069983857038,1.19169704020361,10.8009588952385));
#13368=CARTESIAN_POINT('Ctrl Pts',(1.46183224266941,1.36734350565572,10.8162137414634));
#13369=CARTESIAN_POINT('Ctrl Pts',(1.34304586006897,1.4841839929986,10.8280230207915));
#13370=CARTESIAN_POINT('Ctrl Pts',(1.20457537589151,1.5899983065899,10.8398882087009));
#13371=CARTESIAN_POINT('Ctrl Pts',(1.19794907056745,1.59499670193988,10.8404517448334));
#13372=CARTESIAN_POINT('Ctrl Pts',(1.15998333046581,1.62326518944805,10.8436555744936));
#13373=CARTESIAN_POINT('Ctrl Pts',(1.12799482236966,1.64565469744037,10.8462587041124));
#13374=CARTESIAN_POINT('Ctrl Pts',(1.0898313312646,1.67073011290138,10.8492353091764));
#13375=CARTESIAN_POINT('Ctrl Pts',(1.08427715325324,1.67434001884288,10.8496653968606));
#13376=CARTESIAN_POINT('Ctrl Pts',(1.07584626368473,1.67976008090876,10.8503134179153));
#13377=CARTESIAN_POINT('Ctrl Pts',(1.07298280759178,1.68159061829356,10.8505326742979));
#13378=CARTESIAN_POINT('Ctrl Pts',(1.06784200519072,1.68485853012347,10.8509247911943));
#13379=CARTESIAN_POINT('Ctrl Pts',(1.06556642355902,1.68629861289665,10.8510978304081));
#13380=CARTESIAN_POINT('Ctrl Pts',(1.06070105572988,1.68936383902179,10.851466664683));
#13381=CARTESIAN_POINT('Ctrl Pts',(1.05811045780334,1.69098763142009,10.8516623700795));
#13382=CARTESIAN_POINT('Ctrl Pts',(1.05100268997079,1.69542006626987,10.8521974839793));
#13383=CARTESIAN_POINT('Ctrl Pts',(1.04647796233831,1.69821663262926,10.8525361032482));
#13384=CARTESIAN_POINT('Ctrl Pts',(1.03635612263194,1.70441675059738,10.8532892076642));
#13385=CARTESIAN_POINT('Ctrl Pts',(1.03075329425527,1.70781091511418,10.8537031047277));
#13386=CARTESIAN_POINT('Ctrl Pts',(1.01348724605751,1.71815467498233,10.8549698085792));
#13387=CARTESIAN_POINT('Ctrl Pts',(1.00176945093445,1.72501300710784,10.8558172214698));
#13388=CARTESIAN_POINT('Ctrl Pts',(0.957266090258331,1.7504540347863,10.8589932170021));
#13389=CARTESIAN_POINT('Ctrl Pts',(0.924024397900348,1.76822707115688,10.8612795273042));
#13390=CARTESIAN_POINT('Ctrl Pts',(0.764848599869605,1.84761635888256,10.8719212785174));
#13391=CARTESIAN_POINT('Ctrl Pts',(0.633147938843941,1.89678897016429,10.8798673279181));
#13392=CARTESIAN_POINT('Ctrl Pts',(0.398270067624479,1.95726360566081,10.8940972575643));
#13393=CARTESIAN_POINT('Ctrl Pts',(0.297365000135306,1.97511254391445,10.9002235989706));
#13394=CARTESIAN_POINT('Ctrl Pts',(0.182801897187334,1.98639748964364,10.9074103018087));
#13395=CARTESIAN_POINT('Ctrl Pts',(0.170047416009286,1.98752997074415,10.9082134201533));
#13396=CARTESIAN_POINT('Ctrl Pts',(0.151096708408553,1.98902887326342,10.909411499708));
#13397=CARTESIAN_POINT('Ctrl Pts',(0.144908076426884,1.98948931184355,10.9098035085367));
#13398=CARTESIAN_POINT('Ctrl Pts',(0.133889393864926,1.99025742459117,10.910502858357));
#13399=CARTESIAN_POINT('Ctrl Pts',(0.129060161153479,1.9905764140209,10.9108098417131));
#13400=CARTESIAN_POINT('Ctrl Pts',(0.118892520502812,1.99121087006749,10.9114571949216));
#13401=CARTESIAN_POINT('Ctrl Pts',(0.113553916667409,1.99152244968456,10.9117976842396));
#13402=CARTESIAN_POINT('Ctrl Pts',(0.0994670428453642,1.99228778240215,
10.9126977184032));
#13403=CARTESIAN_POINT('Ctrl Pts',(0.0907170012092321,1.99270537765926,
10.9132583921254));
#13404=CARTESIAN_POINT('Ctrl Pts',(0.0508163584331215,1.99434628750642,
10.9158226862553));
#13405=CARTESIAN_POINT('Ctrl Pts',(0.0196439302237547,1.99489682687232,
10.9178472310749));
#13406=CARTESIAN_POINT('Ctrl Pts',(-0.0640937880287946,1.994412918141,10.9233461230898));
#13407=CARTESIAN_POINT('Ctrl Pts',(-0.116623582303313,1.99203138321846,
10.9268601614018));
#13408=CARTESIAN_POINT('Ctrl Pts',(-0.347019774684995,1.97244188629581,
10.9425483617762));
#13409=CARTESIAN_POINT('Ctrl Pts',(-0.522178578381608,1.93346017966513,
10.9552937245448));
#13410=CARTESIAN_POINT('Ctrl Pts',(-0.729662010320395,1.8569938569278,10.9703012580068));
#13411=CARTESIAN_POINT('Ctrl Pts',(-0.769053228237434,1.84102976552721,
10.9731409907176));
#13412=CARTESIAN_POINT('Ctrl Pts',(-0.814101039336908,1.82107466773797,
10.9763535481769));
#13413=CARTESIAN_POINT('Ctrl Pts',(-0.820280538466502,1.81829955979445,
10.976793454484));
#13414=CARTESIAN_POINT('Ctrl Pts',(-0.829568244223379,1.8140716248345,10.9774533167758));
#13415=CARTESIAN_POINT('Ctrl Pts',(-0.832686956982909,1.8126422051683,10.9776746677651));
#13416=CARTESIAN_POINT('Ctrl Pts',(-0.838249645143889,1.81007523646692,
10.9780690596784));
#13417=CARTESIAN_POINT('Ctrl Pts',(-0.840695008634041,1.8089407762612,10.9782422881299));
#13418=CARTESIAN_POINT('Ctrl Pts',(-0.845437063942329,1.80672913526672,
10.9785779249696));
#13419=CARTESIAN_POINT('Ctrl Pts',(-0.847733985157901,1.80565253797444,
10.9787403683061));
#13420=CARTESIAN_POINT('Ctrl Pts',(-0.854277159541992,1.80257042850529,
10.9792027628207));
#13421=CARTESIAN_POINT('Ctrl Pts',(-0.858518429323778,1.80055428205638,
10.9795020609028));
#13422=CARTESIAN_POINT('Ctrl Pts',(-0.876824727420797,1.79177274031775,
10.9807922290948));
#13423=CARTESIAN_POINT('Ctrl Pts',(-0.890817678531163,1.78485715268485,
10.9817741298754));
#13424=CARTESIAN_POINT('Ctrl Pts',(-0.927844073483961,1.76601405747701,
10.9843646793023));
#13425=CARTESIAN_POINT('Ctrl Pts',(-0.950729158841067,1.75380001092075,
10.9859578746841));
#13426=CARTESIAN_POINT('Ctrl Pts',(-1.04893575990428,1.69889846082873,10.9927881506313));
#13427=CARTESIAN_POINT('Ctrl Pts',(-1.12167729766783,1.6517762468957,10.9978329164871));
#13428=CARTESIAN_POINT('Ctrl Pts',(-1.32057934302796,1.50370889556682,11.0122272007663));
#13429=CARTESIAN_POINT('Ctrl Pts',(-1.43783833356192,1.39200716739544,11.0215272898759));
#13430=CARTESIAN_POINT('Ctrl Pts',(-1.54715729279438,1.25914509274536,11.0321742106069));
#13431=CARTESIAN_POINT('Ctrl Pts',(-1.55388909503108,1.25082801644079,11.0328388759933));
#13432=CARTESIAN_POINT('Ctrl Pts',(-1.56909255897397,1.23173213310819,11.0343611495779));
#13433=CARTESIAN_POINT('Ctrl Pts',(-1.57752059250481,1.22091943700962,11.0352204021583));
#13434=CARTESIAN_POINT('Ctrl Pts',(-1.58966496891364,1.2050031889213,11.0364817041372));
#13435=CARTESIAN_POINT('Ctrl Pts',(-1.59346972588795,1.19996734534479,11.0368802687716));
#13436=CARTESIAN_POINT('Ctrl Pts',(-1.60016727531381,1.19101467774119,11.037587980364));
#13437=CARTESIAN_POINT('Ctrl Pts',(-1.60306975969126,1.18710514128067,11.0378967452583));
#13438=CARTESIAN_POINT('Ctrl Pts',(-1.60906922151075,1.17896196619303,11.0385393015672));
#13439=CARTESIAN_POINT('Ctrl Pts',(-1.61216386865649,1.17472666483535,11.0388731802423));
#13440=CARTESIAN_POINT('Ctrl Pts',(-1.6201118699108,1.16375855619813,11.0397370338344));
#13441=CARTESIAN_POINT('Ctrl Pts',(-1.62493993481684,1.1570076287283,11.0402679787043));
#13442=CARTESIAN_POINT('Ctrl Pts',(-1.64518548371286,1.12832225184836,11.0425209836365));
#13443=CARTESIAN_POINT('Ctrl Pts',(-1.66020144550007,1.1061091373075,11.0442582464616));
#13444=CARTESIAN_POINT('Ctrl Pts',(-1.69801759708666,1.04766220825605,11.04881276962));
#13445=CARTESIAN_POINT('Ctrl Pts',(-1.72010621887257,1.01098665059158,11.0516549401773));
#13446=CARTESIAN_POINT('Ctrl Pts',(-1.81212349807512,0.846446118276032,
11.0643380862754));
#13447=CARTESIAN_POINT('Ctrl Pts',(-1.86909260842827,0.71186065329645,11.0745801411154));
#13448=CARTESIAN_POINT('Ctrl Pts',(-1.91766546332463,0.549676539188225,
11.0863390863317));
#13449=CARTESIAN_POINT('Ctrl Pts',(-1.92403797224547,0.526937429217819,
11.087973855698));
#13450=CARTESIAN_POINT('Ctrl Pts',(-1.93382961434331,0.48944825423669,11.0906415798658));
#13451=CARTESIAN_POINT('Ctrl Pts',(-1.93748718911132,0.474763078420624,
11.0916797270721));
#13452=CARTESIAN_POINT('Ctrl Pts',(-1.95275747688053,0.410335096913716,
11.0962008682575));
#13453=CARTESIAN_POINT('Ctrl Pts',(-1.96262537482699,0.360193463234318,
11.0996328524568));
#13454=CARTESIAN_POINT('Ctrl Pts',(-1.9716741461021,0.302622368356984,11.103435111308));
#13455=CARTESIAN_POINT('Ctrl Pts',(-1.97275191807297,0.295514990814411,
11.1039021243318));
#13456=CARTESIAN_POINT('Ctrl Pts',(-1.97429258332861,0.284970841996255,
11.104591265172));
#13457=CARTESIAN_POINT('Ctrl Pts',(-1.97478495967614,0.281538538851066,
11.104815012788));
#13458=CARTESIAN_POINT('Ctrl Pts',(-1.97564471696911,0.275432025900574,
11.1052120372398));
#13459=CARTESIAN_POINT('Ctrl Pts',(-1.97601562110247,0.272758343705778,
11.1053855116788));
#13460=CARTESIAN_POINT('Ctrl Pts',(-1.97672398601088,0.267574772269198,
11.1057211331572));
#13461=CARTESIAN_POINT('Ctrl Pts',(-1.97706209223068,0.265065009508012,
11.1058833169833));
#13462=CARTESIAN_POINT('Ctrl Pts',(-1.97779457931958,0.259548379229047,
11.1062391269904));
#13463=CARTESIAN_POINT('Ctrl Pts',(-1.97818688548416,0.256541235552543,
11.1064326364959));
#13464=CARTESIAN_POINT('Ctrl Pts',(-1.97913716594411,0.249125249240378,
11.1069087854463));
#13465=CARTESIAN_POINT('Ctrl Pts',(-1.97968727101385,0.244715388383343,
11.1071909927869));
#13466=CARTESIAN_POINT('Ctrl Pts',(-1.98236366706657,0.222660544509065,
11.1085978967308));
#13467=CARTESIAN_POINT('Ctrl Pts',(-1.98426889430126,0.204988861766575,
11.1097108448385));
#13468=CARTESIAN_POINT('Ctrl Pts',(-1.99176151173023,0.125541988964189,
11.1146595082694));
#13469=CARTESIAN_POINT('Ctrl Pts',(-1.99470237646159,0.063547673007487,
11.118372994414));
#13470=CARTESIAN_POINT('Ctrl Pts',(-1.99474942627503,0.00151290297884356,
11.1220284394135));
#13471=CARTESIAN_POINT('',(-1.99456005621966,0.000760494868686946,11.9209548813952));
#13472=CARTESIAN_POINT('Ctrl Pts',(-1.99474947325114,0.00144964281281663,
11.1209548814577));
#13473=CARTESIAN_POINT('Ctrl Pts',(-1.99480131921667,-0.069891870774131,
11.1255252561228));
#13474=CARTESIAN_POINT('Ctrl Pts',(-1.99102091811838,-0.141380335692712,
11.1300956307879));
#13475=CARTESIAN_POINT('Ctrl Pts',(-1.98339220536142,-0.212562748880289,
11.134666005453));
#13476=CARTESIAN_POINT('Ctrl Pts',(-1.97608236203098,-0.280769837659475,
11.1390453449075));
#13477=CARTESIAN_POINT('Ctrl Pts',(-1.96523955113442,-0.348695383328597,
11.1434246843619));
#13478=CARTESIAN_POINT('Ctrl Pts',(-1.95090270643391,-0.415940130942959,
11.1478040238164));
#13479=CARTESIAN_POINT('Ctrl Pts',(-1.93657592334818,-0.483137686112946,
11.1521802898452));
#13480=CARTESIAN_POINT('Ctrl Pts',(-1.91876007095681,-0.549654897703523,
11.156556555874));
#13481=CARTESIAN_POINT('Ctrl Pts',(-1.89754557233706,-0.615100287273548,
11.1609328219028));
#13482=CARTESIAN_POINT('Ctrl Pts',(-1.87633826744473,-0.68052348464844,
11.1653076039623));
#13483=CARTESIAN_POINT('Ctrl Pts',(-1.85173475778282,-0.744875100833432,
11.1696823860218));
#13484=CARTESIAN_POINT('Ctrl Pts',(-1.82387543994964,-0.807778399097496,
11.1740571680812));
#13485=CARTESIAN_POINT('Ctrl Pts',(-1.79601546514479,-0.87068318073186,
11.1784320533058));
#13486=CARTESIAN_POINT('Ctrl Pts',(-1.76489973735248,-0.93213911629917,
11.1828069385303));
#13487=CARTESIAN_POINT('Ctrl Pts',(-1.73071614738497,-0.991790895139154,
11.1871818237548));
#13488=CARTESIAN_POINT('Ctrl Pts',(-1.69649783545685,-1.05150326523703,
11.1915611527664));
#13489=CARTESIAN_POINT('Ctrl Pts',(-1.65920569757315,-1.10940738467463,
11.1959404817779));
#13490=CARTESIAN_POINT('Ctrl Pts',(-1.61907217740582,-1.16517502841864,
11.2003198107894));
#13491=CARTESIAN_POINT('Ctrl Pts',(-1.57891446872006,-1.22097628338522,
11.2047017792275));
#13492=CARTESIAN_POINT('Ctrl Pts',(-1.53591228988533,-1.2746381099726,11.2090837476656));
#13493=CARTESIAN_POINT('Ctrl Pts',(-1.49033792455086,-1.32586591823813,
11.2134657161038));
#13494=CARTESIAN_POINT('Ctrl Pts',(-1.44468829793984,-1.37717832384728,
11.2178549209024));
#13495=CARTESIAN_POINT('Ctrl Pts',(-1.39645837009637,-1.42604833939218,
11.2222441257011));
#13496=CARTESIAN_POINT('Ctrl Pts',(-1.34595586245941,-1.4722195416483,11.2266333304997));
#13497=CARTESIAN_POINT('Ctrl Pts',(-1.33057399689337,-1.48628219436312,
11.2279701781398));
#13498=CARTESIAN_POINT('Ctrl Pts',(-1.31498152753624,-1.50009478276201,
11.2293070257799));
#13499=CARTESIAN_POINT('Ctrl Pts',(-1.29918768722309,-1.51365085666012,
11.2306438734201));
#13500=CARTESIAN_POINT('Ctrl Pts',(-1.24656660001067,-1.55881627132221,
11.235097912138));
#13501=CARTESIAN_POINT('Ctrl Pts',(-1.19148327420651,-1.6013238553351,11.239551950856));
#13502=CARTESIAN_POINT('Ctrl Pts',(-1.13423719732462,-1.64089412903611,
11.244005989574));
#13503=CARTESIAN_POINT('Ctrl Pts',(-1.07707717019071,-1.68040492246765,
11.2484533331798));
#13504=CARTESIAN_POINT('Ctrl Pts',(-1.01776124374331,-1.71698689262936,
11.2529006767855));
#13505=CARTESIAN_POINT('Ctrl Pts',(-0.956622630222744,-1.75040015592027,
11.2573480203913));
#13506=CARTESIAN_POINT('Ctrl Pts',(-0.895556092843091,-1.78377402840831,
11.2617901210361));
#13507=CARTESIAN_POINT('Ctrl Pts',(-0.832671563617494,-1.81398637971139,
11.2662322216809));
#13508=CARTESIAN_POINT('Ctrl Pts',(-0.768330434763023,-1.84084108643763,
11.2706743223257));
#13509=CARTESIAN_POINT('Ctrl Pts',(-0.704029892577714,-1.86767885309588,
11.2751136208737));
#13510=CARTESIAN_POINT('Ctrl Pts',(-0.63827502424924,-1.89116298870622,
11.2795529194217));
#13511=CARTESIAN_POINT('Ctrl Pts',(-0.571449601274847,-1.91114439949022,
11.2839922179697));
#13512=CARTESIAN_POINT('Ctrl Pts',(-0.504643624635163,-1.93111999564282,
11.2884302246728));
#13513=CARTESIAN_POINT('Ctrl Pts',(-0.436768180595059,-1.94759475026453,
11.2928682313759));
#13514=CARTESIAN_POINT('Ctrl Pts',(-0.36822300174688,-1.96046917432652,
11.2973062380789));
#13515=CARTESIAN_POINT('Ctrl Pts',(-0.299674478550111,-1.97334422653718,
11.3017444613142));
#13516=CARTESIAN_POINT('Ctrl Pts',(-0.230456637258554,-1.98261851141494,
11.3061826845495));
#13517=CARTESIAN_POINT('Ctrl Pts',(-0.160978461993672,-1.98824382239054,
11.3106209077849));
#13518=CARTESIAN_POINT('Ctrl Pts',(-0.0914266822696495,-1.99387509276232,
11.3150638328279));
#13519=CARTESIAN_POINT('Ctrl Pts',(-0.0216145070355556,-1.99584963392224,
11.3195067578709));
#13520=CARTESIAN_POINT('Ctrl Pts',(0.048045874980268,-1.99417129565075,
11.3239496829139));
#13521=CARTESIAN_POINT('Ctrl Pts',(0.117746920628242,-1.99249197766412,
11.3283952014752));
#13522=CARTESIAN_POINT('Ctrl Pts',(0.187295508419194,-1.98715557353959,
11.3328407200364));
#13523=CARTESIAN_POINT('Ctrl Pts',(0.256284174689232,-1.97821788089782,
11.3372862385977));
#13524=CARTESIAN_POINT('Ctrl Pts',(0.325393228107833,-1.96926459173288,
11.3417395147129));
#13525=CARTESIAN_POINT('Ctrl Pts',(0.393939928096308,-1.95669755763645,
11.3461927908282));
#13526=CARTESIAN_POINT('Ctrl Pts',(0.461527390003027,-1.94062361904028,
11.3506460669434));
#13527=CARTESIAN_POINT('Ctrl Pts',(0.497718532255903,-1.93201648715684,
11.3530306682412));
#13528=CARTESIAN_POINT('Ctrl Pts',(0.533634893021944,-1.92240467714963,
11.355415269539));
#13529=CARTESIAN_POINT('Ctrl Pts',(0.569217740337809,-1.91181032704207,
11.3577998708368));
#13530=CARTESIAN_POINT('Ctrl Pts',(0.63568058248553,-1.89202184264661,11.3622539095548));
#13531=CARTESIAN_POINT('Ctrl Pts',(0.701241918662385,-1.86872423163233,
11.3667079482728));
#13532=CARTESIAN_POINT('Ctrl Pts',(0.765504628151487,-1.84201797677945,
11.3711619869908));
#13533=CARTESIAN_POINT('Ctrl Pts',(0.829670740803476,-1.81535186557707,
11.3756093305965));
#13534=CARTESIAN_POINT('Ctrl Pts',(0.892541652685848,-1.78528746619354,
11.3800566742023));
#13535=CARTESIAN_POINT('Ctrl Pts',(0.953735274802135,-1.75197505350336,
11.384504017808));
#13536=CARTESIAN_POINT('Ctrl Pts',(1.01485675592812,-1.71870191272351,11.3889461184528));
#13537=CARTESIAN_POINT('Ctrl Pts',(1.07430444665581,-1.68218859660003,11.3933882190976));
#13538=CARTESIAN_POINT('Ctrl Pts',(1.1317177927405,-1.64263276483046,11.3978303197424));
#13539=CARTESIAN_POINT('Ctrl Pts',(1.18909492223215,-1.6031018850548,11.4022696182904));
#13540=CARTESIAN_POINT('Ctrl Pts',(1.24443985059334,-1.56053257405536,11.4067089168385));
#13541=CARTESIAN_POINT('Ctrl Pts',(1.29741944767327,-1.5151667694677,11.4111482153865));
#13542=CARTESIAN_POINT('Ctrl Pts',(1.35038362758203,-1.46981416642201,11.4155862220895));
#13543=CARTESIAN_POINT('Ctrl Pts',(1.40098347095676,-1.42166700353641,11.4200242287926));
#13544=CARTESIAN_POINT('Ctrl Pts',(1.44891891168712,-1.37100749445632,11.4244622354957));
#13545=CARTESIAN_POINT('Ctrl Pts',(1.49685669120806,-1.3203455136772,11.428900458731));
#13546=CARTESIAN_POINT('Ctrl Pts',(1.54212947525079,-1.26717130058426,11.4333386819663));
#13547=CARTESIAN_POINT('Ctrl Pts',(1.58447530493118,-1.21180261204672,11.4377769052016));
#13548=CARTESIAN_POINT('Ctrl Pts',(1.62686599534494,-1.15637526649402,11.4422198302446));
#13549=CARTESIAN_POINT('Ctrl Pts',(1.6663232443781,-1.09874919494268,11.4466627552876));
#13550=CARTESIAN_POINT('Ctrl Pts',(1.70262712490201,-1.03927303248372,11.4511056803307));
#13551=CARTESIAN_POINT('Ctrl Pts',(1.73895219749533,-0.979762151340572,
11.4555511988919));
#13552=CARTESIAN_POINT('Ctrl Pts',(1.77212000491597,-0.918399460529095,
11.4599967174532));
#13553=CARTESIAN_POINT('Ctrl Pts',(1.80195685377863,-0.855557747682884,
11.4644422360144));
#13554=CARTESIAN_POINT('Ctrl Pts',(1.83184576877543,-0.792606374293586,
11.4688955121297));
#13555=CARTESIAN_POINT('Ctrl Pts',(1.85839193572584,-0.728171279465302,
11.4733487882449));
#13556=CARTESIAN_POINT('Ctrl Pts',(1.88147030347454,-0.662643991630075,
11.4778020643602));
#13557=CARTESIAN_POINT('Ctrl Pts',(1.89382810574432,-0.627556013348388,
11.480186665658));
#13558=CARTESIAN_POINT('Ctrl Pts',(1.90519244737116,-0.592155115030856,
11.4825712669558));
#13559=CARTESIAN_POINT('Ctrl Pts',(1.91555014288408,-0.55650266180565,11.4849558682536));
#13560=CARTESIAN_POINT('Ctrl Pts',(1.93489659584712,-0.489909807393396,
11.4894099069716));
#13561=CARTESIAN_POINT('Ctrl Pts',(1.95080463819388,-0.422175018186061,
11.4938639456896));
#13562=CARTESIAN_POINT('Ctrl Pts',(1.96314374571715,-0.353686578981496,
11.4983179844075));
#13563=CARTESIAN_POINT('Ctrl Pts',(1.97546430564468,-0.285301088542166,
11.5027653280133));
#13564=CARTESIAN_POINT('Ctrl Pts',(1.98422649217828,-0.216164674414784,
11.5072126716191));
#13565=CARTESIAN_POINT('Ctrl Pts',(1.98934978254012,-0.146679941394854,
11.5116600152248));
#13566=CARTESIAN_POINT('Ctrl Pts',(1.99446703306922,-0.0772771237329385,
11.5161021158696));
#13567=CARTESIAN_POINT('Ctrl Pts',(1.99595387185215,-0.00752728862473041,
11.5205442165144));
#13568=CARTESIAN_POINT('Ctrl Pts',(1.99378127442722,0.0621594099342622,
11.5249863171592));
#13569=CARTESIAN_POINT('Ctrl Pts',(1.99161004748637,0.131802149815071,11.5294256157072));
#13570=CARTESIAN_POINT('Ctrl Pts',(1.98578397886954,0.201381343966332,11.5338649142553));
#13571=CARTESIAN_POINT('Ctrl Pts',(1.97632611885387,0.270485922805627,11.5383042128033));
#13572=CARTESIAN_POINT('Ctrl Pts',(1.9668710110948,0.339570392071139,11.5427422195063));
#13573=CARTESIAN_POINT('Ctrl Pts',(1.95378627631826,0.408180035411662,11.5471802262094));
#13574=CARTESIAN_POINT('Ctrl Pts',(1.93714672842288,0.475909776176658,11.5516182329125));
#13575=CARTESIAN_POINT('Ctrl Pts',(1.92050636867686,0.543642821504602,11.5560564561478));
#13576=CARTESIAN_POINT('Ctrl Pts',(1.90031097059076,0.610495404171167,11.5604946793831));
#13577=CARTESIAN_POINT('Ctrl Pts',(1.87668586299971,0.676075242940492,11.5649329026184));
#13578=CARTESIAN_POINT('Ctrl Pts',(1.8530357272144,0.741724556311701,11.5693758276614));
#13579=CARTESIAN_POINT('Ctrl Pts',(1.82594879609034,0.806097973076582,11.5738187527044));
#13580=CARTESIAN_POINT('Ctrl Pts',(1.79559911605028,0.868821832678858,11.5782616777475));
#13581=CARTESIAN_POINT('Ctrl Pts',(1.76523171965278,0.931582306779709,11.5827071963087));
#13582=CARTESIAN_POINT('Ctrl Pts',(1.73159801957856,0.992690878126272,11.58715271487));
#13583=CARTESIAN_POINT('Ctrl Pts',(1.69491740017859,1.05179968105712,11.5915982334312));
#13584=CARTESIAN_POINT('Ctrl Pts',(1.6581727720738,1.11101163049915,11.5960515095465));
#13585=CARTESIAN_POINT('Ctrl Pts',(1.61837089061509,1.16821644373751,11.6005047856617));
#13586=CARTESIAN_POINT('Ctrl Pts',(1.57577323210027,1.22309700494126,11.6049580617769));
#13587=CARTESIAN_POINT('Ctrl Pts',(1.55296341093742,1.2524839672772,11.6073426630747));
#13588=CARTESIAN_POINT('Ctrl Pts',(1.52935262853928,1.28120508871815,11.6097272643725));
#13589=CARTESIAN_POINT('Ctrl Pts',(1.5049853393288,1.30921605967288,11.6121118656703));
#13590=CARTESIAN_POINT('Ctrl Pts',(1.45947129482322,1.36153589581327,11.6165659043883));
#13591=CARTESIAN_POINT('Ctrl Pts',(1.41113556380725,1.41158311938672,11.6210199431063));
#13592=CARTESIAN_POINT('Ctrl Pts',(1.36023393229373,1.45903776919473,11.6254739818242));
#13593=CARTESIAN_POINT('Ctrl Pts',(1.30940881384106,1.50642108729096,11.62992132543));
#13594=CARTESIAN_POINT('Ctrl Pts',(1.25602580513888,1.55121923516703,11.6343686690358));
#13595=CARTESIAN_POINT('Ctrl Pts',(1.20037980321197,1.59314653768597,11.6388160126415));
#13596=CARTESIAN_POINT('Ctrl Pts',(1.14479940220149,1.63502441222494,11.6432581132863));
#13597=CARTESIAN_POINT('Ctrl Pts',(1.08696169573552,1.67403787013299,11.6477002139311));
#13598=CARTESIAN_POINT('Ctrl Pts',(1.02719580968401,1.70994044664357,11.6521423145759));
#13599=CARTESIAN_POINT('Ctrl Pts',(0.967467624218168,1.74582037564985,11.6565816131239));
#13600=CARTESIAN_POINT('Ctrl Pts',(0.905814090722211,1.77859306461083,11.6610209116719));
#13601=CARTESIAN_POINT('Ctrl Pts',(0.842593298733142,1.80805533527876,11.6654602102199));
#13602=CARTESIAN_POINT('Ctrl Pts',(0.779390904123909,1.83750903236565,11.669898216923));
#13603=CARTESIAN_POINT('Ctrl Pts',(0.71462259991777,1.86365401685104,11.6743362236261));
#13604=CARTESIAN_POINT('Ctrl Pts',(0.648669462487063,1.88633387578571,11.6787742303291));
#13605=CARTESIAN_POINT('Ctrl Pts',(0.582713107174641,1.90901484128038,11.6832124535644));
#13606=CARTESIAN_POINT('Ctrl Pts',(0.515572267596593,1.92823018863076,11.6876506767997));
#13607=CARTESIAN_POINT('Ctrl Pts',(0.447644611669163,1.94387290328961,11.692088900035));
#13608=CARTESIAN_POINT('Ctrl Pts',(0.379644993886647,1.95953218967834,11.6965318250781));
#13609=CARTESIAN_POINT('Ctrl Pts',(0.310857374064267,1.97161117899342,11.7009747501211));
#13610=CARTESIAN_POINT('Ctrl Pts',(0.241690140920874,1.98005389782239,11.7054176751641));
#13611=CARTESIAN_POINT('Ctrl Pts',(0.172482532016436,1.98850154501387,11.7098631937254));
#13612=CARTESIAN_POINT('Ctrl Pts',(0.102895357275272,1.99330866309628,11.7143087122866));
#13613=CARTESIAN_POINT('Ctrl Pts',(0.0333398646557803,1.9944713625231,11.7187542308479));
#13614=CARTESIAN_POINT('Ctrl Pts',(-0.0363370042399317,1.99563609089286,
11.7232075069631));
#13615=CARTESIAN_POINT('Ctrl Pts',(-0.105981591456101,1.99314372318742,
11.7276607830783));
#13616=CARTESIAN_POINT('Ctrl Pts',(-0.175185713106997,1.98704240730368,
11.7321140591936));
#13617=CARTESIAN_POINT('Ctrl Pts',(-0.212242530163042,1.98377532810216,
11.7344986604914));
#13618=CARTESIAN_POINT('Ctrl Pts',(-0.249173186378843,1.979474340568,11.7368832617892));
#13619=CARTESIAN_POINT('Ctrl Pts',(-0.285916359980977,1.97415283035413,
11.739267863087));
#13620=CARTESIAN_POINT('Ctrl Pts',(-0.354546498694724,1.96421313412377,
11.743721901805));
#13621=CARTESIAN_POINT('Ctrl Pts',(-0.422793615799594,1.95067066436604,
11.748175940523));
#13622=CARTESIAN_POINT('Ctrl Pts',(-0.490250215933375,1.93356724431225,
11.752629979241));
#13623=CARTESIAN_POINT('Ctrl Pts',(-0.55760541831628,1.9164895333562,11.7570773228467));
#13624=CARTESIAN_POINT('Ctrl Pts',(-0.624171991471304,1.89586161514751,
11.7615246664525));
#13625=CARTESIAN_POINT('Ctrl Pts',(-0.689550091135187,1.87177675867488,
11.7659720100582));
#13626=CARTESIAN_POINT('Ctrl Pts',(-0.754851116739743,1.84772029577237,
11.770414110703));
#13627=CARTESIAN_POINT('Ctrl Pts',(-0.818965994427438,1.82021515722925,
11.7748562113478));
#13628=CARTESIAN_POINT('Ctrl Pts',(-0.881509314446687,1.78940461915234,
11.7792983119926));
#13629=CARTESIAN_POINT('Ctrl Pts',(-0.944013181862676,1.75861351649931,
11.7837376105406));
#13630=CARTESIAN_POINT('Ctrl Pts',(-1.00494702006678,1.7245213664352,11.7881769090886));
#13631=CARTESIAN_POINT('Ctrl Pts',(-1.06394613150128,1.68731923232193,11.7926162076367));
#13632=CARTESIAN_POINT('Ctrl Pts',(-1.12292807407352,1.65012792410587,11.7970542143397));
#13633=CARTESIAN_POINT('Ctrl Pts',(-1.17997599364078,1.60982868941689,11.8014922210428));
#13634=CARTESIAN_POINT('Ctrl Pts',(-1.2347520655769,1.56665723725822,11.8059302277459));
#13635=CARTESIAN_POINT('Ctrl Pts',(-1.28953081006082,1.52348367874609,11.8103684509811));
#13636=CARTESIAN_POINT('Ctrl Pts',(-1.34203710383137,1.47743792945814,11.8148066742164));
#13637=CARTESIAN_POINT('Ctrl Pts',(-1.39196567148208,1.42879639274301,11.8192448974517));
#13638=CARTESIAN_POINT('Ctrl Pts',(-1.44194713294038,1.38010332568753,11.8236878224947));
#13639=CARTESIAN_POINT('Ctrl Pts',(-1.48934506633877,1.32880932473937,11.8281307475378));
#13640=CARTESIAN_POINT('Ctrl Pts',(-1.53389130511928,1.27522744111765,11.8325736725808));
#13641=CARTESIAN_POINT('Ctrl Pts',(-1.57846354737293,1.22161427954498,11.8370191911421));
#13642=CARTESIAN_POINT('Ctrl Pts',(-1.62018048883087,1.1657109695526,11.8414647097033));
#13643=CARTESIAN_POINT('Ctrl Pts',(-1.65881620481107,1.10786116510878,11.8459102282646));
#13644=CARTESIAN_POINT('Ctrl Pts',(-1.69751934119421,1.04991041114129,11.8503635043798));
#13645=CARTESIAN_POINT('Ctrl Pts',(-1.73313026885596,0.990006803099989,
11.854816780495));
#13646=CARTESIAN_POINT('Ctrl Pts',(-1.76546847291161,0.928519592499352,
11.8592700566103));
#13647=CARTESIAN_POINT('Ctrl Pts',(-1.78278465124067,0.89559495939712,11.8616546579081));
#13648=CARTESIAN_POINT('Ctrl Pts',(-1.79916325838748,0.862216626750999,
11.8640392592059));
#13649=CARTESIAN_POINT('Ctrl Pts',(-1.81458234810586,0.828443398454376,
11.8664238605037));
#13650=CARTESIAN_POINT('Ctrl Pts',(-1.84597961350514,0.75967234701184,11.8712795271602));
#13651=CARTESIAN_POINT('Ctrl Pts',(-1.87350349450898,0.689026870672636,
11.8761351938167));
#13652=CARTESIAN_POINT('Ctrl Pts',(-1.89694749304094,0.61694227537565,11.8809908604732));
#13653=CARTESIAN_POINT('Ctrl Pts',(-1.92032753640226,0.545054326678276,
11.8858332808829));
#13654=CARTESIAN_POINT('Ctrl Pts',(-1.93964974790703,0.471735397355194,
11.8906757012927));
#13655=CARTESIAN_POINT('Ctrl Pts',(-1.9547553251231,0.397440789807616,11.8955181217024));
#13656=CARTESIAN_POINT('Ctrl Pts',(-1.96979393975964,0.323475528070162,
11.9003390758049));
#13657=CARTESIAN_POINT('Ctrl Pts',(-1.98065308357961,0.24854353722681,11.9051600299073));
#13658=CARTESIAN_POINT('Ctrl Pts',(-1.98722406893279,0.173112860164138,
11.9099809840098));
#13659=CARTESIAN_POINT('Ctrl Pts',(-1.9922098952135,0.115878787668584,11.9136389498049));
#13660=CARTESIAN_POINT('Ctrl Pts',(-1.99472789398327,0.0583580291533336,
11.9172969156001));
#13661=CARTESIAN_POINT('Ctrl Pts',(-1.99474985500375,0.000760567236024933,
11.9209548813952));
#13662=CARTESIAN_POINT('',(-1.99382857833478,-0.00178311501442863,12.7209548813952));
#13663=CARTESIAN_POINT('Ctrl Pts',(-1.99173490036883,0.00075941768049894,
11.9209548813952));
#13664=CARTESIAN_POINT('Ctrl Pts',(-1.99043489393824,-0.379843555327031,
11.9451632069036));
#13665=CARTESIAN_POINT('Ctrl Pts',(-1.70198160698615,-1.42865295746539,
12.0117568648843));
#13666=CARTESIAN_POINT('Ctrl Pts',(-0.00405728410159747,-2.35857299970061,
12.1207358553372));
#13667=CARTESIAN_POINT('Ctrl Pts',(1.98079133142009,-1.28037055489497,12.2478918527539));
#13668=CARTESIAN_POINT('Ctrl Pts',(2.14890506846846,0.972157427159623,12.3750478501707));
#13669=CARTESIAN_POINT('Ctrl Pts',(0.346093990525894,2.33304565025909,12.5022038475874));
#13670=CARTESIAN_POINT('Ctrl Pts',(-1.57649463483796,1.62673220971673,12.6175061913289));
#13671=CARTESIAN_POINT('Ctrl Pts',(-1.98970252853481,0.476968094023456,
12.6904232025982));
#13672=CARTESIAN_POINT('Ctrl Pts',(-1.99382857833478,-0.00178311501442863,
12.7209548813952));
#13673=CARTESIAN_POINT('',(-1.99474927319053,0.00170282290857631,14.3209548813952));
#13674=CARTESIAN_POINT('Ctrl Pts',(-1.99474916918916,-0.00182058209230188,
12.7204256504633));
#13675=CARTESIAN_POINT('Ctrl Pts',(-1.99460679830126,-0.157811466306289,
12.7312264087668));
#13676=CARTESIAN_POINT('Ctrl Pts',(-1.97616778132757,-0.31325526735429,
12.7423019706705));
#13677=CARTESIAN_POINT('Ctrl Pts',(-1.93667103452653,-0.478030541023614,
12.7535601346536));
#13678=CARTESIAN_POINT('Ctrl Pts',(-1.93340893355319,-0.49105784999197,
12.7544464877575));
#13679=CARTESIAN_POINT('Ctrl Pts',(-1.92837319535795,-0.510339709358736,
12.7557518529825));
#13680=CARTESIAN_POINT('Ctrl Pts',(-1.92670022090365,-0.516619841895187,
12.7561759781784));
#13681=CARTESIAN_POINT('Ctrl Pts',(-1.92359608508044,-0.528047542457987,
12.7569457143287));
#13682=CARTESIAN_POINT('Ctrl Pts',(-1.92217488677198,-0.533197723076139,
12.7572918624728));
#13683=CARTESIAN_POINT('Ctrl Pts',(-1.9199018539286,-0.541307600311889,
12.7578356783885));
#13684=CARTESIAN_POINT('Ctrl Pts',(-1.91906384055371,-0.544271093361395,
12.7580341333404));
#13685=CARTESIAN_POINT('Ctrl Pts',(-1.91747870536807,-0.54982748025022,
12.7584057123258));
#13686=CARTESIAN_POINT('Ctrl Pts',(-1.91673319421761,-0.552420768865559,
12.7585789244244));
#13687=CARTESIAN_POINT('Ctrl Pts',(-1.91502024271313,-0.558334121172091,
12.7589734164481));
#13688=CARTESIAN_POINT('Ctrl Pts',(-1.91404943156409,-0.561653180207082,
12.7591944971162));
#13689=CARTESIAN_POINT('Ctrl Pts',(-1.91104739346366,-0.571818519507528,
12.7598706075471));
#13690=CARTESIAN_POINT('Ctrl Pts',(-1.90898800145358,-0.578656524494429,
12.7603240241146));
#13691=CARTESIAN_POINT('Ctrl Pts',(-1.89228835616597,-0.633046479359327,
12.7639205456607));
#13692=CARTESIAN_POINT('Ctrl Pts',(-1.87590895521207,-0.680051187043739,
12.766967896101));
#13693=CARTESIAN_POINT('Ctrl Pts',(-1.85122230962036,-0.743188074175726,
12.7710398230691));
#13694=CARTESIAN_POINT('Ctrl Pts',(-1.8444300470715,-0.759888402771221,
12.7721147940824));
#13695=CARTESIAN_POINT('Ctrl Pts',(-1.80315008930699,-0.85756877825328,
12.7784023528058));
#13696=CARTESIAN_POINT('Ctrl Pts',(-1.7635581713491,-0.936289686919568,
12.7834734917473));
#13697=CARTESIAN_POINT('Ctrl Pts',(-1.68905244863127,-1.06282096944462,
12.7919988403461));
#13698=CARTESIAN_POINT('Ctrl Pts',(-1.65698452241267,-1.11215487093237,
12.7954259849033));
#13699=CARTESIAN_POINT('Ctrl Pts',(-1.57930105486164,-1.22083051713804,
12.8033327871925));
#13700=CARTESIAN_POINT('Ctrl Pts',(-1.53243537248501,-1.27916337219581,
12.8078405023811));
#13701=CARTESIAN_POINT('Ctrl Pts',(-1.47031737710255,-1.34815465818939,
12.8136028579882));
#13702=CARTESIAN_POINT('Ctrl Pts',(-1.45804320789259,-1.36141989920375,
12.8147319234833));
#13703=CARTESIAN_POINT('Ctrl Pts',(-1.44179249904295,-1.37851091291772,
12.8162153862357));
#13704=CARTESIAN_POINT('Ctrl Pts',(-1.43797768360073,-1.38248982918874,
12.8165628239745));
#13705=CARTESIAN_POINT('Ctrl Pts',(-1.43042839098918,-1.3902988154367,12.8172488422753));
#13706=CARTESIAN_POINT('Ctrl Pts',(-1.42669490061373,-1.39412977789228,
12.817587378461));
#13707=CARTESIAN_POINT('Ctrl Pts',(-1.41955456083233,-1.40139781330903,
12.8182334685947));
#13708=CARTESIAN_POINT('Ctrl Pts',(-1.41615051977085,-1.40483760164717,
12.8185408978828));
#13709=CARTESIAN_POINT('Ctrl Pts',(-1.40835499247842,-1.41265786775097,
12.8192436305046));
#13710=CARTESIAN_POINT('Ctrl Pts',(-1.40395554084635,-1.41703030103379,
12.819639285598));
#13711=CARTESIAN_POINT('Ctrl Pts',(-1.39042276542373,-1.43035508100822,
12.820853529247));
#13712=CARTESIAN_POINT('Ctrl Pts',(-1.38122382111978,-1.43924003129459,
12.8216750514602));
#13713=CARTESIAN_POINT('Ctrl Pts',(-1.29831278994866,-1.51779401831155,
12.8290465316095));
#13714=CARTESIAN_POINT('Ctrl Pts',(-1.21948442709691,-1.58182383899944,
12.8358365595217));
#13715=CARTESIAN_POINT('Ctrl Pts',(-1.01476707034905,-1.7236823899953,12.8529359269563));
#13716=CARTESIAN_POINT('Ctrl Pts',(-0.884437241337347,-1.7940460025461,
12.8634072685098));
#13717=CARTESIAN_POINT('Ctrl Pts',(-0.716745461652485,-1.86182887998794,
12.8757356395092));
#13718=CARTESIAN_POINT('Ctrl Pts',(-0.685642474360487,-1.87350620538434,
12.8779751074788));
#13719=CARTESIAN_POINT('Ctrl Pts',(-0.636620266354247,-1.89052661724212,
12.8814168954455));
#13720=CARTESIAN_POINT('Ctrl Pts',(-0.618894044152356,-1.8964035641936,
12.8826437936863));
#13721=CARTESIAN_POINT('Ctrl Pts',(-0.596262042720049,-1.90355581625355,
12.8841856328525));
#13722=CARTESIAN_POINT('Ctrl Pts',(-0.591431099653924,-1.90506231522886,
12.8845133326984));
#13723=CARTESIAN_POINT('Ctrl Pts',(-0.583710941702521,-1.90743760068412,
12.8850347029975));
#13724=CARTESIAN_POINT('Ctrl Pts',(-0.580825438647956,-1.90831823186895,
12.8852290565953));
#13725=CARTESIAN_POINT('Ctrl Pts',(-0.575343114859659,-1.90997780424531,
12.8855973277552));
#13726=CARTESIAN_POINT('Ctrl Pts',(-0.57274673620158,-1.9107579880196,12.885771314185));
#13727=CARTESIAN_POINT('Ctrl Pts',(-0.566788361835478,-1.91253517929596,
12.8861696329972));
#13728=CARTESIAN_POINT('Ctrl Pts',(-0.56342532544817,-1.91352861547976,
12.8863937549288));
#13729=CARTESIAN_POINT('Ctrl Pts',(-0.554462542651234,-1.9161505316297,
12.8869892454798));
#13730=CARTESIAN_POINT('Ctrl Pts',(-0.548858193039458,-1.91776334750431,
12.8873597183418));
#13731=CARTESIAN_POINT('Ctrl Pts',(-0.509825454254745,-1.9288110415947,
12.8899274032023));
#13732=CARTESIAN_POINT('Ctrl Pts',(-0.476160281378337,-1.93739664735316,
12.892078062006));
#13733=CARTESIAN_POINT('Ctrl Pts',(-0.369545281309147,-1.96163925882593,
12.8987386913856));
#13734=CARTESIAN_POINT('Ctrl Pts',(-0.295928033976509,-1.97408731883704,
12.9031202238321));
#13735=CARTESIAN_POINT('Ctrl Pts',(-0.0926386958131628,-1.99683052226044,
12.9150309613857));
#13736=CARTESIAN_POINT('Ctrl Pts',(0.0375989808105898,-1.99862419921429,
12.922474052959));
#13737=CARTESIAN_POINT('Ctrl Pts',(0.208077979658812,-1.98429420822249,
12.93273237886));
#13738=CARTESIAN_POINT('Ctrl Pts',(0.248953392655578,-1.97958122397856,
12.935229170551));
#13739=CARTESIAN_POINT('Ctrl Pts',(0.306741935923933,-1.97110002409537,
12.9388282845268));
#13740=CARTESIAN_POINT('Ctrl Pts',(0.32379817334263,-1.96837004513549,12.9398991490418));
#13741=CARTESIAN_POINT('Ctrl Pts',(0.353736865043894,-1.96317848165001,
12.9417951230866));
#13742=CARTESIAN_POINT('Ctrl Pts',(0.366634661603345,-1.96081068243473,
12.9426172699228));
#13743=CARTESIAN_POINT('Ctrl Pts',(0.385655416590161,-1.95712459311536,
12.9438379867305));
#13744=CARTESIAN_POINT('Ctrl Pts',(0.391797196955183,-1.95590432494245,
12.944233433526));
#13745=CARTESIAN_POINT('Ctrl Pts',(0.40269990291107,-1.95368472766596,12.9449377343189));
#13746=CARTESIAN_POINT('Ctrl Pts',(0.407463131458751,-1.95269685889412,
12.9452462199318));
#13747=CARTESIAN_POINT('Ctrl Pts',(0.416739118091649,-1.95073764978661,
12.9458485245));
#13748=CARTESIAN_POINT('Ctrl Pts',(0.421252215197863,-1.94976804811328,
12.9461422859941));
#13749=CARTESIAN_POINT('Ctrl Pts',(0.433350350379864,-1.94712489838476,
12.9469317157075));
#13750=CARTESIAN_POINT('Ctrl Pts',(0.440928986778763,-1.94542271033173,
12.9474282997078));
#13751=CARTESIAN_POINT('Ctrl Pts',(0.468599873911747,-1.93903773727626,
12.949249082651));
#13752=CARTESIAN_POINT('Ctrl Pts',(0.488628518270105,-1.93408771940577,
12.9505818339787));
#13753=CARTESIAN_POINT('Ctrl Pts',(0.671050145446621,-1.88598841292785,
12.9628610526209));
#13754=CARTESIAN_POINT('Ctrl Pts',(0.827428707151443,-1.82279982009586,
12.974496735734));
#13755=CARTESIAN_POINT('Ctrl Pts',(1.03859223260738,-1.70464996305835,12.9913766088605));
#13756=CARTESIAN_POINT('Ctrl Pts',(1.10112362756031,-1.66494242939957,12.9965290735613));
#13757=CARTESIAN_POINT('Ctrl Pts',(1.19762375794861,-1.59584463406636,13.0045941421972));
#13758=CARTESIAN_POINT('Ctrl Pts',(1.2330609149702,-1.56862496142643,13.0075819884151));
#13759=CARTESIAN_POINT('Ctrl Pts',(1.27264266974691,-1.536050642658,13.0109227078983));
#13760=CARTESIAN_POINT('Ctrl Pts',(1.27770756447548,-1.53184017583816,13.0113502497672));
#13761=CARTESIAN_POINT('Ctrl Pts',(1.2853141451971,-1.52545282050443,13.0119923153173));
#13762=CARTESIAN_POINT('Ctrl Pts',(1.28787129740379,-1.52329454839005,13.0122081578691));
#13763=CARTESIAN_POINT('Ctrl Pts',(1.2924739137601,-1.51939000190424,13.0125966250882));
#13764=CARTESIAN_POINT('Ctrl Pts',(1.29452127535165,-1.51764602709827,13.0127694140074));
#13765=CARTESIAN_POINT('Ctrl Pts',(1.29896646940969,-1.51384400076335,13.013144544374));
#13766=CARTESIAN_POINT('Ctrl Pts',(1.30136293201885,-1.51178439825401,13.013346768207));
#13767=CARTESIAN_POINT('Ctrl Pts',(1.30795805801339,-1.50608901736665,13.0139032877959));
#13768=CARTESIAN_POINT('Ctrl Pts',(1.31214648636693,-1.50244134988453,13.0142567156789));
#13769=CARTESIAN_POINT('Ctrl Pts',(1.33324989760919,-1.48390700437273,13.0160377588024));
#13770=CARTESIAN_POINT('Ctrl Pts',(1.34992782386582,-1.46875125927684,13.0174462758331));
#13771=CARTESIAN_POINT('Ctrl Pts',(1.51160399704185,-1.31675010068925,13.0311525738477));
#13772=CARTESIAN_POINT('Ctrl Pts',(1.63558659584174,-1.15916296833073,13.0421826743286));
#13773=CARTESIAN_POINT('Ctrl Pts',(1.76057541025715,-0.939288047761927,
13.0571867551679));
#13774=CARTESIAN_POINT('Ctrl Pts',(1.7851229567189,-0.891752862080258,13.060402952193));
#13775=CARTESIAN_POINT('Ctrl Pts',(1.82107415985678,-0.814685723407736,
13.0656184057982));
#13776=CARTESIAN_POINT('Ctrl Pts',(1.83373701955855,-0.785768599972928,
13.0675754043001));
#13777=CARTESIAN_POINT('Ctrl Pts',(1.84904489286473,-0.748423646147957,
13.0701079363825));
#13778=CARTESIAN_POINT('Ctrl Pts',(1.85232789631094,-0.740260988095704,
13.0706617869076));
#13779=CARTESIAN_POINT('Ctrl Pts',(1.85752248557571,-0.727094537834776,
13.0715557500279));
#13780=CARTESIAN_POINT('Ctrl Pts',(1.85946812895349,-0.722104236147295,
13.0718947137212));
#13781=CARTESIAN_POINT('Ctrl Pts',(1.86313283254579,-0.712591759533854,
13.0725411306208));
#13782=CARTESIAN_POINT('Ctrl Pts',(1.86485558867669,-0.708071041753189,
13.072848457088));
#13783=CARTESIAN_POINT('Ctrl Pts',(1.86874507449941,-0.69775190812976,13.0735502712907));
#13784=CARTESIAN_POINT('Ctrl Pts',(1.87090128549016,-0.691949606032181,
13.0739451074359));
#13785=CARTESIAN_POINT('Ctrl Pts',(1.87740737433139,-0.67418916601277,13.0751543876654));
#13786=CARTESIAN_POINT('Ctrl Pts',(1.88166979833925,-0.662199545685784,
13.0759717305749));
#13787=CARTESIAN_POINT('Ctrl Pts',(1.93462754370278,-0.508595727634907,
13.0864573011627));
#13788=CARTESIAN_POINT('Ctrl Pts',(1.96733008104411,-0.362005440389104,
13.0966739134973));
#13789=CARTESIAN_POINT('Ctrl Pts',(1.99243399321145,-0.128438933471832,
13.1130339695099));
#13790=CARTESIAN_POINT('Ctrl Pts',(1.99610201943448,-0.0432103174738727,
13.1190074024435));
#13791=CARTESIAN_POINT('Ctrl Pts',(1.9934006718632,0.0850802574767662,13.1278259638173));
#13792=CARTESIAN_POINT('Ctrl Pts',(1.99109722319045,0.128129848801596,13.1307547908512));
#13793=CARTESIAN_POINT('Ctrl Pts',(1.98547219423881,0.193477003084971,13.1351234634735));
#13794=CARTESIAN_POINT('Ctrl Pts',(1.98316496548815,0.215847192835952,13.1366051061775));
#13795=CARTESIAN_POINT('Ctrl Pts',(1.97984207652003,0.243477810113742,13.1384140784597));
#13796=CARTESIAN_POINT('Ctrl Pts',(1.97918301485427,0.248778389909406,13.1387601430468));
#13797=CARTESIAN_POINT('Ctrl Pts',(1.97811043169272,0.257130638311162,13.1393038574043));
#13798=CARTESIAN_POINT('Ctrl Pts',(1.97771112694384,0.260184057559157,13.1395022938702));
#13799=CARTESIAN_POINT('Ctrl Pts',(1.97694865725338,0.265911358168978,13.1398738571327));
#13800=CARTESIAN_POINT('Ctrl Pts',(1.97658714172015,0.268585396321136,13.1400470719096));
#13801=CARTESIAN_POINT('Ctrl Pts',(1.97574988168768,0.274685145101786,13.1404415947336));
#13802=CARTESIAN_POINT('Ctrl Pts',(1.97527065421958,0.278110350309131,13.140662703405));
#13803=CARTESIAN_POINT('Ctrl Pts',(1.97377430711122,0.288606264528695,13.1413389839619));
#13804=CARTESIAN_POINT('Ctrl Pts',(1.97272809844936,0.295672867620914,13.1417925414698));
#13805=CARTESIAN_POINT('Ctrl Pts',(1.964083492199,0.351973432573512,13.1453931210843));
#13806=CARTESIAN_POINT('Ctrl Pts',(1.95468039609188,0.400917412061402,13.1484441468779));
#13807=CARTESIAN_POINT('Ctrl Pts',(1.93926858598507,0.467557326489517,13.1525523334263));
#13808=CARTESIAN_POINT('Ctrl Pts',(1.93483115752957,0.485593375777294,13.1536595073319));
#13809=CARTESIAN_POINT('Ctrl Pts',(1.89335903109508,0.644554129527794,13.1633962601067));
#13810=CARTESIAN_POINT('Ctrl Pts',(1.84123860629181,0.781090367770322,13.1716437892504));
#13811=CARTESIAN_POINT('Ctrl Pts',(1.74873821181218,0.961341575418219,13.1836318445919));
#13812=CARTESIAN_POINT('Ctrl Pts',(1.72061766441957,1.01081008227968,13.187044264059));
#13813=CARTESIAN_POINT('Ctrl Pts',(1.67290828311319,1.08696545973394,13.192549166655));
#13814=CARTESIAN_POINT('Ctrl Pts',(1.65470286124178,1.11448386144481,13.1945930931445));
#13815=CARTESIAN_POINT('Ctrl Pts',(1.63071184513949,1.14886302404906,13.1972231222505));
#13816=CARTESIAN_POINT('Ctrl Pts',(1.62555037681857,1.15615454769268,13.197785411657));
#13817=CARTESIAN_POINT('Ctrl Pts',(1.61719866423327,1.16778639120521,13.1986897412691));
#13818=CARTESIAN_POINT('Ctrl Pts',(1.61403947472152,1.17214894454351,13.1990305837515));
#13819=CARTESIAN_POINT('Ctrl Pts',(1.608012980178,1.18040042485246,13.1996784713379));
#13820=CARTESIAN_POINT('Ctrl Pts',(1.60514913448571,1.18429184021412,13.1999853806643));
#13821=CARTESIAN_POINT('Ctrl Pts',(1.59861612955871,1.19310170842326,13.2006833264761));
#13822=CARTESIAN_POINT('Ctrl Pts',(1.59493836968672,1.19801369434502,13.2010746972126));
#13823=CARTESIAN_POINT('Ctrl Pts',(1.58372779031625,1.21284333352319,13.2022630990607));
#13824=CARTESIAN_POINT('Ctrl Pts',(1.57612481340966,1.22270733470932,13.203062884784));
#13825=CARTESIAN_POINT('Ctrl Pts',(1.56033147370935,1.24280531712927,13.2047119638263));
#13826=CARTESIAN_POINT('Ctrl Pts',(1.5521316207831,1.25303103802927,13.2055616113609));
#13827=CARTESIAN_POINT('Ctrl Pts',(1.44996213316498,1.37790090780837,13.2160698435598));
#13828=CARTESIAN_POINT('Ctrl Pts',(1.34361496954079,1.48178394063907,13.2262569473503));
#13829=CARTESIAN_POINT('Ctrl Pts',(1.1574594013498,1.62697318623863,13.2427204541973));
#13830=CARTESIAN_POINT('Ctrl Pts',(1.08464744814017,1.67639352202142,13.2488716641467));
#13831=CARTESIAN_POINT('Ctrl Pts',(0.979941461428567,1.73777504832511,13.257146343355));
#13832=CARTESIAN_POINT('Ctrl Pts',(0.950649470120971,1.75397070834892,13.2594030327629));
#13833=CARTESIAN_POINT('Ctrl Pts',(0.904250294865482,1.77812089379548,13.2628727538733));
#13834=CARTESIAN_POINT('Ctrl Pts',(0.887415296080831,1.78658239798831,13.2641106634409));
#13835=CARTESIAN_POINT('Ctrl Pts',(0.865932525493793,1.79700132662705,13.2656615516521));
#13836=CARTESIAN_POINT('Ctrl Pts',(0.861394488730777,1.79918104779167,13.2659875519552));
#13837=CARTESIAN_POINT('Ctrl Pts',(0.854129078571266,1.80263699787101,13.2665068525781));
#13838=CARTESIAN_POINT('Ctrl Pts',(0.851407020973725,1.80392425392159,13.2667008267593));
#13839=CARTESIAN_POINT('Ctrl Pts',(0.846227197220622,1.80635944688689,13.2670688124267));
#13840=CARTESIAN_POINT('Ctrl Pts',(0.84377003472561,1.80750851982913,13.2672428909646));
#13841=CARTESIAN_POINT('Ctrl Pts',(0.838121183428136,1.8101361321636,13.2676419882736));
#13842=CARTESIAN_POINT('Ctrl Pts',(0.834927925133512,1.81161124289155,13.267866793755));
#13843=CARTESIAN_POINT('Ctrl Pts',(0.826396797936264,1.81552480931151,13.2684652928087));
#13844=CARTESIAN_POINT('Ctrl Pts',(0.821051992097934,1.81794819211223,13.2688380762222));
#13845=CARTESIAN_POINT('Ctrl Pts',(0.783334542785741,1.83484935122413,13.2714539631357));
#13846=CARTESIAN_POINT('Ctrl Pts',(0.750589195424921,1.84848624102692,13.2736485184695));
#13847=CARTESIAN_POINT('Ctrl Pts',(0.7072754536045,1.86518335845651,13.2764742729566));
#13848=CARTESIAN_POINT('Ctrl Pts',(0.69702318445152,1.86903884840689,13.2771375635024));
#13849=CARTESIAN_POINT('Ctrl Pts',(0.670810015722815,1.87865093964678,13.2788205837695));
#13850=CARTESIAN_POINT('Ctrl Pts',(0.654806281530004,1.88428877580716,13.2798360097516));
#13851=CARTESIAN_POINT('Ctrl Pts',(0.568108531090599,1.91359290048269,13.2852815374695));
#13852=CARTESIAN_POINT('Ctrl Pts',(0.496198715834034,1.93348726425133,13.289602664025));
#13853=CARTESIAN_POINT('Ctrl Pts',(0.368398015461284,1.96124235590159,13.2971874262387));
#13854=CARTESIAN_POINT('Ctrl Pts',(0.312975950731405,1.97084614455032,13.3004459759949));
#13855=CARTESIAN_POINT('Ctrl Pts',(0.157032436129244,1.99112439144268,13.309665945822));
#13856=CARTESIAN_POINT('Ctrl Pts',(0.0560098044528245,1.99652054836473,
13.3157054147493));
#13857=CARTESIAN_POINT('Ctrl Pts',(-0.0598190941009771,1.99390812031561,
13.3229219794116));
#13858=CARTESIAN_POINT('Ctrl Pts',(-0.0746551103487114,1.9934077635794,
13.3238515869151));
#13859=CARTESIAN_POINT('Ctrl Pts',(-0.0960672529864728,1.99244625372998,
13.3252013740779));
#13860=CARTESIAN_POINT('Ctrl Pts',(-0.102649086167767,1.99211800717658,
13.3256173913731));
#13861=CARTESIAN_POINT('Ctrl Pts',(-0.114117915505229,1.99148904997615,
13.3263442815541));
#13862=CARTESIAN_POINT('Ctrl Pts',(-0.119005682748961,1.9912029483676,13.3266546939597));
#13863=CARTESIAN_POINT('Ctrl Pts',(-0.128441960770964,1.99061573506232,
13.3272552051017));
#13864=CARTESIAN_POINT('Ctrl Pts',(-0.132990594538204,1.99031702076845,
13.3275452266908));
#13865=CARTESIAN_POINT('Ctrl Pts',(-0.144987077762068,1.98948788928263,
13.3283116039575));
#13866=CARTESIAN_POINT('Ctrl Pts',(-0.152432987274602,1.98893124471401,
13.3287887801909));
#13867=CARTESIAN_POINT('Ctrl Pts',(-0.178586625663199,1.98682831389388,
13.3304702536337));
#13868=CARTESIAN_POINT('Ctrl Pts',(-0.197275014016704,1.98505981283332,
13.3316814981852));
#13869=CARTESIAN_POINT('Ctrl Pts',(-0.422204760476087,1.96056684551021,
13.3463816197707));
#13870=CARTESIAN_POINT('Ctrl Pts',(-0.623673038696467,1.90606107047558,
13.3609840152083));
#13871=CARTESIAN_POINT('Ctrl Pts',(-0.864687321768802,1.79848295300659,
13.3792660631763));
#13872=CARTESIAN_POINT('Ctrl Pts',(-0.915324463526708,1.77324764414166,
13.3831441071015));
#13873=CARTESIAN_POINT('Ctrl Pts',(-0.988424635264389,1.73285065072883,
13.3887331243258));
#13874=CARTESIAN_POINT('Ctrl Pts',(-1.0117596025864,1.71933048663833,13.3905156379324));
#13875=CARTESIAN_POINT('Ctrl Pts',(-1.03964711410544,1.70240811575281,13.392637445272));
#13876=CARTESIAN_POINT('Ctrl Pts',(-1.04446719328993,1.69945514753302,13.393003866304));
#13877=CARTESIAN_POINT('Ctrl Pts',(-1.05195193000269,1.69482583433654,13.3935722869875));
#13878=CARTESIAN_POINT('Ctrl Pts',(-1.05462523394687,1.69316363297528,13.3937751951124));
#13879=CARTESIAN_POINT('Ctrl Pts',(-1.05957596719524,1.69006910221778,13.3941507371138));
#13880=CARTESIAN_POINT('Ctrl Pts',(-1.06185441208804,1.68863850726223,13.3943234791955));
#13881=CARTESIAN_POINT('Ctrl Pts',(-1.06697309923974,1.68541011823196,13.3947113567623));
#13882=CARTESIAN_POINT('Ctrl Pts',(-1.0698116870299,1.68360975758649,13.3949263190115));
#13883=CARTESIAN_POINT('Ctrl Pts',(-1.07705361076544,1.67899089185472,13.3954744262642));
#13884=CARTESIAN_POINT('Ctrl Pts',(-1.08145047555473,1.6761622134475,13.3958069071688));
#13885=CARTESIAN_POINT('Ctrl Pts',(-1.106579794563,1.65985547820696,13.397705730972));
#13886=CARTESIAN_POINT('Ctrl Pts',(-1.12707242421554,1.64600939750679,13.3992487275687));
#13887=CARTESIAN_POINT('Ctrl Pts',(-1.3150683005157,1.51383003712872,13.4134053495354));
#13888=CARTESIAN_POINT('Ctrl Pts',(-1.46366043151311,1.37069681692587,13.4247195065143));
#13889=CARTESIAN_POINT('Ctrl Pts',(-1.61694263365183,1.16911808737151,13.4398090495905));
#13890=CARTESIAN_POINT('Ctrl Pts',(-1.64465750403186,1.12979722331419,13.4427126003522));
#13891=CARTESIAN_POINT('Ctrl Pts',(-1.68688281901247,1.06503884003824,13.4474632483764));
#13892=CARTESIAN_POINT('Ctrl Pts',(-1.70230214304197,1.04021567511907,13.449277126273));
#13893=CARTESIAN_POINT('Ctrl Pts',(-1.72152701723658,1.00769320696023,13.4516485291823));
#13894=CARTESIAN_POINT('Ctrl Pts',(-1.72583638906771,1.00029476901316,13.4521876533559));
#13895=CARTESIAN_POINT('Ctrl Pts',(-1.73273778654472,0.988268917991104,
13.4530635315654));
#13896=CARTESIAN_POINT('Ctrl Pts',(-1.73535925271265,0.983658454101459,
13.453399219929));
#13897=CARTESIAN_POINT('Ctrl Pts',(-1.74034313959852,0.974811186966071,
13.4540432150859));
#13898=CARTESIAN_POINT('Ctrl Pts',(-1.74270855633166,0.97057610767373,13.4543514113084));
#13899=CARTESIAN_POINT('Ctrl Pts',(-1.74805622349338,0.960918984256324,
13.4550540300552));
#13900=CARTESIAN_POINT('Ctrl Pts',(-1.75102872749484,0.955491626786637,
13.4554487974626));
#13901=CARTESIAN_POINT('Ctrl Pts',(-1.76019467883963,0.938569519496435,
13.4566793741643));
#13902=CARTESIAN_POINT('Ctrl Pts',(-1.76630045118237,0.927027913828409,
13.457518283898));
#13903=CARTESIAN_POINT('Ctrl Pts',(-1.77788086488448,0.904607918294743,
13.4591474082248));
#13904=CARTESIAN_POINT('Ctrl Pts',(-1.78337007327317,0.893737672019076,
13.4599370634548));
#13905=CARTESIAN_POINT('Ctrl Pts',(-1.85354326899408,0.751553268442137,
13.4702641222799));
#13906=CARTESIAN_POINT('Ctrl Pts',(-1.90366933323944,0.613581557943482,
13.4803164337795));
#13907=CARTESIAN_POINT('Ctrl Pts',(-1.96803454245798,0.34893131267785,13.499307222851));
#13908=CARTESIAN_POINT('Ctrl Pts',(-1.98614827540819,0.223905700191042,
13.5081504270945));
#13909=CARTESIAN_POINT('Ctrl Pts',(-1.99288066089879,0.0870330352683144,
13.5172147805769));
#13910=CARTESIAN_POINT('Ctrl Pts',(-1.99332947349335,0.0760637918280366,
13.5179367987093));
#13911=CARTESIAN_POINT('Ctrl Pts',(-1.99395253407056,0.0569799569801758,
13.5191846199383));
#13912=CARTESIAN_POINT('Ctrl Pts',(-1.99416785586615,0.0488670821884949,
13.5197124786122));
#13913=CARTESIAN_POINT('Ctrl Pts',(-1.99440810164452,0.0371101366683036,
13.5204734340479));
#13914=CARTESIAN_POINT('Ctrl Pts',(-1.99447256002238,0.0334670880705113,
13.5207086697192));
#13915=CARTESIAN_POINT('Ctrl Pts',(-1.99456773343447,0.0271021835891608,
13.5211186621565));
#13916=CARTESIAN_POINT('Ctrl Pts',(-1.99460285953706,0.0243804164211393,
13.5212936647085));
#13917=CARTESIAN_POINT('Ctrl Pts',(-1.99466073433152,0.0190504664484458,
13.5216357345527));
#13918=CARTESIAN_POINT('Ctrl Pts',(-1.99468393878625,0.0164423202752563,
13.5218028275926));
#13919=CARTESIAN_POINT('Ctrl Pts',(-1.99473339151841,0.00931187168358707,
13.5222588583593));
#13920=CARTESIAN_POINT('Ctrl Pts',(-1.99474937675379,0.00478947843869328,
13.5225472241312));
#13921=CARTESIAN_POINT('Ctrl Pts',(-1.9947518565835,-0.0137361267942171,
13.5237250868335));
#13922=CARTESIAN_POINT('Ctrl Pts',(-1.99460627795939,-0.0277393759214068,
13.5246074513443));
#13923=CARTESIAN_POINT('Ctrl Pts',(-1.99241474297638,-0.132448655508878,
13.5311534944693));
#13924=CARTESIAN_POINT('Ctrl Pts',(-1.98432956355882,-0.2229339883265,13.5365216716757));
#13925=CARTESIAN_POINT('Ctrl Pts',(-1.95880170590122,-0.383837398866256,
13.5460309432565));
#13926=CARTESIAN_POINT('Ctrl Pts',(-1.94363461399264,-0.454444639112673,
13.5501909662735));
#13927=CARTESIAN_POINT('Ctrl Pts',(-1.89190391522397,-0.64442650627835,
13.5616588835142));
#13928=CARTESIAN_POINT('Ctrl Pts',(-1.84792265271898,-0.761420471277343,
13.569043723363));
#13929=CARTESIAN_POINT('Ctrl Pts',(-1.78761479390147,-0.885228866413328,
13.5776391827148));
#13930=CARTESIAN_POINT('Ctrl Pts',(-1.7818037667411,-0.89686795090905,13.578454990176));
#13931=CARTESIAN_POINT('Ctrl Pts',(-1.77303495227816,-0.914009644700568,
13.5796683731143));
#13932=CARTESIAN_POINT('Ctrl Pts',(-1.77016441296378,-0.919556698763571,
13.5800628839119));
#13933=CARTESIAN_POINT('Ctrl Pts',(-1.7650210609023,-0.929382423509603,
13.5807650484149));
#13934=CARTESIAN_POINT('Ctrl Pts',(-1.76275861241262,-0.933666486623504,
13.581072333889));
#13935=CARTESIAN_POINT('Ctrl Pts',(-1.75797591366456,-0.942643423616753,
13.5817186431198));
#13936=CARTESIAN_POINT('Ctrl Pts',(-1.75545243093064,-0.947334523251863,
13.5820577799426));
#13937=CARTESIAN_POINT('Ctrl Pts',(-1.74877426631718,-0.959630776713941,
13.5829504212264));
#13938=CARTESIAN_POINT('Ctrl Pts',(-1.74458879691419,-0.967218996866907,
13.5835050213464));
#13939=CARTESIAN_POINT('Ctrl Pts',(-1.72558086116508,-1.0011554253151,13.586002369479));
#13940=CARTESIAN_POINT('Ctrl Pts',(-1.71021068043326,-1.02719071048617,
13.5879647286637));
#13941=CARTESIAN_POINT('Ctrl Pts',(-1.66765998501485,-1.09566265393085,
13.593254408302));
#13942=CARTESIAN_POINT('Ctrl Pts',(-1.63945451104634,-1.13743336707393,
13.5966178070499));
#13943=CARTESIAN_POINT('Ctrl Pts',(-1.55059752970957,-1.25884448808484,
13.6068074846884));
#13944=CARTESIAN_POINT('Ctrl Pts',(-1.48550662201408,-1.33503142406606,
13.6137709875337));
#13945=CARTESIAN_POINT('Ctrl Pts',(-1.32818199005847,-1.49336030230474,
13.6293441809708));
#13946=CARTESIAN_POINT('Ctrl Pts',(-1.23346872288955,-1.57249952554449,
13.6379336920815));
#13947=CARTESIAN_POINT('Ctrl Pts',(-1.12583008634324,-1.64669100060092,
13.6464686967165));
#13948=CARTESIAN_POINT('Ctrl Pts',(-1.11958546388382,-1.65094307238791,
13.6469597321174));
#13949=CARTESIAN_POINT('Ctrl Pts',(-1.11041204924244,-1.65711342331361,
13.6476748841197));
#13950=CARTESIAN_POINT('Ctrl Pts',(-1.10750221803199,-1.65905956925683,
13.6479008283778));
#13951=CARTESIAN_POINT('Ctrl Pts',(-1.10233048015204,-1.66249884824038,
13.6483007840563));
#13952=CARTESIAN_POINT('Ctrl Pts',(-1.10007063819243,-1.6639950418226,13.648475000758));
#13953=CARTESIAN_POINT('Ctrl Pts',(-1.09528607635229,-1.66714879204547,
13.6488426906523));
#13954=CARTESIAN_POINT('Ctrl Pts',(-1.09276064635298,-1.66880521749823,
13.649036087936));
#13955=CARTESIAN_POINT('Ctrl Pts',(-1.08598144410121,-1.67322969790105,
13.6495534465257));
#13956=CARTESIAN_POINT('Ctrl Pts',(-1.0817208182994,-1.67598728858241,13.6498767132344));
#13957=CARTESIAN_POINT('Ctrl Pts',(-1.06121797543951,-1.6891465215322,13.651423535225));
#13958=CARTESIAN_POINT('Ctrl Pts',(-1.0448353165871,-1.69932892365676,13.6526331289959));
#13959=CARTESIAN_POINT('Ctrl Pts',(-0.998669783616965,-1.72710233649159,
13.6559762264157));
#13960=CARTESIAN_POINT('Ctrl Pts',(-0.968572184483595,-1.7441594062842,
13.6580810796015));
#13961=CARTESIAN_POINT('Ctrl Pts',(-0.857073414099578,-1.80357161420617,
13.6656660709162));
#13962=CARTESIAN_POINT('Ctrl Pts',(-0.773216541669191,-1.84108225219575,
13.6709707383685));
#13963=CARTESIAN_POINT('Ctrl Pts',(-0.540926825004352,-1.9263069878786,
13.6853210900567));
#13964=CARTESIAN_POINT('Ctrl Pts',(-0.389033638832481,-1.96262681157849,
13.6943910236463));
#13965=CARTESIAN_POINT('Ctrl Pts',(-0.22198425449101,-1.98239973600362,
13.7048953654109));
#13966=CARTESIAN_POINT('Ctrl Pts',(-0.209481802514728,-1.98375983561964,
13.7056843004836));
#13967=CARTESIAN_POINT('Ctrl Pts',(-0.190837058928924,-1.98560991446025,
13.7068652520011));
#13968=CARTESIAN_POINT('Ctrl Pts',(-0.184703839776413,-1.98618982115298,
13.7072544392017));
#13969=CARTESIAN_POINT('Ctrl Pts',(-0.173753088159362,-1.98717407349497,
13.7079506339012));
#13970=CARTESIAN_POINT('Ctrl Pts',(-0.168936565998396,-1.98758933635946,
13.7082572956933));
#13971=CARTESIAN_POINT('Ctrl Pts',(-0.158764366555967,-1.98842910403805,
13.7089059193552));
#13972=CARTESIAN_POINT('Ctrl Pts',(-0.153408396588484,-1.98884948872417,
13.709248008155));
#13973=CARTESIAN_POINT('Ctrl Pts',(-0.139204099398249,-1.98990665094881,
13.7101567850753));
#13974=CARTESIAN_POINT('Ctrl Pts',(-0.130353189343438,-1.99050604183705,
13.7107246418595));
#13975=CARTESIAN_POINT('Ctrl Pts',(-0.0892311574106101,-1.99301541238939,
13.7133705314204));
#13976=CARTESIAN_POINT('Ctrl Pts',(-0.056922212642224,-1.9941996618506,
13.7154711510732));
#13977=CARTESIAN_POINT('Ctrl Pts',(0.0306819320997055,-1.99528012266538,
13.7212297306897));
#13978=CARTESIAN_POINT('Ctrl Pts',(0.0859639078202527,-1.99366331705495,
13.7249321416479));
#13979=CARTESIAN_POINT('Ctrl Pts',(0.244771904188504,-1.98240144378039,
13.735757126845));
#13980=CARTESIAN_POINT('Ctrl Pts',(0.347700116554994,-1.9669596245787,13.743014511153));
#13981=CARTESIAN_POINT('Ctrl Pts',(0.518426938686605,-1.92752329500175,
13.7552335581274));
#13982=CARTESIAN_POINT('Ctrl Pts',(0.587000182459165,-1.90775903599471,
13.7601893322398));
#13983=CARTESIAN_POINT('Ctrl Pts',(0.662713030689064,-1.88146670996804,
13.7656255059346));
#13984=CARTESIAN_POINT('Ctrl Pts',(0.671035747824405,-1.87851445874288,
13.7662225510292));
#13985=CARTESIAN_POINT('Ctrl Pts',(0.71085800742426,-1.86409019765168,13.769075898882));
#13986=CARTESIAN_POINT('Ctrl Pts',(0.742086858824165,-1.85187979996067,
13.7713034109572));
#13987=CARTESIAN_POINT('Ctrl Pts',(0.77831348089238,-1.83665156452692,13.7738634727205));
#13988=CARTESIAN_POINT('Ctrl Pts',(0.783622080171581,-1.8343928917962,13.7742380080199));
#13989=CARTESIAN_POINT('Ctrl Pts',(0.792124647729441,-1.83073162212737,
13.7748368142688));
#13990=CARTESIAN_POINT('Ctrl Pts',(0.795324816879373,-1.82934364347109,
13.7750619464291));
#13991=CARTESIAN_POINT('Ctrl Pts',(0.801003431197971,-1.82686299487258,
13.7754609809476));
#13992=CARTESIAN_POINT('Ctrl Pts',(0.803483307726371,-1.82577366433469,
13.775635085254));
#13993=CARTESIAN_POINT('Ctrl Pts',(0.808729990388,-1.82345620411572,13.7760031014962));
#13994=CARTESIAN_POINT('Ctrl Pts',(0.811496214154684,-1.82222683011553,
13.7761969353473));
#13995=CARTESIAN_POINT('Ctrl Pts',(0.818920931295585,-1.81890685375166,
13.7767166973144));
#13996=CARTESIAN_POINT('Ctrl Pts',(0.823574253168949,-1.81680463595911,
13.777041919548));
#13997=CARTESIAN_POINT('Ctrl Pts',(0.846081381207996,-1.80653241389346,
13.7786126202225));
#13998=CARTESIAN_POINT('Ctrl Pts',(0.863822733397944,-1.79811663187595,
13.7798436106925));
#13999=CARTESIAN_POINT('Ctrl Pts',(0.913256145319009,-1.77376684802055,
13.7832614458629));
#14000=CARTESIAN_POINT('Ctrl Pts',(0.944652895926133,-1.75724694852104,
13.7854180641716));
#14001=CARTESIAN_POINT('Ctrl Pts',(1.0588760128137,-1.6931998345439,13.7932720581506));
#14002=CARTESIAN_POINT('Ctrl Pts',(1.1387030602224,-1.64057973191981,13.7987816775673));
#14003=CARTESIAN_POINT('Ctrl Pts',(1.21823562510925,-1.57954176858851,13.8045975176185));
#14004=CARTESIAN_POINT('Ctrl Pts',(1.22200275413431,-1.57662915924049,13.8048737913468));
#14005=CARTESIAN_POINT('Ctrl Pts',(1.34054237754247,-1.48429849005539,13.81359359804));
#14006=CARTESIAN_POINT('Ctrl Pts',(1.44518155266242,-1.3826198123348,13.8221163291868));
#14007=CARTESIAN_POINT('Ctrl Pts',(1.54598727698084,-1.26060103973144,13.8319971454823));
#14008=CARTESIAN_POINT('Ctrl Pts',(1.55405021421574,-1.25064765680068,13.8328005582588));
#14009=CARTESIAN_POINT('Ctrl Pts',(1.56587678229632,-1.23575725294827,13.8339989931224));
#14010=CARTESIAN_POINT('Ctrl Pts',(1.56971424079087,-1.23087907058031,13.8343910602453));
#14011=CARTESIAN_POINT('Ctrl Pts',(1.5765034552398,-1.22216522723103,13.8350904754685));
#14012=CARTESIAN_POINT('Ctrl Pts',(1.57946414870929,-1.21833656651237,13.8353974656866));
#14013=CARTESIAN_POINT('Ctrl Pts',(1.58566649092188,-1.21025531799901,13.8360447937092));
#14014=CARTESIAN_POINT('Ctrl Pts',(1.58890502796241,-1.20600040065295,13.8363852508279));
#14015=CARTESIAN_POINT('Ctrl Pts',(1.59740249985309,-1.19474244704764,13.8372851089981));
#14016=CARTESIAN_POINT('Ctrl Pts',(1.60263244524425,-1.18771777064549,13.8378456381307));
#14017=CARTESIAN_POINT('Ctrl Pts',(1.62625411533122,-1.15554989028574,13.8404083171236));
#14018=CARTESIAN_POINT('Ctrl Pts',(1.6441006921545,-1.1300135964279,13.8424313591748));
#14019=CARTESIAN_POINT('Ctrl Pts',(1.69040731019591,-1.06033411940189,13.8479251632032));
#14020=CARTESIAN_POINT('Ctrl Pts',(1.7177325813566,-1.01546998495897,13.8514355260991));
#14021=CARTESIAN_POINT('Ctrl Pts',(1.79271940753026,-0.880648034672342,
13.8619020718953));
#14022=CARTESIAN_POINT('Ctrl Pts',(1.83530232144922,-0.788064673361517,
13.8689946708152));
#14023=CARTESIAN_POINT('Ctrl Pts',(1.9116315202932,-0.581921974203907,13.884330097668));
#14024=CARTESIAN_POINT('Ctrl Pts',(1.94272336619323,-0.467761892707373,
13.8925466142314));
#14025=CARTESIAN_POINT('Ctrl Pts',(1.96488315905716,-0.343977164830148,
13.9007580609771));
#14026=CARTESIAN_POINT('Ctrl Pts',(1.96618828157022,-0.336436865826537,
13.9012555005137));
#14027=CARTESIAN_POINT('Ctrl Pts',(1.96803020612822,-0.3254182746908,13.9019781998201));
#14028=CARTESIAN_POINT('Ctrl Pts',(1.96860122662795,-0.321945890983775,
13.9022053416384));
#14029=CARTESIAN_POINT('Ctrl Pts',(1.96959616892833,-0.315794004044673,
13.9026066606355));
#14030=CARTESIAN_POINT('Ctrl Pts',(1.97002381686889,-0.313115127344135,
13.9027810480091));
#14031=CARTESIAN_POINT('Ctrl Pts',(1.97091447964498,-0.307461766781899,
13.9031482797371));
#14032=CARTESIAN_POINT('Ctrl Pts',(1.97137622556085,-0.3044871125265,13.9033410513282));
#14033=CARTESIAN_POINT('Ctrl Pts',(1.97259164080799,-0.296538511739521,
13.9038549668516));
#14034=CARTESIAN_POINT('Ctrl Pts',(1.97333323695362,-0.291562699246015,
13.904175432223));
#14035=CARTESIAN_POINT('Ctrl Pts',(1.97675713439055,-0.267978117832872,
13.9056887214018));
#14036=CARTESIAN_POINT('Ctrl Pts',(1.9791951938879,-0.249334086534074,13.9068683054678));
#14037=CARTESIAN_POINT('Ctrl Pts',(1.98522763885092,-0.197514836733235,
13.9101075476434));
#14038=CARTESIAN_POINT('Ctrl Pts',(1.98825394017183,-0.164278499112953,
13.9121406680116));
#14039=CARTESIAN_POINT('Ctrl Pts',(1.99619160483572,-0.0436532919129626,
13.9194087086716));
#14040=CARTESIAN_POINT('Ctrl Pts',(1.99618533483194,0.043963104206752,13.9244809522692));
#14041=CARTESIAN_POINT('Ctrl Pts',(1.98063159133876,0.279746294262301,13.9381854976157));
#14042=CARTESIAN_POINT('Ctrl Pts',(1.95426623850361,0.4266096851535,13.9468162839343));
#14043=CARTESIAN_POINT('Ctrl Pts',(1.90756626232315,0.583473421016851,13.9569409452345));
#14044=CARTESIAN_POINT('Ctrl Pts',(1.90314774562963,0.597728130332748,13.9578690641864));
#14045=CARTESIAN_POINT('Ctrl Pts',(1.89544359618929,0.621630907615951,13.9594396531293));
#14046=CARTESIAN_POINT('Ctrl Pts',(1.89224316941717,0.631305942690054,13.9600793464363));
#14047=CARTESIAN_POINT('Ctrl Pts',(1.88697072846152,0.646844416737335,13.9611133090565));
#14048=CARTESIAN_POINT('Ctrl Pts',(1.88494515609302,0.652723514693834,13.9615060443685));
#14049=CARTESIAN_POINT('Ctrl Pts',(1.8812891406975,0.663175922719456,13.9622070512015));
#14050=CARTESIAN_POINT('Ctrl Pts',(1.87966942028213,0.667752952187103,13.9625149649794));
#14051=CARTESIAN_POINT('Ctrl Pts',(1.87625048449666,0.677303220194546,13.9631594514686));
#14052=CARTESIAN_POINT('Ctrl Pts',(1.87444817059189,0.682275301866131,13.963496125358));
#14053=CARTESIAN_POINT('Ctrl Pts',(1.8696995001406,0.695214715739058,13.9643752960744));
#14054=CARTESIAN_POINT('Ctrl Pts',(1.86672200931945,0.703170433128824,13.9649188290253));
#14055=CARTESIAN_POINT('Ctrl Pts',(1.85350437410389,0.737811679144055,13.9672987406728));
#14056=CARTESIAN_POINT('Ctrl Pts',(1.84274258265454,0.764293249764667,13.9691525367127));
#14057=CARTESIAN_POINT('Ctrl Pts',(1.81291974310069,0.833383345159686,13.9740833975887));
#14058=CARTESIAN_POINT('Ctrl Pts',(1.79292668649248,0.87556788092392,13.9771907967008));
#14059=CARTESIAN_POINT('Ctrl Pts',(1.68296810186906,1.08798519929659,13.9933389278402));
#14060=CARTESIAN_POINT('Ctrl Pts',(1.5701948284717,1.24521702220936,14.0071145680869));
#14061=CARTESIAN_POINT('Ctrl Pts',(1.41027053067053,1.41124472081864,14.0227049741085));
#14062=CARTESIAN_POINT('Ctrl Pts',(1.38309971724818,1.43788395560388,14.0252402074162));
#14063=CARTESIAN_POINT('Ctrl Pts',(1.35035870687126,1.46819689488969,14.0281483765619));
#14064=CARTESIAN_POINT('Ctrl Pts',(1.3455137860071,1.47263824953324,14.0285750805002));
#14065=CARTESIAN_POINT('Ctrl Pts',(1.33813866080774,1.47933226872889,14.0292190152375));
#14066=CARTESIAN_POINT('Ctrl Pts',(1.33562458356043,1.48160251385363,14.0294375446393));
#14067=CARTESIAN_POINT('Ctrl Pts',(1.33110208309596,1.48566552574412,14.02982887802));
#14068=CARTESIAN_POINT('Ctrl Pts',(1.3290958120192,1.48746063234251,14.030001857629));
#14069=CARTESIAN_POINT('Ctrl Pts',(1.32475040087298,1.49133286812748,14.0303751681932));
#14070=CARTESIAN_POINT('Ctrl Pts',(1.32241001548226,1.49340855074957,14.0305753906491));
#14071=CARTESIAN_POINT('Ctrl Pts',(1.31589437113479,1.49915993465938,14.0311305195149));
#14072=CARTESIAN_POINT('Ctrl Pts',(1.31170856481017,1.50282372501202,14.0314845450913));
#14073=CARTESIAN_POINT('Ctrl Pts',(1.2881920714096,1.5232343469081,14.0334593624688));
#14074=CARTESIAN_POINT('Ctrl Pts',(1.26855496702423,1.53962662174213,14.0350551617011));
#14075=CARTESIAN_POINT('Ctrl Pts',(1.12039736330129,1.65854288372357,14.0467527892344));
#14076=CARTESIAN_POINT('Ctrl Pts',(0.979942041663491,1.74521719071281,14.0560101728908));
#14077=CARTESIAN_POINT('Ctrl Pts',(0.730475920874315,1.85943988592107,14.072061721505));
#14078=CARTESIAN_POINT('Ctrl Pts',(0.626929162196461,1.89685699182623,14.0786182510588));
#14079=CARTESIAN_POINT('Ctrl Pts',(0.508370114521299,1.92892565464097,14.0862848138036));
#14080=CARTESIAN_POINT('Ctrl Pts',(0.495871109096363,1.93217654088341,14.0870947723244));
#14081=CARTESIAN_POINT('Ctrl Pts',(0.477299835351369,1.93681470720925,14.0883011036752));
#14082=CARTESIAN_POINT('Ctrl Pts',(0.47125104699431,1.93829533151338,14.0886944638391));
#14083=CARTESIAN_POINT('Ctrl Pts',(0.460486545571937,1.94087690316734,14.0893953319801));
#14084=CARTESIAN_POINT('Ctrl Pts',(0.455773549061324,1.94198905331613,14.0897024766012));
#14085=CARTESIAN_POINT('Ctrl Pts',(0.451048087361994,1.94308599538547,14.0900107288729));
#14086=CARTESIAN_POINT('Ctrl Pts',(0.451039591272035,1.94308796756123,14.0900112830925));
#14087=CARTESIAN_POINT('Ctrl Pts',(0.451022618687848,1.94309190724672,14.0900123902554));
#14088=CARTESIAN_POINT('Ctrl Pts',(0.451014142110932,1.94309387477591,14.090012943204));
#14089=CARTESIAN_POINT('Ctrl Pts',(0.450997208663554,1.94309780514339,14.0900140478177));
#14090=CARTESIAN_POINT('Ctrl Pts',(0.45098875162203,1.94309976802165,14.0900145994938));
#14091=CARTESIAN_POINT('Ctrl Pts',(0.450971856898543,1.94310368916857,14.0900157015852));
#14092=CARTESIAN_POINT('Ctrl Pts',(0.450963419250079,1.94310564742973,14.0900162519982));
#14093=CARTESIAN_POINT('Ctrl Pts',(0.450946563230409,1.94310955936236,14.0900173515686));
#14094=CARTESIAN_POINT('Ctrl Pts',(0.450938144895026,1.94311151302578,14.0900179007237));
#14095=CARTESIAN_POINT('Ctrl Pts',(0.450921327437817,1.9431154157785,14.0900189977823));
#14096=CARTESIAN_POINT('Ctrl Pts',(0.450912928337988,1.94311736486297,14.0900195456844));
#14097=CARTESIAN_POINT('Ctrl Pts',(0.450896149287829,1.94312125847344,14.0900206402413));
#14098=CARTESIAN_POINT('Ctrl Pts',(0.450887769335964,1.94312320300007,14.0900211868962));
#14099=CARTESIAN_POINT('Ctrl Pts',(0.450871028619272,1.94312708748694,14.0900222789561));
#14100=CARTESIAN_POINT('Ctrl Pts',(0.450862667788463,1.94312902746275,14.0900228243655));
#14101=CARTESIAN_POINT('Ctrl Pts',(0.450845965149942,1.94313290288682,14.0900239139452));
#14102=CARTESIAN_POINT('Ctrl Pts',(0.450837623352016,1.94313483833306,14.0900244581149));
#14103=CARTESIAN_POINT('Ctrl Pts',(0.445712436350852,1.94432393855725,14.0903587956287));
#14104=CARTESIAN_POINT('Ctrl Pts',(0.44059096277679,1.94549087805976,14.090693237635));
#14105=CARTESIAN_POINT('Ctrl Pts',(0.427247453436127,1.9484758358801,14.0915655262044));
#14106=CARTESIAN_POINT('Ctrl Pts',(0.419018475824329,1.95026202926371,14.0921043884722));
#14107=CARTESIAN_POINT('Ctrl Pts',(0.4009526909984,1.9540637975691,14.093289505301));
#14108=CARTESIAN_POINT('Ctrl Pts',(0.391111523534666,1.9560572986011,14.0939364510269));
#14109=CARTESIAN_POINT('Ctrl Pts',(0.362157647324509,1.96169517831095,14.095844017298));
#14110=CARTESIAN_POINT('Ctrl Pts',(0.34300661950407,1.96513423172292,14.0971110843593));
#14111=CARTESIAN_POINT('Ctrl Pts',(0.275847153198609,1.97618280946162,14.1015741010343));
#14112=CARTESIAN_POINT('Ctrl Pts',(0.227616654485031,1.98231686626571,14.1048146659128));
#14113=CARTESIAN_POINT('Ctrl Pts',(0.0600476630782478,1.99743282104281,
14.1161925064959));
#14114=CARTESIAN_POINT('Ctrl Pts',(-0.05983373020311,1.99743790249784,14.1245580774018));
#14115=CARTESIAN_POINT('Ctrl Pts',(-0.246995628927533,1.98057683442121,
14.1376545033346));
#14116=CARTESIAN_POINT('Ctrl Pts',(-0.31465766922163,1.97095996034574,14.1423914355414));
#14117=CARTESIAN_POINT('Ctrl Pts',(-0.420250004285369,1.95037441021363,
14.1496745242331));
#14118=CARTESIAN_POINT('Ctrl Pts',(-0.458576121107775,1.94172059170124,
14.1522944264559));
#14119=CARTESIAN_POINT('Ctrl Pts',(-0.503052720171037,1.93028743298646,
14.1552879441627));
#14120=CARTESIAN_POINT('Ctrl Pts',(-0.509472628877797,1.92860292871875,
14.1557188841443));
#14121=CARTESIAN_POINT('Ctrl Pts',(-0.519169733065526,1.92600672891297,
14.1563679340139));
#14122=CARTESIAN_POINT('Ctrl Pts',(-0.522453121330005,1.92511866335154,
14.1565873730946));
#14123=CARTESIAN_POINT('Ctrl Pts',(-0.528332219504052,1.92351238145379,
14.1569796874041));
#14124=CARTESIAN_POINT('Ctrl Pts',(-0.530928750029529,1.92279730560957,
14.1571527421038));
#14125=CARTESIAN_POINT('Ctrl Pts',(-0.53652835559629,1.9212429852997,14.1575254849396));
#14126=CARTESIAN_POINT('Ctrl Pts',(-0.5395309027404,1.92040196058962,14.1577250675247));
#14127=CARTESIAN_POINT('Ctrl Pts',(-0.547840098401107,1.91805349810208,
14.1582766315778));
#14128=CARTESIAN_POINT('Ctrl Pts',(-0.553142535064395,1.91653106748637,
14.1586277506138));
#14129=CARTESIAN_POINT('Ctrl Pts',(-0.582338975191743,1.90801695011468,
14.1605567148997));
#14130=CARTESIAN_POINT('Ctrl Pts',(-0.606108063188161,1.90060004179537,
14.1621109123188));
#14131=CARTESIAN_POINT('Ctrl Pts',(-0.677268036377954,1.87692440877626,
14.1667323226522));
#14132=CARTESIAN_POINT('Ctrl Pts',(-0.724193761676973,1.85932282933657,
14.1697373885421));
#14133=CARTESIAN_POINT('Ctrl Pts',(-0.904492790581082,1.78383024896867,
14.1812948314115));
#14134=CARTESIAN_POINT('Ctrl Pts',(-1.03203783113073,1.71320114618023,14.1895273311107));
#14135=CARTESIAN_POINT('Ctrl Pts',(-1.17434099269437,1.6126943095871,14.1998544280922));
#14136=CARTESIAN_POINT('Ctrl Pts',(-1.19753894490107,1.59554381993037,14.2015768445579));
#14137=CARTESIAN_POINT('Ctrl Pts',(-1.26286629641932,1.54501919947881,14.2065540833302));
#14138=CARTESIAN_POINT('Ctrl Pts',(-1.30402707849208,1.51043973353006,14.2098469913305));
#14139=CARTESIAN_POINT('Ctrl Pts',(-1.35107059390338,1.46756063510306,14.2138292785904));
#14140=CARTESIAN_POINT('Ctrl Pts',(-1.35835197126327,1.46082370048428,14.214452149388));
#14141=CARTESIAN_POINT('Ctrl Pts',(-1.3701049018581,1.44978571134198,14.2154683235296));
#14142=CARTESIAN_POINT('Ctrl Pts',(-1.37460723140893,1.44551755743488,14.2158602162599));
#14143=CARTESIAN_POINT('Ctrl Pts',(-1.38258616241949,1.43788264027959,14.2165594358498));
#14144=CARTESIAN_POINT('Ctrl Pts',(-1.38607057537324,1.43452408245359,14.2168664055652));
#14145=CARTESIAN_POINT('Ctrl Pts',(-1.39277871695146,1.42801097739425,14.2174605375819));
#14146=CARTESIAN_POINT('Ctrl Pts',(-1.39600403929216,1.42485810791133,14.2177476254877));
#14147=CARTESIAN_POINT('Ctrl Pts',(-1.40295859262847,1.4180134999054,14.2183697634872));
#14148=CARTESIAN_POINT('Ctrl Pts',(-1.40668399721728,1.41431793796357,14.218704981133));
#14149=CARTESIAN_POINT('Ctrl Pts',(-1.42121147691924,1.39979265190426,14.2200198984145));
#14150=CARTESIAN_POINT('Ctrl Pts',(-1.43190319211175,1.38885375658874,14.2210044416164));
#14151=CARTESIAN_POINT('Ctrl Pts',(-1.48996490074829,1.32806659090648,14.2264456742866));
#14152=CARTESIAN_POINT('Ctrl Pts',(-1.53485355648307,1.27592278644834,14.2310070410109));
#14153=CARTESIAN_POINT('Ctrl Pts',(-1.61307833441772,1.17494042229399,14.2396547067972));
#14154=CARTESIAN_POINT('Ctrl Pts',(-1.64711153839,1.12673397856859,14.2437116930747));
#14155=CARTESIAN_POINT('Ctrl Pts',(-1.76304350119893,0.946020985530517,
14.2586084017862));
#14156=CARTESIAN_POINT('Ctrl Pts',(-1.83149559110271,0.805547899966137,
14.2696511925881));
#14157=CARTESIAN_POINT('Ctrl Pts',(-1.88758510298821,0.645174720774092,
14.2808593455718));
#14158=CARTESIAN_POINT('Ctrl Pts',(-1.8921161350605,0.631763009804888,14.2817861563105));
#14159=CARTESIAN_POINT('Ctrl Pts',(-1.89796473959787,0.613823764000471,
14.2830108333472));
#14160=CARTESIAN_POINT('Ctrl Pts',(-1.89940945525219,0.60933856632469,14.2833157857629));
#14161=CARTESIAN_POINT('Ctrl Pts',(-1.90164065600232,0.602326639120403,
14.2837905472326));
#14162=CARTESIAN_POINT('Ctrl Pts',(-1.90243801746204,0.599803430025924,
14.2839609874213));
#14163=CARTESIAN_POINT('Ctrl Pts',(-1.90395991547368,0.594953896847176,
14.2842877895007));
#14164=CARTESIAN_POINT('Ctrl Pts',(-1.90468520225311,0.592627859197365,
14.2844441923629));
#14165=CARTESIAN_POINT('Ctrl Pts',(-1.90641061662941,0.587058466087206,
14.2848178608698));
#14166=CARTESIAN_POINT('Ctrl Pts',(-1.90740672910799,0.583813884704258,
14.2850348889252));
#14167=CARTESIAN_POINT('Ctrl Pts',(-1.91037970765942,0.574041337216675,
14.2856866241069));
#14168=CARTESIAN_POINT('Ctrl Pts',(-1.91233140354439,0.567505674450074,
14.2861198829101));
#14169=CARTESIAN_POINT('Ctrl Pts',(-1.93061598164805,0.505110414873003,
14.2902324828119));
#14170=CARTESIAN_POINT('Ctrl Pts',(-1.9445321990242,0.448565048757741,14.2937791938054));
#14171=CARTESIAN_POINT('Ctrl Pts',(-1.98164655554369,0.263133038175746,
14.3050692892849));
#14172=CARTESIAN_POINT('Ctrl Pts',(-1.9946405641782,0.132561637484325,14.3125121367147));
#14173=CARTESIAN_POINT('Ctrl Pts',(-1.99474931168446,0.00165711628034759,
14.3201739592359));
#14174=CARTESIAN_POINT('',(-1.994663636046,-0.00099025261153359,15.1209549068572));
#14175=CARTESIAN_POINT('Ctrl Pts',(-1.99474927319053,0.00170282290857632,
14.3209548813952));
#14176=CARTESIAN_POINT('Ctrl Pts',(-1.99480844880348,-0.0676176626926073,
14.3253702812332));
#14177=CARTESIAN_POINT('Ctrl Pts',(-1.99124984682737,-0.137000164295673,
14.3297856810711));
#14178=CARTESIAN_POINT('Ctrl Pts',(-1.98408075767403,-0.206036670346913,
14.3342010809091));
#14179=CARTESIAN_POINT('Ctrl Pts',(-1.97691422051932,-0.275048601300166,
14.3386149089861));
#14180=CARTESIAN_POINT('Ctrl Pts',(-1.96613979730227,-0.34371428884389,
14.3430287370631));
#14181=CARTESIAN_POINT('Ctrl Pts',(-1.95181673263811,-0.411629693649408,
14.3474425651401));
#14182=CARTESIAN_POINT('Ctrl Pts',(-1.93749376889503,-0.479544619919332,
14.3518563621171));
#14183=CARTESIAN_POINT('Ctrl Pts',(-1.91962231764192,-0.546708789784324,
14.356270159094));
#14184=CARTESIAN_POINT('Ctrl Pts',(-1.89831258304288,-0.61272905885152,
14.360683956071));
#14185=CARTESIAN_POINT('Ctrl Pts',(-1.876980577809,-0.678818325178993,14.3651023658722));
#14186=CARTESIAN_POINT('Ctrl Pts',(-1.85220326800389,-0.74376083169,14.3695207756734));
#14187=CARTESIAN_POINT('Ctrl Pts',(-1.82414023188162,-0.807180262971581,
14.3739391854746));
#14188=CARTESIAN_POINT('Ctrl Pts',(-1.79606178800796,-0.870634514107515,
14.378360021163));
#14189=CARTESIAN_POINT('Ctrl Pts',(-1.76469425181013,-0.932563583840136,
14.3827808568514));
#14190=CARTESIAN_POINT('Ctrl Pts',(-1.73024341602082,-0.99261537556931,
14.3872016925398));
#14191=CARTESIAN_POINT('Ctrl Pts',(-1.69572952893114,-1.05277707300822,
14.3916306191622));
#14192=CARTESIAN_POINT('Ctrl Pts',(-1.65812134455463,-1.11105421647625,
14.3960595457846));
#14193=CARTESIAN_POINT('Ctrl Pts',(-1.61766783441448,-1.16712396085453,
14.400488472407));
#14194=CARTESIAN_POINT('Ctrl Pts',(-1.59009756172142,-1.20533716255158,
14.4035069178842));
#14195=CARTESIAN_POINT('Ctrl Pts',(-1.56120656146211,-1.24252572116292,
14.4065253633613));
#14196=CARTESIAN_POINT('Ctrl Pts',(-1.53108363525599,-1.27859706880287,
14.4095438088384));
#14197=CARTESIAN_POINT('Ctrl Pts',(-1.48663404004653,-1.33182419522096,
14.4139978475564));
#14198=CARTESIAN_POINT('Ctrl Pts',(-1.43931749796301,-1.38283607938058,
14.4184518862744));
#14199=CARTESIAN_POINT('Ctrl Pts',(-1.38938328998155,-1.43130766644354,
14.4229059249924));
#14200=CARTESIAN_POINT('Ctrl Pts',(-1.33952414087314,-1.47970639317994,
14.4273532685981));
#14201=CARTESIAN_POINT('Ctrl Pts',(-1.28705548380105,-1.52557206330759,
14.4318006122039));
#14202=CARTESIAN_POINT('Ctrl Pts',(-1.23226639428315,-1.56861311228116,
14.4362479558096));
#14203=CARTESIAN_POINT('Ctrl Pts',(-1.17754189546993,-1.61160342028226,
14.4406900564544));
#14204=CARTESIAN_POINT('Ctrl Pts',(-1.12050278047846,-1.65177541983638,
14.4451321570992));
#14205=CARTESIAN_POINT('Ctrl Pts',(-1.06147313750855,-1.68887605846248,
14.449574257744));
#14206=CARTESIAN_POINT('Ctrl Pts',(-1.0024807306989,-1.72595329384139,14.454013556292));
#14207=CARTESIAN_POINT('Ctrl Pts',(-0.941500700329472,-1.75996275179668,
14.4584528548401));
#14208=CARTESIAN_POINT('Ctrl Pts',(-0.878886965382996,-1.79069407341954,
14.4628921533881));
#14209=CARTESIAN_POINT('Ctrl Pts',(-0.816291451161476,-1.82141645216494,
14.4673301600911));
#14210=CARTESIAN_POINT('Ctrl Pts',(-0.752063615385313,-1.84886237271784,
14.4717681667942));
#14211=CARTESIAN_POINT('Ctrl Pts',(-0.686581302364516,-1.87286776835511,
14.4762061734973));
#14212=CARTESIAN_POINT('Ctrl Pts',(-0.621095794433747,-1.89687433522587,
14.4806443967326));
#14213=CARTESIAN_POINT('Ctrl Pts',(-0.554356148211634,-1.91743987764979,
14.4850826199679));
#14214=CARTESIAN_POINT('Ctrl Pts',(-0.486757792449514,-1.93444938263829,
14.4895208432032));
#14215=CARTESIAN_POINT('Ctrl Pts',(-0.419087823689509,-1.95147690732019,
14.4939637682462));
#14216=CARTESIAN_POINT('Ctrl Pts',(-0.350557805364128,-1.96494075565657,
14.4984066932892));
#14217=CARTESIAN_POINT('Ctrl Pts',(-0.281574914249643,-1.97477672919379,
14.5028496183323));
#14218=CARTESIAN_POINT('Ctrl Pts',(-0.212551754982117,-1.98461844439362,
14.5072951368935));
#14219=CARTESIAN_POINT('Ctrl Pts',(-0.143075684511765,-1.99082802607985,
14.5117406554548));
#14220=CARTESIAN_POINT('Ctrl Pts',(-0.0735577887056503,-1.99339329140557,
14.5161861740161));
#14221=CARTESIAN_POINT('Ctrl Pts',(-0.00391858223084199,-1.99596303319089,
14.5206394501313));
#14222=CARTESIAN_POINT('Ctrl Pts',(0.0657621058233227,-1.9948757716827,
14.5250927262465));
#14223=CARTESIAN_POINT('Ctrl Pts',(0.135075203542659,-1.99017141268985,
14.5295460023618));
#14224=CARTESIAN_POINT('Ctrl Pts',(0.172190374149558,-1.98765236373141,
14.5319306036596));
#14225=CARTESIAN_POINT('Ctrl Pts',(0.209200261547404,-1.98409707230917,
14.5343152049574));
#14226=CARTESIAN_POINT('Ctrl Pts',(0.246043286472205,-1.97951768460955,
14.5366998062552));
#14227=CARTESIAN_POINT('Ctrl Pts',(0.314859930853649,-1.9709641498373,14.5411538449732));
#14228=CARTESIAN_POINT('Ctrl Pts',(0.383366292641739,-1.95880084951107,
14.5456078836912));
#14229=CARTESIAN_POINT('Ctrl Pts',(0.451154115862295,-1.94306137994674,
14.5500619224091));
#14230=CARTESIAN_POINT('Ctrl Pts',(0.518840043452057,-1.92734556925067,
14.5545092660149));
#14231=CARTESIAN_POINT('Ctrl Pts',(0.585809103166717,-1.90806436824703,
14.5589566096206));
#14232=CARTESIAN_POINT('Ctrl Pts',(0.651659651011456,-1.88530296285335,
14.5634039532264));
#14233=CARTESIAN_POINT('Ctrl Pts',(0.717432567829195,-1.86256839081694,
14.5678460538712));
#14234=CARTESIAN_POINT('Ctrl Pts',(0.78208913123683,-1.8363619222356,14.572288154516));
#14235=CARTESIAN_POINT('Ctrl Pts',(0.84524112026654,-1.80681903109043,14.5767302551608));
#14236=CARTESIAN_POINT('Ctrl Pts',(0.908353272741763,-1.77729477573189,
14.5811695537088));
#14237=CARTESIAN_POINT('Ctrl Pts',(0.969962291210684,-1.74443847987309,
14.5856088522568));
#14238=CARTESIAN_POINT('Ctrl Pts',(1.02969969890823,-1.70843381275609,14.5900481508048));
#14239=CARTESIAN_POINT('Ctrl Pts',(1.08941972289794,-1.67243962307086,14.5944861575079));
#14240=CARTESIAN_POINT('Ctrl Pts',(1.14726879824033,-1.63329913347875,14.598924164211));
#14241=CARTESIAN_POINT('Ctrl Pts',(1.20290441521812,-1.59124119175842,14.603362170914));
#14242=CARTESIAN_POINT('Ctrl Pts',(1.25854274668131,-1.54918119801323,14.6078003941493));
#14243=CARTESIAN_POINT('Ctrl Pts',(1.31196701628196,-1.50420376666524,14.6122386173846));
#14244=CARTESIAN_POINT('Ctrl Pts',(1.36286643617424,-1.45657908801744,14.6166768406199));
#14245=CARTESIAN_POINT('Ctrl Pts',(1.41381977838484,-1.40890395627829,14.6211197656629));
#14246=CARTESIAN_POINT('Ctrl Pts',(1.46224257392157,-1.35857631480648,14.625562690706));
#14247=CARTESIAN_POINT('Ctrl Pts',(1.50786039712126,-1.30590374273654,14.630005615749));
#14248=CARTESIAN_POINT('Ctrl Pts',(1.55350484932201,-1.25320042351825,14.6344511343102));
#14249=CARTESIAN_POINT('Ctrl Pts',(1.59634076943718,-1.19814983568675,14.6388966528715));
#14250=CARTESIAN_POINT('Ctrl Pts',(1.63613534788825,-1.14109100683976,14.6433421714327));
#14251=CARTESIAN_POINT('Ctrl Pts',(1.6759993689896,-1.08393260874362,14.647795447548));
#14252=CARTESIAN_POINT('Ctrl Pts',(1.71281119567868,-1.02475938979194,14.6522487236632));
#14253=CARTESIAN_POINT('Ctrl Pts',(1.7463829026841,-0.963936885751685,14.6567019997785));
#14254=CARTESIAN_POINT('Ctrl Pts',(1.76435958637126,-0.931368183897583,
14.6590866010763));
#14255=CARTESIAN_POINT('Ctrl Pts',(1.78140803983468,-0.898326965747828,
14.6614712023741));
#14256=CARTESIAN_POINT('Ctrl Pts',(1.79750513532895,-0.864871580621115,
14.6638558036719));
#14257=CARTESIAN_POINT('Ctrl Pts',(1.82757183312203,-0.802382484093477,
14.6683098423899));
#14258=CARTESIAN_POINT('Ctrl Pts',(1.85443560269746,-0.738199890156618,
14.6727638811079));
#14259=CARTESIAN_POINT('Ctrl Pts',(1.87790365578977,-0.672685232535569,
14.6772179198259));
#14260=CARTESIAN_POINT('Ctrl Pts',(1.90133643275199,-0.607269053624067,
14.6816652634316));
#14261=CARTESIAN_POINT('Ctrl Pts',(1.92138346023068,-0.540525242221817,
14.6861126070374));
#14262=CARTESIAN_POINT('Ctrl Pts',(1.93789890410999,-0.472837604203937,
14.6905599506432));
#14263=CARTESIAN_POINT('Ctrl Pts',(1.95439487797856,-0.40522976295377,14.695002051288));
#14264=CARTESIAN_POINT('Ctrl Pts',(1.96736742174678,-0.336680778312421,
14.6994441519327));
#14265=CARTESIAN_POINT('Ctrl Pts',(1.97672024875239,-0.267590397197427,
14.7038862525775));
#14266=CARTESIAN_POINT('Ctrl Pts',(1.98606717595331,-0.198543598600828,
14.7083255511255));
#14267=CARTESIAN_POINT('Ctrl Pts',(1.99179885047881,-0.128956565028441,
14.7127648496736));
#14268=CARTESIAN_POINT('Ctrl Pts',(1.99387019594011,-0.0592385367960217,
14.7172041482216));
#14269=CARTESIAN_POINT('Ctrl Pts',(1.99594093863565,0.0104592033475351,
14.7216421549247));
#14270=CARTESIAN_POINT('Ctrl Pts',(1.99435345225302,0.0802873733827579,
14.7260801616277));
#14271=CARTESIAN_POINT('Ctrl Pts',(1.9891147034653,0.14983410478972,14.7305181683308));
#14272=CARTESIAN_POINT('Ctrl Pts',(1.98387569907679,0.219384229411427,14.7349563915661));
#14273=CARTESIAN_POINT('Ctrl Pts',(1.97498511775459,0.288652400145195,14.7393946148014));
#14274=CARTESIAN_POINT('Ctrl Pts',(1.96250185980714,0.357231035540775,14.7438328380367));
#14275=CARTESIAN_POINT('Ctrl Pts',(1.95000537722553,0.425882322432253,14.7482757630798));
#14276=CARTESIAN_POINT('Ctrl Pts',(1.93390870918407,0.493842133362405,14.7527186881228));
#14277=CARTESIAN_POINT('Ctrl Pts',(1.91432187784903,0.560713215903262,14.7571616131658));
#14278=CARTESIAN_POINT('Ctrl Pts',(1.89472361287431,0.627623333847515,14.7616071317271));
#14279=CARTESIAN_POINT('Ctrl Pts',(1.8716312916122,0.693442996346155,14.7660526502883));
#14280=CARTESIAN_POINT('Ctrl Pts',(1.84520390820222,0.757792913436942,14.7704981688496));
#14281=CARTESIAN_POINT('Ctrl Pts',(1.81873040827047,0.822255122929385,14.7749514449648));
#14282=CARTESIAN_POINT('Ctrl Pts',(1.7889104383344,0.885242024887659,14.77940472108));
#14283=CARTESIAN_POINT('Ctrl Pts',(1.75594958037184,0.946397714331535,14.7838579971953));
#14284=CARTESIAN_POINT('Ctrl Pts',(1.73829998878123,0.979144827387656,14.7862425984931));
#14285=CARTESIAN_POINT('Ctrl Pts',(1.71975057072094,1.01136734982018,14.7886271997909));
#14286=CARTESIAN_POINT('Ctrl Pts',(1.70033786218429,1.0430142457908,14.7910118010887));
#14287=CARTESIAN_POINT('Ctrl Pts',(1.66407815054065,1.1021253852871,14.7954658398067));
#14288=CARTESIAN_POINT('Ctrl Pts',(1.62466051492961,1.15946051834799,14.7999198785247));
#14289=CARTESIAN_POINT('Ctrl Pts',(1.58228445562378,1.21466187228849,14.8043739172427));
#14290=CARTESIAN_POINT('Ctrl Pts',(1.53997209411923,1.26978025001712,14.8088212608484));
#14291=CARTESIAN_POINT('Ctrl Pts',(1.49471043073078,1.32277082935464,14.8132686044542));
#14292=CARTESIAN_POINT('Ctrl Pts',(1.44674319681738,1.37330320212349,14.8177159480599));
#14293=CARTESIAN_POINT('Ctrl Pts',(1.39883251134216,1.42377600241912,14.8221580487047));
#14294=CARTESIAN_POINT('Ctrl Pts',(1.34822292568409,1.47179599853222,14.8266001493495));
#14295=CARTESIAN_POINT('Ctrl Pts',(1.29519839933177,1.51706580901041,14.8310422499943));
#14296=CARTESIAN_POINT('Ctrl Pts',(1.24220732108556,1.56230706309162,14.8354815485423));
#14297=CARTESIAN_POINT('Ctrl Pts',(1.18680469559286,1.6048012559041,14.8399208470903));
#14298=CARTESIAN_POINT('Ctrl Pts',(1.12931018983699,1.64428892157988,14.8443601456383));
#14299=CARTESIAN_POINT('Ctrl Pts',(1.07183241509984,1.68376509626423,14.8487981523414));
#14300=CARTESIAN_POINT('Ctrl Pts',(1.01226437189007,1.72023620361864,14.8532361590445));
#14301=CARTESIAN_POINT('Ctrl Pts',(0.950956113603648,1.75348511043004,14.8576741657476));
#14302=CARTESIAN_POINT('Ctrl Pts',(0.88964486406114,1.78673563946979,14.8621123889829));
#14303=CARTESIAN_POINT('Ctrl Pts',(0.826593662360921,1.81676342455656,14.8665506122182));
#14304=CARTESIAN_POINT('Ctrl Pts',(0.762177074998283,1.8433973171422,14.8709888354535));
#14305=CARTESIAN_POINT('Ctrl Pts',(0.697692245370325,1.87005942539773,14.8754317604965));
#14306=CARTESIAN_POINT('Ctrl Pts',(0.631839596301452,1.89332027736661,14.8798746855395));
#14307=CARTESIAN_POINT('Ctrl Pts',(0.565012688063195,1.91305729784228,14.8843176105826));
#14308=CARTESIAN_POINT('Ctrl Pts',(0.49814677020792,1.93280583962921,14.8887631291438));
#14309=CARTESIAN_POINT('Ctrl Pts',(0.430305937505898,1.94902634181036,14.8932086477051));
#14310=CARTESIAN_POINT('Ctrl Pts',(0.36189516215694,1.96164712782585,14.8976541662663));
#14311=CARTESIAN_POINT('Ctrl Pts',(0.293365008095398,1.97428993746523,14.9021074423816));
#14312=CARTESIAN_POINT('Ctrl Pts',(0.224263411437848,1.98332042829676,14.9065607184968));
#14313=CARTESIAN_POINT('Ctrl Pts',(0.155000906492105,1.98871875374238,14.911013994612));
#14314=CARTESIAN_POINT('Ctrl Pts',(0.117912826860775,1.99160940178001,14.9133985959098));
#14315=CARTESIAN_POINT('Ctrl Pts',(0.0807786240323059,1.9934594943657,14.9157831972076));
#14316=CARTESIAN_POINT('Ctrl Pts',(0.0436609877912965,1.99427211800323,
14.9181677985054));
#14317=CARTESIAN_POINT('Ctrl Pts',(-0.0256685848673973,1.99578996383686,
14.9226218372234));
#14318=CARTESIAN_POINT('Ctrl Pts',(-0.0952147042007433,1.99369121041427,
14.9270758759414));
#14319=CARTESIAN_POINT('Ctrl Pts',(-0.164568558321337,1.9879498867205,14.9315299146594));
#14320=CARTESIAN_POINT('Ctrl Pts',(-0.23381816282341,1.98221719312829,14.9359772582651));
#14321=CARTESIAN_POINT('Ctrl Pts',(-0.302875591799381,1.97285283653371,
14.9404246018709));
#14322=CARTESIAN_POINT('Ctrl Pts',(-0.371331093043246,1.95988284900892,
14.9448719454766));
#14323=CARTESIAN_POINT('Ctrl Pts',(-0.439705892287796,1.94692815176621,
14.9493140461214));
#14324=CARTESIAN_POINT('Ctrl Pts',(-0.50747969449479,1.93037635664942,14.9537561467662));
#14325=CARTESIAN_POINT('Ctrl Pts',(-0.574248734939866,1.91030519889361,
14.958198247411));
#14326=CARTESIAN_POINT('Ctrl Pts',(-0.640975657178532,1.89024670211301,
14.962637545959));
#14327=CARTESIAN_POINT('Ctrl Pts',(-0.706698607236841,1.86667338732895,
14.967076844507));
#14328=CARTESIAN_POINT('Ctrl Pts',(-0.771026365742641,1.83971353906789,
14.9715161430551));
#14329=CARTESIAN_POINT('Ctrl Pts',(-0.835335404739012,1.81276153617787,
14.9759541497581));
#14330=CARTESIAN_POINT('Ctrl Pts',(-0.898249606883893,1.78242514529255,
14.9803921564612));
#14331=CARTESIAN_POINT('Ctrl Pts',(-0.959396892739438,1.74888111794425,
14.9848301631642));
#14332=CARTESIAN_POINT('Ctrl Pts',(-1.02054716199727,1.71533545396846,14.9892683863995));
#14333=CARTESIAN_POINT('Ctrl Pts',(-1.07992991574231,1.67858208037216,14.9937066096349));
#14334=CARTESIAN_POINT('Ctrl Pts',(-1.13719846480731,1.63884325490265,14.9981448328702));
#14335=CARTESIAN_POINT('Ctrl Pts',(-1.19452768357992,1.59906233053311,15.0025877579132));
#14336=CARTESIAN_POINT('Ctrl Pts',(-1.24973782419091,1.55628992123207,15.0070306829562));
#14337=CARTESIAN_POINT('Ctrl Pts',(-1.30251275241996,1.51079055208966,15.0114736079993));
#14338=CARTESIAN_POINT('Ctrl Pts',(-1.35531848754674,1.46526462309281,15.0159191265605));
#14339=CARTESIAN_POINT('Ctrl Pts',(-1.40568582728078,1.41700890466694,15.0203646451217));
#14340=CARTESIAN_POINT('Ctrl Pts',(-1.45333525226866,1.36632507369703,15.024810163683));
#14341=CARTESIAN_POINT('Ctrl Pts',(-1.50106782683335,1.31555279802716,15.0292634397982));
#14342=CARTESIAN_POINT('Ctrl Pts',(-1.54607270297582,1.26234432549998,15.0337167159134));
#14343=CARTESIAN_POINT('Ctrl Pts',(-1.58811092639866,1.20703407075078,15.0381699920287));
#14344=CARTESIAN_POINT('Ctrl Pts',(-1.61062118615774,1.17741701987729,15.0405545933265));
#14345=CARTESIAN_POINT('Ctrl Pts',(-1.63228156273777,1.14719782153022,15.0429391946243));
#14346=CARTESIAN_POINT('Ctrl Pts',(-1.65306071014801,1.11643085368731,15.0453237959222));
#14347=CARTESIAN_POINT('Ctrl Pts',(-1.69250007913533,1.05803433849728,15.0498498319821));
#14348=CARTESIAN_POINT('Ctrl Pts',(-1.7289149253273,0.997436794586338,15.054375868042));
#14349=CARTESIAN_POINT('Ctrl Pts',(-1.76205646792578,0.934978377472412,
15.0589019041019));
#14350=CARTESIAN_POINT('Ctrl Pts',(-1.79514361190896,0.8726224797688,15.0634205111143));
#14351=CARTESIAN_POINT('Ctrl Pts',(-1.82496790410304,0.808412185118617,
15.0679391181267));
#14352=CARTESIAN_POINT('Ctrl Pts',(-1.85132377080753,0.742716539564723,
15.0724577251391));
#14353=CARTESIAN_POINT('Ctrl Pts',(-1.8776377558735,0.677125289791475,15.0769691517136));
#14354=CARTESIAN_POINT('Ctrl Pts',(-1.90049410200383,0.610053815379963,
15.081480578288));
#14355=CARTESIAN_POINT('Ctrl Pts',(-1.91973394386375,0.541894036945723,
15.0859920048625));
#14356=CARTESIAN_POINT('Ctrl Pts',(-1.93895579597693,0.473797989656515,
15.0904992131371));
#14357=CARTESIAN_POINT('Ctrl Pts',(-1.95456773249438,0.404616108680934,
15.0950064214117));
#14358=CARTESIAN_POINT('Ctrl Pts',(-1.9664600146909,0.334757484041611,15.0995136296864));
#14359=CARTESIAN_POINT('Ctrl Pts',(-1.97834478141561,0.264943007406439,
15.1040179895761));
#14360=CARTESIAN_POINT('Ctrl Pts',(-1.98651448514305,0.19445309810863,15.1085223494659));
#14361=CARTESIAN_POINT('Ctrl Pts',(-1.99091034060607,0.123707631809064,
15.1130267093556));
#14362=CARTESIAN_POINT('Ctrl Pts',(-1.9934894046851,0.0822010144004573,
15.1156694333688));
#14363=CARTESIAN_POINT('Ctrl Pts',(-1.99477039666107,0.0406066125744606,
15.118312157382));
#14364=CARTESIAN_POINT('Ctrl Pts',(-1.99474975438214,-0.000989895140077555,
15.1209548813952));
#14365=CARTESIAN_POINT('',(-1.99474960167085,-0.00126060858409071,15.9209548813952));
#14366=CARTESIAN_POINT('Ctrl Pts',(-1.99194226862274,-0.00100154882577569,
15.1209557114637));
#14367=CARTESIAN_POINT('Ctrl Pts',(-1.99314834912532,-0.270951609428265,
15.1381304054221));
#14368=CARTESIAN_POINT('Ctrl Pts',(-1.81615384618631,-1.20559135040691,
15.1976904318527));
#14369=CARTESIAN_POINT('Ctrl Pts',(-0.39307670270623,-2.32559105654038,
15.2996357907556));
#14370=CARTESIAN_POINT('Ctrl Pts',(1.74244179285117,-1.58958474294282,15.4267917881723));
#14371=CARTESIAN_POINT('Ctrl Pts',(2.27983395951717,0.604351034998105,15.5539477855891));
#14372=CARTESIAN_POINT('Ctrl Pts',(0.726216434408433,2.24399036247175,15.6811037830058));
#14373=CARTESIAN_POINT('Ctrl Pts',(-1.40931799962854,1.84136068164181,15.8034391074587));
#14374=CARTESIAN_POINT('Ctrl Pts',(-1.99268108475784,0.585369840690117,
15.8833890994392));
#14375=CARTESIAN_POINT('Ctrl Pts',(-1.99701534988654,-0.00124451225460149,
15.9209537589475));
#14376=CARTESIAN_POINT('',(-1.9947492845807,0.00168942735318613,16.7209548813952));
#14377=CARTESIAN_POINT('Ctrl Pts',(-1.99474960167085,-0.00126060858409071,
15.9209548813952));
#14378=CARTESIAN_POINT('Ctrl Pts',(-1.99470208524479,-0.0764491906300473,
15.9257751802099));
#14379=CARTESIAN_POINT('Ctrl Pts',(-1.99040364133295,-0.15150312980269,
15.9305954790246));
#14380=CARTESIAN_POINT('Ctrl Pts',(-1.98189826454668,-0.226068200963442,
15.9354157778393));
#14381=CARTESIAN_POINT('Ctrl Pts',(-1.97403915062585,-0.294967604657519,
15.9398698165573));
#14382=CARTESIAN_POINT('Ctrl Pts',(-1.9625673256446,-0.363593144450402,
15.9443238552752));
#14383=CARTESIAN_POINT('Ctrl Pts',(-1.94751226712666,-0.431536246323711,
15.9487778939932));
#14384=CARTESIAN_POINT('Ctrl Pts',(-1.93247983870082,-0.499377219158404,
15.953225237599));
#14385=CARTESIAN_POINT('Ctrl Pts',(-1.9138749719689,-0.566537315980175,
15.9576725812047));
#14386=CARTESIAN_POINT('Ctrl Pts',(-1.89177879811183,-0.632614054155122,
15.9621199248105));
#14387=CARTESIAN_POINT('Ctrl Pts',(-1.86970867337248,-0.698612894647751,
15.9665620254553));
#14388=CARTESIAN_POINT('Ctrl Pts',(-1.8441555706978,-0.763530451062614,
15.9710041261001));
#14389=CARTESIAN_POINT('Ctrl Pts',(-1.8152510421405,-0.826977155977006,
15.9754462267448));
#14390=CARTESIAN_POINT('Ctrl Pts',(-1.78636474668785,-0.890383838428903,
15.9798855252929));
#14391=CARTESIAN_POINT('Ctrl Pts',(-1.75413142171885,-0.952321065487502,
15.9843248238409));
#14392=CARTESIAN_POINT('Ctrl Pts',(-1.71873101120809,-1.01241852690062,
15.9887641223889));
#14393=CARTESIAN_POINT('Ctrl Pts',(-1.68334090228919,-1.07249849982955,
15.993202129092));
#14394=CARTESIAN_POINT('Ctrl Pts',(-1.64478578575177,-1.13073934831471,
15.997640135795));
#14395=CARTESIAN_POINT('Ctrl Pts',(-1.60329104367608,-1.18679627222539,
16.0020781424981));
#14396=CARTESIAN_POINT('Ctrl Pts',(-1.56179427705422,-1.24285593117729,
16.0065163657334));
#14397=CARTESIAN_POINT('Ctrl Pts',(-1.51735789333274,-1.29673106194095,
16.0109545889687));
#14398=CARTESIAN_POINT('Ctrl Pts',(-1.4702489349152,-1.34810816772273,16.015392812204));
#14399=CARTESIAN_POINT('Ctrl Pts',(-1.42309006975507,-1.39953970187818,
16.0198357372471));
#14400=CARTESIAN_POINT('Ctrl Pts',(-1.37325331028224,-1.44846756744527,
16.0242786622901));
#14401=CARTESIAN_POINT('Ctrl Pts',(-1.3210434525273,-1.49461425091385,16.0287215873331));
#14402=CARTESIAN_POINT('Ctrl Pts',(-1.2688031177294,-1.54078787210099,16.0331671058944));
#14403=CARTESIAN_POINT('Ctrl Pts',(-1.21418731085471,-1.58417677519995,
16.0376126244556));
#14404=CARTESIAN_POINT('Ctrl Pts',(-1.15753269447796,-1.62454474352497,
16.0420581430169));
#14405=CARTESIAN_POINT('Ctrl Pts',(-1.10077921421411,-1.66498315508159,
16.0465114191321));
#14406=CARTESIAN_POINT('Ctrl Pts',(-1.0419802354975,-1.70238984602281,16.0509646952473));
#14407=CARTESIAN_POINT('Ctrl Pts',(-0.981499380362869,-1.73657321436423,
16.0554179713626));
#14408=CARTESIAN_POINT('Ctrl Pts',(-0.949113621673195,-1.7548774251073,
16.0578025726604));
#14409=CARTESIAN_POINT('Ctrl Pts',(-0.916246009917864,-1.77225821794876,
16.0601871739582));
#14410=CARTESIAN_POINT('Ctrl Pts',(-0.882954658215231,-1.78869187789178,
16.062571775256));
#14411=CARTESIAN_POINT('Ctrl Pts',(-0.820771948848264,-1.81938722211212,
16.067025813974));
#14412=CARTESIAN_POINT('Ctrl Pts',(-0.756863528050589,-1.84689687916948,
16.071479852692));
#14413=CARTESIAN_POINT('Ctrl Pts',(-0.691588866982415,-1.87102442569999,
16.07593389141));
#14414=CARTESIAN_POINT('Ctrl Pts',(-0.626412323871697,-1.89511570477932,
16.0803812350157));
#14415=CARTESIAN_POINT('Ctrl Pts',(-0.55987407197145,-1.9158347951379,16.0848285786215));
#14416=CARTESIAN_POINT('Ctrl Pts',(-0.49235642696649,-1.93303199956048,
16.0892759222272));
#14417=CARTESIAN_POINT('Ctrl Pts',(-0.424918378324872,-1.95020893024674,
16.093718022872));
#14418=CARTESIAN_POINT('Ctrl Pts',(-0.356503701891035,-1.96387210102227,
16.0981601235168));
#14419=CARTESIAN_POINT('Ctrl Pts',(-0.287511153246104,-1.97392119884738,
16.1026022241616));
#14420=CARTESIAN_POINT('Ctrl Pts',(-0.218562125406478,-1.98396395765708,
16.1070415227096));
#14421=CARTESIAN_POINT('Ctrl Pts',(-0.149036431812932,-1.99039709566335,
16.1114808212577));
#14422=CARTESIAN_POINT('Ctrl Pts',(-0.0793428373953858,-1.99317141175917,
16.1159201198057));
#14423=CARTESIAN_POINT('Ctrl Pts',(-0.00966952395637401,-1.99594492052333,
16.1203581265088));
#14424=CARTESIAN_POINT('Ctrl Pts',(0.060171104389546,-1.99506170156083,
16.1247961332118));
#14425=CARTESIAN_POINT('Ctrl Pts',(0.129767129810311,-1.99052456767577,
16.1292341399149));
#14426=CARTESIAN_POINT('Ctrl Pts',(0.199366550850822,-1.985987212422,16.1336723631502));
#14427=CARTESIAN_POINT('Ctrl Pts',(0.268720856904589,-1.97779562253691,
16.1381105863855));
#14428=CARTESIAN_POINT('Ctrl Pts',(0.337421893263111,-1.96600458505232,
16.1425488096208));
#14429=CARTESIAN_POINT('Ctrl Pts',(0.406195710787947,-1.95420105626475,
16.1469917346639));
#14430=CARTESIAN_POINT('Ctrl Pts',(0.474314393816407,-1.93879055185456,
16.1514346597069));
#14431=CARTESIAN_POINT('Ctrl Pts',(0.541379600595374,-1.91987908227555,
16.1558775847499));
#14432=CARTESIAN_POINT('Ctrl Pts',(0.608483956096018,-1.90095657329332,
16.1603231033112));
#14433=CARTESIAN_POINT('Ctrl Pts',(0.67453314763782,-1.87852918892982,16.1647686218724));
#14434=CARTESIAN_POINT('Ctrl Pts',(0.739146301158942,-1.85275209026547,
16.1692141404337));
#14435=CARTESIAN_POINT('Ctrl Pts',(0.803872206436622,-1.82693000984439,
16.1736674165489));
#14436=CARTESIAN_POINT('Ctrl Pts',(0.86715662689341,-1.79774675175449,16.1781206926642));
#14437=CARTESIAN_POINT('Ctrl Pts',(0.928641602442285,-1.76540429837288,
16.1825739687794));
#14438=CARTESIAN_POINT('Ctrl Pts',(0.961565038738243,-1.74808584465213,
16.1849585700772));
#14439=CARTESIAN_POINT('Ctrl Pts',(0.993972985444529,-1.72986231995028,
16.187343171375));
#14440=CARTESIAN_POINT('Ctrl Pts',(1.02581404086845,-1.71076974372858,16.1897277726728));
#14441=CARTESIAN_POINT('Ctrl Pts',(1.08528783793931,-1.67510798601822,16.1941818113908));
#14442=CARTESIAN_POINT('Ctrl Pts',(1.14301756517406,-1.63627055467081,16.1986358501087));
#14443=CARTESIAN_POINT('Ctrl Pts',(1.19864345620722,-1.59445333183246,16.2030898888267));
#14444=CARTESIAN_POINT('Ctrl Pts',(1.25418573288342,-1.55269896677728,16.2075372324325));
#14445=CARTESIAN_POINT('Ctrl Pts',(1.30763006179368,-1.50797399189125,16.2119845760382));
#14446=CARTESIAN_POINT('Ctrl Pts',(1.35864359363725,-1.46051879411683,16.216431919644));
#14447=CARTESIAN_POINT('Ctrl Pts',(1.40959698577044,-1.41311954114268,16.2208740202888));
#14448=CARTESIAN_POINT('Ctrl Pts',(1.45812491568086,-1.36299678976376,16.2253161209336));
#14449=CARTESIAN_POINT('Ctrl Pts',(1.5039271534303,-1.31043148606672,16.2297582215784));
#14450=CARTESIAN_POINT('Ctrl Pts',(1.54970049892527,-1.25789934079611,16.2341975201264));
#14451=CARTESIAN_POINT('Ctrl Pts',(1.59275124224513,-1.20292806799045,16.2386368186744));
#14452=CARTESIAN_POINT('Ctrl Pts',(1.63281670701351,-1.14583470177751,16.2430761172224));
#14453=CARTESIAN_POINT('Ctrl Pts',(1.67287051264969,-1.08875794985093,16.2475141239255));
#14454=CARTESIAN_POINT('Ctrl Pts',(1.70994048321272,-1.02956073094718,16.2519521306286));
#14455=CARTESIAN_POINT('Ctrl Pts',(1.74380596639477,-0.968590890967903,
16.2563901373316));
#14456=CARTESIAN_POINT('Ctrl Pts',(1.77767310188819,-0.90761807624412,16.2608283605669));
#14457=CARTESIAN_POINT('Ctrl Pts',(1.80833520396687,-0.844872897870323,
16.2652665838022));
#14458=CARTESIAN_POINT('Ctrl Pts',(1.83561735544561,-0.78072817733631,16.2697048070375));
#14459=CARTESIAN_POINT('Ctrl Pts',(1.86292840935303,-0.71651550254979,16.2741477320806));
#14460=CARTESIAN_POINT('Ctrl Pts',(1.88685217379302,-0.650900777687739,
16.2785906571236));
#14461=CARTESIAN_POINT('Ctrl Pts',(1.90726211090804,-0.584276306891349,
16.2830335821666));
#14462=CARTESIAN_POINT('Ctrl Pts',(1.92768396214346,-0.517612944649016,
16.2874791007279));
#14463=CARTESIAN_POINT('Ctrl Pts',(1.94458778476755,-0.449939138391337,
16.2919246192891));
#14464=CARTESIAN_POINT('Ctrl Pts',(1.95789782189687,-0.381659116898178,
16.2963701378504));
#14465=CARTESIAN_POINT('Ctrl Pts',(1.97123108541253,-0.313259944861491,
16.3008234139656));
#14466=CARTESIAN_POINT('Ctrl Pts',(1.98095797655841,-0.244252930624363,
16.3052766900809));
#14467=CARTESIAN_POINT('Ctrl Pts',(1.98705450970589,-0.175048387474627,
16.3097299661961));
#14468=CARTESIAN_POINT('Ctrl Pts',(1.99031902788971,-0.137991344717777,
16.3121145674939));
#14469=CARTESIAN_POINT('Ctrl Pts',(1.9925435086667,-0.100877687560439,16.3144991687917));
#14470=CARTESIAN_POINT('Ctrl Pts',(1.99373040618451,-0.0637701337254548,
16.3168837700896));
#14471=CARTESIAN_POINT('Ctrl Pts',(1.99594733339302,0.00554060667434544,
16.3213378088076));
#14472=CARTESIAN_POINT('Ctrl Pts',(1.99455002903019,0.0751043545663258,
16.3257918475255));
#14473=CARTESIAN_POINT('Ctrl Pts',(1.98950840071178,0.144512580757758,16.3302458862435));
#14474=CARTESIAN_POINT('Ctrl Pts',(1.98447435074406,0.213816475601102,16.3346932298493));
#14475=CARTESIAN_POINT('Ctrl Pts',(1.97580688443937,0.282964828430934,16.339140573455));
#14476=CARTESIAN_POINT('Ctrl Pts',(1.96352790037351,0.351547645355233,16.3435879170608));
#14477=CARTESIAN_POINT('Ctrl Pts',(1.9512633919677,0.420049610187985,16.3480300177056));
#14478=CARTESIAN_POINT('Ctrl Pts',(1.93539590780862,0.487986883710277,16.3524721183504));
#14479=CARTESIAN_POINT('Ctrl Pts',(1.91599910738696,0.55495493780339,16.3569142189952));
#14480=CARTESIAN_POINT('Ctrl Pts',(1.89661454255294,0.621880748151312,16.3613535175432));
#14481=CARTESIAN_POINT('Ctrl Pts',(1.87370521382342,0.687838082780794,16.3657928160912));
#14482=CARTESIAN_POINT('Ctrl Pts',(1.84739545392445,0.752434448519792,16.3702321146392));
#14483=CARTESIAN_POINT('Ctrl Pts',(1.82109335021942,0.817012016584237,16.3746701213423));
#14484=CARTESIAN_POINT('Ctrl Pts',(1.79139296429455,0.880228948804925,16.3791081280453));
#14485=CARTESIAN_POINT('Ctrl Pts',(1.75846728643509,0.941711402202184,16.3835461347484));
#14486=CARTESIAN_POINT('Ctrl Pts',(1.72554000211776,1.00319685535458,16.3879843579837));
#14487=CARTESIAN_POINT('Ctrl Pts',(1.68938734666912,1.06294723122832,16.392422581219));
#14488=CARTESIAN_POINT('Ctrl Pts',(1.65022807032527,1.12061361691287,16.3968608044543));
#14489=CARTESIAN_POINT('Ctrl Pts',(1.61102730904968,1.17834109376909,16.4013037294974));
#14490=CARTESIAN_POINT('Ctrl Pts',(1.5688138449804,1.23397976804312,16.4057466545404));
#14491=CARTESIAN_POINT('Ctrl Pts',(1.52384900168036,1.28721085396984,16.4101895795834));
#14492=CARTESIAN_POINT('Ctrl Pts',(1.47885791055047,1.34047301307249,16.4146350981447));
#14493=CARTESIAN_POINT('Ctrl Pts',(1.43111257864675,1.39132442951403,16.4190806167059));
#14494=CARTESIAN_POINT('Ctrl Pts',(1.38091184868274,1.43948255587472,16.4235261352672));
#14495=CARTESIAN_POINT('Ctrl Pts',(1.33062351704363,1.48772471951021,16.4279794113824));
#14496=CARTESIAN_POINT('Ctrl Pts',(1.27787160477796,1.53326389141308,16.4324326874976));
#14497=CARTESIAN_POINT('Ctrl Pts',(1.22298809976581,1.57585775701084,16.4368859636129));
#14498=CARTESIAN_POINT('Ctrl Pts',(1.19359956110515,1.59866554717565,16.4392705649107));
#14499=CARTESIAN_POINT('Ctrl Pts',(1.16360033488857,1.62062956977358,16.4416551662085));
#14500=CARTESIAN_POINT('Ctrl Pts',(1.133044480218,1.64171793202959,16.4440397675062));
#14501=CARTESIAN_POINT('Ctrl Pts',(1.075971224454,1.68110748619711,16.4484938062242));
#14502=CARTESIAN_POINT('Ctrl Pts',(1.01672846294902,1.71759532923459,16.4529478449422));
#14503=CARTESIAN_POINT('Ctrl Pts',(0.9556433773219,1.75093497819902,16.4574018836602));
#14504=CARTESIAN_POINT('Ctrl Pts',(0.894650112069388,1.78422451249101,16.461849227266));
#14505=CARTESIAN_POINT('Ctrl Pts',(0.831820445286944,1.81437501237467,16.4662965708717));
#14506=CARTESIAN_POINT('Ctrl Pts',(0.767510938572033,1.84118291369225,16.4707439144775));
#14507=CARTESIAN_POINT('Ctrl Pts',(0.703277246155202,1.86795921124974,16.4751860151223));
#14508=CARTESIAN_POINT('Ctrl Pts',(0.637567628450513,1.89140054927231,16.4796281157671));
#14509=CARTESIAN_POINT('Ctrl Pts',(0.570762075637924,1.91134984121523,16.4840702164118));
#14510=CARTESIAN_POINT('Ctrl Pts',(0.503998664063982,1.93128654905642,16.4885095149599));
#14511=CARTESIAN_POINT('Ctrl Pts',(0.436141156807205,1.94773544090862,16.4929488135079));
#14512=CARTESIAN_POINT('Ctrl Pts',(0.367586860665507,1.96058854999362,16.4973881120559));
#14513=CARTESIAN_POINT('Ctrl Pts',(0.299052513964234,1.97343791879757,16.501826118759));
#14514=CARTESIAN_POINT('Ctrl Pts',(0.229822261833278,1.98269349189533,16.506264125462));
#14515=CARTESIAN_POINT('Ctrl Pts',(0.160304074559982,1.9882983091527,16.5107021321651));
#14516=CARTESIAN_POINT('Ctrl Pts',(0.0907824954646867,1.99390339987149,
16.5151403554004));
#14517=CARTESIAN_POINT('Ctrl Pts',(0.0209734415047426,1.99585734415392,
16.5195785786357));
#14518=CARTESIAN_POINT('Ctrl Pts',(-0.0487113021962039,1.9941551523235,
16.524016801871));
#14519=CARTESIAN_POINT('Ctrl Pts',(-0.118469869192843,1.99245115720868,
16.528459726914));
#14520=CARTESIAN_POINT('Ctrl Pts',(-0.188103372686751,1.98708330709254,
16.5329026519571));
#14521=CARTESIAN_POINT('Ctrl Pts',(-0.257202307474941,1.97809871733682,
16.5373455770001));
#14522=CARTESIAN_POINT('Ctrl Pts',(-0.326341578155567,1.96910888290624,
16.5417910955614));
#14523=CARTESIAN_POINT('Ctrl Pts',(-0.394945177390739,1.95649819518938,
16.5462366141226));
#14524=CARTESIAN_POINT('Ctrl Pts',(-0.462613754326337,1.9403649339256,16.5506821326839));
#14525=CARTESIAN_POINT('Ctrl Pts',(-0.530400414817623,1.92420351967056,
16.5551354087991));
#14526=CARTESIAN_POINT('Ctrl Pts',(-0.59724832641095,1.90450739972527,16.5595886849143));
#14527=CARTESIAN_POINT('Ctrl Pts',(-0.662774019135407,1.88142450341732,
16.5640419610296));
#14528=CARTESIAN_POINT('Ctrl Pts',(-0.697861143281239,1.86906427623425,
16.5664265623274));
#14529=CARTESIAN_POINT('Ctrl Pts',(-0.732569496974778,1.85573378313794,
16.5688111636252));
#14530=CARTESIAN_POINT('Ctrl Pts',(-0.766842997887297,1.8414612075988,16.571195764923));
#14531=CARTESIAN_POINT('Ctrl Pts',(-0.830860198668538,1.81480240970457,
16.575649803641));
#14532=CARTESIAN_POINT('Ctrl Pts',(-0.893612360096667,1.78474856275656,
16.580103842359));
#14533=CARTESIAN_POINT('Ctrl Pts',(-0.954715109778675,1.75144129837694,
16.584557881077));
#14534=CARTESIAN_POINT('Ctrl Pts',(-1.01572601253417,1.71818409999074,16.5890052246827));
#14535=CARTESIAN_POINT('Ctrl Pts',(-1.07509199803898,1.68168342278787,16.5934525682885));
#14536=CARTESIAN_POINT('Ctrl Pts',(-1.13244887152319,1.64212883656729,16.5978999118943));
#14537=CARTESIAN_POINT('Ctrl Pts',(-1.18973812714929,1.60262088113805,16.602342012539));
#14538=CARTESIAN_POINT('Ctrl Pts',(-1.24502257389276,1.56006644381997,16.6067841131838));
#14539=CARTESIAN_POINT('Ctrl Pts',(-1.29796440887436,1.51469995569929,16.6112262138286));
#14540=CARTESIAN_POINT('Ctrl Pts',(-1.35087284791194,1.46936208496028,16.6156655123766));
#14541=CARTESIAN_POINT('Ctrl Pts',(-1.40144123578169,1.42121600015034,16.6201048109247));
#14542=CARTESIAN_POINT('Ctrl Pts',(-1.44936369199552,1.370537285456,16.6245441094727));
#14543=CARTESIAN_POINT('Ctrl Pts',(-1.49727220267658,1.31987331837129,16.6289821161758));
#14544=CARTESIAN_POINT('Ctrl Pts',(-1.54253597402509,1.26667853999219,16.6334201228788));
#14545=CARTESIAN_POINT('Ctrl Pts',(-1.58488623643313,1.21126511551552,16.6378581295819));
#14546=CARTESIAN_POINT('Ctrl Pts',(-1.62723856512853,1.15584898739425,16.6422963528172));
#14547=CARTESIAN_POINT('Ctrl Pts',(-1.66667680728718,1.09821438868407,16.6467345760525));
#14548=CARTESIAN_POINT('Ctrl Pts',(-1.70297382245688,1.03870482935558,16.6511727992878));
#14549=CARTESIAN_POINT('Ctrl Pts',(-1.73930929030848,0.979132226216345,
16.6556157243308));
#14550=CARTESIAN_POINT('Ctrl Pts',(-1.77249663364252,0.917681116656479,
16.6600586493739));
#14551=CARTESIAN_POINT('Ctrl Pts',(-1.80235375408574,0.854721304071116,
16.6645015744169));
#14552=CARTESIAN_POINT('Ctrl Pts',(-1.83222830335912,0.791724739251659,
16.6689470929782));
#14553=CARTESIAN_POINT('Ctrl Pts',(-1.85876857412591,0.727218171366367,
16.6733926115394));
#14554=CARTESIAN_POINT('Ctrl Pts',(-1.88184098253303,0.661590567465335,
16.6778381301007));
#14555=CARTESIAN_POINT('Ctrl Pts',(-1.90495365293689,0.595848441563515,
16.6822914062159));
#14556=CARTESIAN_POINT('Ctrl Pts',(-1.9245862431658,0.528981844325455,16.6867446823311));
#14557=CARTESIAN_POINT('Ctrl Pts',(-1.94065551072978,0.461393271704447,
16.6911979584464));
#14558=CARTESIAN_POINT('Ctrl Pts',(-1.94926014140979,0.4252015346961,16.6935825597442));
#14559=CARTESIAN_POINT('Ctrl Pts',(-1.95684394291397,0.388802938335382,
16.695967161042));
#14560=CARTESIAN_POINT('Ctrl Pts',(-1.96340024706993,0.352259893126834,
16.6983517623397));
#14561=CARTESIAN_POINT('Ctrl Pts',(-1.98210878387135,0.247983628655827,
16.7051562668403));
#14562=CARTESIAN_POINT('Ctrl Pts',(-1.99251386625485,0.142175269986685,
16.7119607713409));
#14563=CARTESIAN_POINT('Ctrl Pts',(-1.99442689448622,0.0359016023326883,
16.7187652758415));
#14564=CARTESIAN_POINT('Ctrl Pts',(-1.99463209077638,0.0245024175287777,
16.7194951443594));
#14565=CARTESIAN_POINT('Ctrl Pts',(-1.99473962231119,0.0130979115153709,
16.7202250128773));
#14566=CARTESIAN_POINT('Ctrl Pts',(-1.9947492845807,0.00168942735318613,
16.7209548813952));
#14567=CARTESIAN_POINT('',(-1.99474912755533,-0.00183980182347288,18.3208813761083));
#14568=CARTESIAN_POINT('Ctrl Pts',(-1.99474925275694,0.00172659365242297,
16.7215926364432));
#14569=CARTESIAN_POINT('Ctrl Pts',(-1.9948994043772,-0.171744930408297,
16.7317021781126));
#14570=CARTESIAN_POINT('Ctrl Pts',(-1.97242273040134,-0.344485109801641,
16.7415934927886));
#14571=CARTESIAN_POINT('Ctrl Pts',(-1.92332842871311,-0.529292035933361,
16.7533687939037));
#14572=CARTESIAN_POINT('Ctrl Pts',(-1.91854507022307,-0.546376323251258,
16.7544681225366));
#14573=CARTESIAN_POINT('Ctrl Pts',(-1.90971083131583,-0.576381289381483,
16.7564191862247));
#14574=CARTESIAN_POINT('Ctrl Pts',(-1.90575503525689,-0.589328924470519,
16.7572678390983));
#14575=CARTESIAN_POINT('Ctrl Pts',(-1.89975133155701,-0.608286722314829,
16.758520745853));
#14576=CARTESIAN_POINT('Ctrl Pts',(-1.89780597949355,-0.614329163383226,
16.7589216349931));
#14577=CARTESIAN_POINT('Ctrl Pts',(-1.89432082183775,-0.624979833699323,
16.7596310405278));
#14578=CARTESIAN_POINT('Ctrl Pts',(-1.89279295214639,-0.629591937845154,
16.7599391615746));
#14579=CARTESIAN_POINT('Ctrl Pts',(-1.88977632663741,-0.638587841829782,
16.7605419778444));
#14580=CARTESIAN_POINT('Ctrl Pts',(-1.88828912784532,-0.642972134324393,
16.7608366199334));
#14581=CARTESIAN_POINT('Ctrl Pts',(-1.88424328583784,-0.654764251324876,
16.7616314115169));
#14582=CARTESIAN_POINT('Ctrl Pts',(-1.88165624629358,-0.662162180222608,
16.7621324994249));
#14583=CARTESIAN_POINT('Ctrl Pts',(-1.87194113812885,-0.689426888809651,
16.76398848772));
#14584=CARTESIAN_POINT('Ctrl Pts',(-1.86454168532692,-0.709194829619769,
16.7653523793483));
#14585=CARTESIAN_POINT('Ctrl Pts',(-1.79906712736228,-0.876000939067973,
16.7770210675995));
#14586=CARTESIAN_POINT('Ctrl Pts',(-1.72402591656126,-1.01574373637432,
16.7879273345357));
#14587=CARTESIAN_POINT('Ctrl Pts',(-1.60084333265233,-1.19143849657189,
16.8028983703572));
#14588=CARTESIAN_POINT('Ctrl Pts',(-1.56642649265493,-1.23633871549537,
16.8068448240526));
#14589=CARTESIAN_POINT('Ctrl Pts',(-1.48724104459771,-1.33102015279967,
16.8153594114098));
#14590=CARTESIAN_POINT('Ctrl Pts',(-1.44177620401722,-1.38013910794963,
16.8199044840105));
#14591=CARTESIAN_POINT('Ctrl Pts',(-1.38713736152488,-1.43351579268262,
16.8249086803122));
#14592=CARTESIAN_POINT('Ctrl Pts',(-1.38030290565556,-1.44009773448856,
16.8255269360352));
#14593=CARTESIAN_POINT('Ctrl Pts',(-1.37121476338787,-1.44872595574021,
16.8263386600464));
#14594=CARTESIAN_POINT('Ctrl Pts',(-1.36900313404944,-1.45081606050871,
16.8265353910736));
#14595=CARTESIAN_POINT('Ctrl Pts',(-1.3649408153359,-1.45463760293236,16.826895260109));
#14596=CARTESIAN_POINT('Ctrl Pts',(-1.36309159758088,-1.45637058539894,
16.8270585156862));
#14597=CARTESIAN_POINT('Ctrl Pts',(-1.35926721863651,-1.45994091243707,
16.8273949793856));
#14598=CARTESIAN_POINT('Ctrl Pts',(-1.35729165717887,-1.46177775223665,
16.8275681458309));
#14599=CARTESIAN_POINT('Ctrl Pts',(-1.35278065399623,-1.4659549686477,16.8279621055132));
#14600=CARTESIAN_POINT('Ctrl Pts',(-1.35024286756976,-1.46829277289816,
16.8281827015492));
#14601=CARTESIAN_POINT('Ctrl Pts',(-1.34363014384941,-1.47435275911044,
16.8287548618229));
#14602=CARTESIAN_POINT('Ctrl Pts',(-1.33954576808004,-1.47806466661737,
16.8291056590812));
#14603=CARTESIAN_POINT('Ctrl Pts',(-1.31385095224521,-1.50122229483311,
16.8312966892293));
#14604=CARTESIAN_POINT('Ctrl Pts',(-1.29183164696232,-1.52021179910685,
16.8331044695181));
#14605=CARTESIAN_POINT('Ctrl Pts',(-1.25845104809376,-1.5477500207383,16.8357567859099));
#14606=CARTESIAN_POINT('Ctrl Pts',(-1.2474019478171,-1.55666874050016,16.83662083217));
#14607=CARTESIAN_POINT('Ctrl Pts',(-1.20548670207555,-1.5897694100824,16.8398508627155));
#14608=CARTESIAN_POINT('Ctrl Pts',(-1.17400376007209,-1.61315852831366,
16.8421810471608));
#14609=CARTESIAN_POINT('Ctrl Pts',(-1.01786649088892,-1.72216122292385,
16.8533871055019));
#14610=CARTESIAN_POINT('Ctrl Pts',(-0.88444612827677,-1.79433771774679,
16.8619525983611));
#14611=CARTESIAN_POINT('Ctrl Pts',(-0.702313560237534,-1.86756966347505,
16.8736804603366));
#14612=CARTESIAN_POINT('Ctrl Pts',(-0.659921588079329,-1.88296676857671,
16.8764088542704));
#14613=CARTESIAN_POINT('Ctrl Pts',(-0.591111789626785,-1.90534988709954,
16.8808604994485));
#14614=CARTESIAN_POINT('Ctrl Pts',(-0.565007894413109,-1.91325306901849,
16.8825543678677));
#14615=CARTESIAN_POINT('Ctrl Pts',(-0.530358470074206,-1.92297255179209,
16.8848127223741));
#14616=CARTESIAN_POINT('Ctrl Pts',(-0.521950570935666,-1.92527170532885,
16.8853614881375));
#14617=CARTESIAN_POINT('Ctrl Pts',(-0.508369856064159,-1.92888987416888,
16.8862492058251));
#14618=CARTESIAN_POINT('Ctrl Pts',(-0.503206279167951,-1.93024337764132,
16.8865870378666));
#14619=CARTESIAN_POINT('Ctrl Pts',(-0.493348682451939,-1.93278505927322,
16.8872325965002));
#14620=CARTESIAN_POINT('Ctrl Pts',(-0.488655640713422,-1.9339769057428,
16.8875402018763));
#14621=CARTESIAN_POINT('Ctrl Pts',(-0.477920263904788,-1.93666169540857,
16.8882444797975));
#14622=CARTESIAN_POINT('Ctrl Pts',(-0.471875210960821,-1.93814346345745,
16.8886415097306));
#14623=CARTESIAN_POINT('Ctrl Pts',(-0.4532823114638,-1.94260882801189,16.8898641116329));
#14624=CARTESIAN_POINT('Ctrl Pts',(-0.440712579907381,-1.94549899035605,
16.8906926763946));
#14625=CARTESIAN_POINT('Ctrl Pts',(-0.322053805326525,-1.97157329820106,
16.8985346764807));
#14626=CARTESIAN_POINT('Ctrl Pts',(-0.214284177716429,-1.98617599770517,
16.9058249880465));
#14627=CARTESIAN_POINT('Ctrl Pts',(0.0105743818970425,-1.99812789040067,
16.9213305372507));
#14628=CARTESIAN_POINT('Ctrl Pts',(0.127338589318617,-1.99409380935541,
16.9295457174404));
#14629=CARTESIAN_POINT('Ctrl Pts',(0.308036457627854,-1.97190877770144,
16.9421124625644));
#14630=CARTESIAN_POINT('Ctrl Pts',(0.372569782670456,-1.96074074657256,
16.9465662921488));
#14631=CARTESIAN_POINT('Ctrl Pts',(0.444197396236631,-1.94467976401054,
16.9513911718664));
#14632=CARTESIAN_POINT('Ctrl Pts',(0.451941174288067,-1.94289471955762,
16.9519112068623));
#14633=CARTESIAN_POINT('Ctrl Pts',(0.465673474099328,-1.93964269581101,
16.9528303252453));
#14634=CARTESIAN_POINT('Ctrl Pts',(0.471666198362962,-1.93819415220633,
16.9532303807111));
#14635=CARTESIAN_POINT('Ctrl Pts',(0.480829461178627,-1.93593421911843,
16.9538403896719));
#14636=CARTESIAN_POINT('Ctrl Pts',(0.484004811672894,-1.93514278908439,
16.9540514628638));
#14637=CARTESIAN_POINT('Ctrl Pts',(0.489534727765527,-1.93375004024472,
16.954418485626));
#14638=CARTESIAN_POINT('Ctrl Pts',(0.491890145365829,-1.93315223222354,
16.9545746362311));
#14639=CARTESIAN_POINT('Ctrl Pts',(0.497215144611382,-1.93179037795604,
16.9549272442797));
#14640=CARTESIAN_POINT('Ctrl Pts',(0.500184053111433,-1.93102379004457,
16.9551235523412));
#14641=CARTESIAN_POINT('Ctrl Pts',(0.508262478038432,-1.92891801695474,
16.9556569597983));
#14642=CARTESIAN_POINT('Ctrl Pts',(0.513368507351877,-1.92756536592288,
16.9559932877992));
#14643=CARTESIAN_POINT('Ctrl Pts',(0.536775865871086,-1.92126485636246,
16.9575316078273));
#14644=CARTESIAN_POINT('Ctrl Pts',(0.555012190995416,-1.91607633193075,
16.958720271562));
#14645=CARTESIAN_POINT('Ctrl Pts',(0.772893989837999,-1.85071361081576,
16.9728345776938));
#14646=CARTESIAN_POINT('Ctrl Pts',(0.962014661774332,-1.75984760028207,
16.9843177136664));
#14647=CARTESIAN_POINT('Ctrl Pts',(1.17498156820318,-1.61275233921025,16.9997125136978));
#14648=CARTESIAN_POINT('Ctrl Pts',(1.21522493314839,-1.58264954477472,17.0027409572631));
#14649=CARTESIAN_POINT('Ctrl Pts',(1.27767310424683,-1.53214997706384,17.0076721875744));
#14650=CARTESIAN_POINT('Ctrl Pts',(1.30062742208306,-1.51271288465045,17.0095381713437));
#14651=CARTESIAN_POINT('Ctrl Pts',(1.32964809270891,-1.48699001827664,17.0119718292607));
#14652=CARTESIAN_POINT('Ctrl Pts',(1.33612557928478,-1.48117244013243,17.0125199621396));
#14653=CARTESIAN_POINT('Ctrl Pts',(1.34651102714585,-1.47172147055319,17.0134069025389));
#14654=CARTESIAN_POINT('Ctrl Pts',(1.35044290581014,-1.46811443367237,17.0137445937677));
#14655=CARTESIAN_POINT('Ctrl Pts',(1.35791552585645,-1.46120376324465,17.0143900471389));
#14656=CARTESIAN_POINT('Ctrl Pts',(1.36145880687509,-1.45790292186587,17.014697688757));
#14657=CARTESIAN_POINT('Ctrl Pts',(1.36953178293895,-1.45032722186913,17.0154022806826));
#14658=CARTESIAN_POINT('Ctrl Pts',(1.37405352866221,-1.44604400136752,17.0157995895204));
#14659=CARTESIAN_POINT('Ctrl Pts',(1.38789307432268,-1.43281097737236,17.0170238909704));
#14660=CARTESIAN_POINT('Ctrl Pts',(1.39714389626438,-1.42379190990298,17.0178538884728));
#14661=CARTESIAN_POINT('Ctrl Pts',(1.48450426569155,-1.33694887347381,17.0258052492516));
#14662=CARTESIAN_POINT('Ctrl Pts',(1.55610872897948,-1.25287804302608,17.0332124779335));
#14663=CARTESIAN_POINT('Ctrl Pts',(1.72069295185624,-1.02363122956328,17.0526580529795));
#14664=CARTESIAN_POINT('Ctrl Pts',(1.80250219960301,-0.871545664910423,
17.0649278097243));
#14665=CARTESIAN_POINT('Ctrl Pts',(1.87045707916498,-0.693374228043355,
17.0775748386209));
#14666=CARTESIAN_POINT('Ctrl Pts',(1.87687755349391,-0.67580190648771,17.0788038610264));
#14667=CARTESIAN_POINT('Ctrl Pts',(1.88470707528509,-0.653400354238045,
17.0803452457166));
#14668=CARTESIAN_POINT('Ctrl Pts',(1.88634611592212,-0.648653308651839,
17.0806704399948));
#14669=CARTESIAN_POINT('Ctrl Pts',(1.88893830440373,-0.641052801666418,
17.0811887589727));
#14670=CARTESIAN_POINT('Ctrl Pts',(1.88990294140914,-0.638203325528641,
17.0813825531489));
#14671=CARTESIAN_POINT('Ctrl Pts',(1.8917253641804,-0.632779638716112,17.0817504047403));
#14672=CARTESIAN_POINT('Ctrl Pts',(1.89258433324488,-0.630205891986746,
17.0819245283432));
#14673=CARTESIAN_POINT('Ctrl Pts',(1.89454643989515,-0.624286599877598,
17.0823240011495));
#14674=CARTESIAN_POINT('Ctrl Pts',(1.89564596778135,-0.620939881958067,
17.0825491356964));
#14675=CARTESIAN_POINT('Ctrl Pts',(1.89911191100711,-0.61029531361799,17.0832629519958));
#14676=CARTESIAN_POINT('Ctrl Pts',(1.90144512903528,-0.602986605325512,
17.0837497182536));
#14677=CARTESIAN_POINT('Ctrl Pts',(1.93860849380738,-0.484212959314738,
17.0916086666477));
#14678=CARTESIAN_POINT('Ctrl Pts',(1.96363218844635,-0.369895265604416,
17.0984454910807));
#14679=CARTESIAN_POINT('Ctrl Pts',(1.9915189556957,-0.15269870485207,17.1111697144121));
#14680=CARTESIAN_POINT('Ctrl Pts',(1.99672509665209,-0.0505228940066942,
17.1170514265565));
#14681=CARTESIAN_POINT('Ctrl Pts',(1.99270943470483,0.104661765903216,17.1262635987637));
#14682=CARTESIAN_POINT('Ctrl Pts',(1.98921912902339,0.157643813186542,17.1294565384666));
#14683=CARTESIAN_POINT('Ctrl Pts',(1.98030894344449,0.24163944795052,17.1346375721887));
#14684=CARTESIAN_POINT('Ctrl Pts',(1.97626092486122,0.272774118786872,17.1365841223805));
#14685=CARTESIAN_POINT('Ctrl Pts',(1.97014267021654,0.312478056773421,17.1391049179435));
#14686=CARTESIAN_POINT('Ctrl Pts',(1.96874797688675,0.321148060098795,17.1396577293189));
#14687=CARTESIAN_POINT('Ctrl Pts',(1.96641112796066,0.335087283356144,17.1405504160252));
#14688=CARTESIAN_POINT('Ctrl Pts',(1.96550492070334,0.340362479445814,17.1408891484088));
#14689=CARTESIAN_POINT('Ctrl Pts',(1.96373909107313,0.350399425856803,17.1415353881304));
#14690=CARTESIAN_POINT('Ctrl Pts',(1.96288335132864,0.355161827690542,17.1418427698532));
#14691=CARTESIAN_POINT('Ctrl Pts',(1.96089217282094,0.366016188404977,17.1425450791558));
#14692=CARTESIAN_POINT('Ctrl Pts',(1.95974566113158,0.37210604113401,17.1429403569519));
#14693=CARTESIAN_POINT('Ctrl Pts',(1.95669444715618,0.387907654978254,17.1439692887114));
#14694=CARTESIAN_POINT('Ctrl Pts',(1.95474583018036,0.397610666165398,17.1446043378246));
#14695=CARTESIAN_POINT('Ctrl Pts',(1.94964671769277,0.422057507515832,17.146212678081));
#14696=CARTESIAN_POINT('Ctrl Pts',(1.94640116564796,0.436780660137741,17.1471889775793));
#14697=CARTESIAN_POINT('Ctrl Pts',(1.9066627737484,0.607804360083217,17.1586211796375));
#14698=CARTESIAN_POINT('Ctrl Pts',(1.85160712706223,0.759157293208993,17.1697041949126));
#14699=CARTESIAN_POINT('Ctrl Pts',(1.74322663116028,0.972860235438245,17.1864225992283));
#14700=CARTESIAN_POINT('Ctrl Pts',(1.70324107813413,1.0412815395203,17.1919458046493));
#14701=CARTESIAN_POINT('Ctrl Pts',(1.64187964560899,1.13324447116701,17.1994676687122));
#14702=CARTESIAN_POINT('Ctrl Pts',(1.62385259757086,1.15892828729962,17.201579440419));
#14703=CARTESIAN_POINT('Ctrl Pts',(1.5945464757368,1.19865455301218,17.2048507223536));
#14704=CARTESIAN_POINT('Ctrl Pts',(1.58367097175322,1.2129870196339,17.2060319681563));
#14705=CARTESIAN_POINT('Ctrl Pts',(1.56955484254393,1.23107664328562,17.207522138583));
#14706=CARTESIAN_POINT('Ctrl Pts',(1.56649251216811,1.23497097779534,17.2078428982823));
#14707=CARTESIAN_POINT('Ctrl Pts',(1.5615567591525,1.24119982649268,17.2083558156659));
#14708=CARTESIAN_POINT('Ctrl Pts',(1.55969255993737,1.24354157152334,17.2085486189048));
#14709=CARTESIAN_POINT('Ctrl Pts',(1.55612570656695,1.24800149574357,17.2089157488679));
#14710=CARTESIAN_POINT('Ctrl Pts',(1.55442401550327,1.25012036545342,17.2090901369908));
#14711=CARTESIAN_POINT('Ctrl Pts',(1.55048800687116,1.25500084515398,17.209491751099));
#14712=CARTESIAN_POINT('Ctrl Pts',(1.54825063974357,1.25775996827669,17.2097187546575));
#14713=CARTESIAN_POINT('Ctrl Pts',(1.54105754683689,1.26658221993967,17.2104445066029));
#14714=CARTESIAN_POINT('Ctrl Pts',(1.53607340755764,1.27262224323984,17.2109412477218));
#14715=CARTESIAN_POINT('Ctrl Pts',(1.47564383043641,1.344981503694,17.2168927474639));
#14716=CARTESIAN_POINT('Ctrl Pts',(1.41597160064059,1.40766775509536,17.2220559096054));
#14717=CARTESIAN_POINT('Ctrl Pts',(1.22623957411825,1.58266429463629,17.2371968185742));
#14718=CARTESIAN_POINT('Ctrl Pts',(1.08558352783285,1.68225970412614,17.2469054006261));
#14719=CARTESIAN_POINT('Ctrl Pts',(0.89557424447002,1.78293490792719,17.2599707501284));
#14720=CARTESIAN_POINT('Ctrl Pts',(0.856584877135238,1.80199112775066,17.2626447013052));
#14721=CARTESIAN_POINT('Ctrl Pts',(0.80809841153772,1.82375982176157,17.2659752072149));
#14722=CARTESIAN_POINT('Ctrl Pts',(0.799160343714983,1.82769408539495,17.2665893522579));
#14723=CARTESIAN_POINT('Ctrl Pts',(0.785078933710558,1.83376925011825,17.2675573561786));
#14724=CARTESIAN_POINT('Ctrl Pts',(0.779954815427775,1.83595454183938,17.2679096989869));
#14725=CARTESIAN_POINT('Ctrl Pts',(0.770836431191546,1.83979821254026,17.2685368881432));
#14726=CARTESIAN_POINT('Ctrl Pts',(0.766845783110801,1.84146512618626,17.2688114422993));
#14727=CARTESIAN_POINT('Ctrl Pts',(0.757619946758024,1.84528361376427,17.2694463416233));
#14728=CARTESIAN_POINT('Ctrl Pts',(0.752380978013727,1.84742590156835,17.2698069986207));
#14729=CARTESIAN_POINT('Ctrl Pts',(0.737953680735875,1.85325387821658,17.2708005710434));
#14730=CARTESIAN_POINT('Ctrl Pts',(0.72874701791864,1.85689346760762,17.2714350337709));
#14731=CARTESIAN_POINT('Ctrl Pts',(0.703863442471546,1.86651691227008,17.2731511598997));
#14732=CARTESIAN_POINT('Ctrl Pts',(0.688137769142466,1.87237162750896,17.2742371022593));
#14733=CARTESIAN_POINT('Ctrl Pts',(0.521498476140861,1.93202909694234,17.2857616622243));
#14734=CARTESIAN_POINT('Ctrl Pts',(0.364729055316256,1.96765077856525,17.2968236595056));
#14735=CARTESIAN_POINT('Ctrl Pts',(0.126474170586867,1.99231828461863,17.3135360253376));
#14736=CARTESIAN_POINT('Ctrl Pts',(0.0471001584396288,1.99577321602486,
17.3190736188889));
#14737=CARTESIAN_POINT('Ctrl Pts',(-0.0636875971098499,1.99398060404727,
17.3266126631736));
#14738=CARTESIAN_POINT('Ctrl Pts',(-0.0950886864389171,1.99273007043515,
17.3287276943776));
#14739=CARTESIAN_POINT('Ctrl Pts',(-0.144422003463991,1.98959648773868,
17.3320034596387));
#14740=CARTESIAN_POINT('Ctrl Pts',(-0.162379633226104,1.98821146003813,
17.3331859978699));
#14741=CARTESIAN_POINT('Ctrl Pts',(-0.185252458312706,1.986135355567,17.3346775565301));
#14742=CARTESIAN_POINT('Ctrl Pts',(-0.190186496529454,1.98566896076926,
17.3349984384976));
#14743=CARTESIAN_POINT('Ctrl Pts',(-0.198098004156083,1.98489135838566,
17.3355115048271));
#14744=CARTESIAN_POINT('Ctrl Pts',(-0.201076560368469,1.98459183234377,
17.3357043353986));
#14745=CARTESIAN_POINT('Ctrl Pts',(-0.206757705118685,1.98400761054813,
17.3360714848802));
#14746=CARTESIAN_POINT('Ctrl Pts',(-0.20946035300823,1.98372410075963,17.3362458653217));
#14747=CARTESIAN_POINT('Ctrl Pts',(-0.215693700460661,1.98305733715093,
17.3366474186275));
#14748=CARTESIAN_POINT('Ctrl Pts',(-0.219223960627447,1.98267017691049,
17.3368743692849));
#14749=CARTESIAN_POINT('Ctrl Pts',(-0.230530440077363,1.98139963862068,
17.3375997817186));
#14750=CARTESIAN_POINT('Ctrl Pts',(-0.238302622397368,1.98047991071433,
17.338096238868));
#14751=CARTESIAN_POINT('Ctrl Pts',(-0.331048132189682,1.96895090834338,
17.3439963553587));
#14752=CARTESIAN_POINT('Ctrl Pts',(-0.415270758554667,1.9529246701269,17.3491139004739));
#14753=CARTESIAN_POINT('Ctrl Pts',(-0.593622913615264,1.90692113303631,
17.3599225081251));
#14754=CARTESIAN_POINT('Ctrl Pts',(-0.687079757781419,1.87527557139098,
17.3655728624317));
#14755=CARTESIAN_POINT('Ctrl Pts',(-0.871734246862315,1.79708349037046,
17.3772962555882));
#14756=CARTESIAN_POINT('Ctrl Pts',(-0.962451576591365,1.75017503768663,
17.3833618547817));
#14757=CARTESIAN_POINT('Ctrl Pts',(-1.0660925151378,1.68608119888674,17.3909134006739));
#14758=CARTESIAN_POINT('Ctrl Pts',(-1.08284870152087,1.67536912495483,17.3921545956018));
#14759=CARTESIAN_POINT('Ctrl Pts',(-1.10562337586787,1.66032508996702,17.3938709641429));
#14760=CARTESIAN_POINT('Ctrl Pts',(-1.1117824178352,1.65620720522415,17.3943381246782));
#14761=CARTESIAN_POINT('Ctrl Pts',(-1.12210303833124,1.64922341256424,17.3951260641116));
#14762=CARTESIAN_POINT('Ctrl Pts',(-1.12627696042839,1.64637580789518,17.3954461494356));
#14763=CARTESIAN_POINT('Ctrl Pts',(-1.13449141994371,1.64072574189826,17.3960789279609));
#14764=CARTESIAN_POINT('Ctrl Pts',(-1.13853250469233,1.63792413655212,17.3963915870803));
#14765=CARTESIAN_POINT('Ctrl Pts',(-1.14739454843415,1.63173161169286,17.3970802748918));
#14766=CARTESIAN_POINT('Ctrl Pts',(-1.1522109069493,1.6283342184722,17.3974565497375));
#14767=CARTESIAN_POINT('Ctrl Pts',(-1.16891808618526,1.61643796432891,17.3987687715272));
#14768=CARTESIAN_POINT('Ctrl Pts',(-1.18073027044309,1.60782996435622,17.3997089146109));
#14769=CARTESIAN_POINT('Ctrl Pts',(-1.19992253414018,1.59351825975766,17.4012572071185));
#14770=CARTESIAN_POINT('Ctrl Pts',(-1.20735923560672,1.58789111824626,17.4018623476765));
#14771=CARTESIAN_POINT('Ctrl Pts',(-1.34300538959531,1.48374769037878,17.4129967260343));
#14772=CARTESIAN_POINT('Ctrl Pts',(-1.45878229483117,1.37007450571178,17.4241665843122));
#14773=CARTESIAN_POINT('Ctrl Pts',(-1.60840435151322,1.18245579487212,17.4409099962785));
#14774=CARTESIAN_POINT('Ctrl Pts',(-1.65360603875303,1.11837141116755,17.4463739566062));
#14775=CARTESIAN_POINT('Ctrl Pts',(-1.71136239424292,1.02529918178006,17.4538250631175));
#14776=CARTESIAN_POINT('Ctrl Pts',(-1.72717976129861,0.998423736011658,
17.4559233984122));
#14777=CARTESIAN_POINT('Ctrl Pts',(-1.75108121923019,0.95554324262941,17.4591761890734));
#14778=CARTESIAN_POINT('Ctrl Pts',(-1.75959030918713,0.939782061866815,
17.4603520982517));
#14779=CARTESIAN_POINT('Ctrl Pts',(-1.77017730692112,0.919523969635986,
17.4618365347741));
#14780=CARTESIAN_POINT('Ctrl Pts',(-1.77245201322734,0.915131624824078,
17.4621567882204));
#14781=CARTESIAN_POINT('Ctrl Pts',(-1.77607615253173,0.90806938687654,17.4626690888841));
#14782=CARTESIAN_POINT('Ctrl Pts',(-1.77743594036857,0.905404875815389,
17.4628617789466));
#14783=CARTESIAN_POINT('Ctrl Pts',(-1.78001985731118,0.90031342232702,17.46322882833));
#14784=CARTESIAN_POINT('Ctrl Pts',(-1.78124500473685,0.897887066407594,
17.4634032484988));
#14785=CARTESIAN_POINT('Ctrl Pts',(-1.78406138964187,0.89228087701745,17.4638051154565));
#14786=CARTESIAN_POINT('Ctrl Pts',(-1.78564908670546,0.889099288678411,
17.4640323389037));
#14787=CARTESIAN_POINT('Ctrl Pts',(-1.79071443365552,0.878880534899564,
17.4647595031237));
#14788=CARTESIAN_POINT('Ctrl Pts',(-1.79415911046175,0.871826971808802,
17.4652574256228));
#14789=CARTESIAN_POINT('Ctrl Pts',(-1.83693772413718,0.782903076458022,
17.471486767677));
#14790=CARTESIAN_POINT('Ctrl Pts',(-1.87068274842977,0.698446964221641,
17.4768960059342));
#14791=CARTESIAN_POINT('Ctrl Pts',(-1.93624957873512,0.495035771416332,
17.4894088522375));
#14792=CARTESIAN_POINT('Ctrl Pts',(-1.96305815659874,0.374867614614655,
17.496423188457));
#14793=CARTESIAN_POINT('Ctrl Pts',(-1.98936136456924,0.169154535858712,
17.5086988579682));
#14794=CARTESIAN_POINT('Ctrl Pts',(-1.99474073223447,0.0847263743773186,
17.513807208732));
#14795=CARTESIAN_POINT('Ctrl Pts',(-1.99475112954771,-0.0102038292329521,
17.5197422069454));
#14796=CARTESIAN_POINT('Ctrl Pts',(-1.99467058830128,-0.0206258223393189,
17.5203962915775));
#14797=CARTESIAN_POINT('Ctrl Pts',(-1.99441052937542,-0.0373326610394684,
17.521449022418));
#14798=CARTESIAN_POINT('Ctrl Pts',(-1.99428296315399,-0.0436182148692334,
17.5218460427155));
#14799=CARTESIAN_POINT('Ctrl Pts',(-1.99400396827773,-0.0547668596103046,
17.5225519711169));
#14800=CARTESIAN_POINT('Ctrl Pts',(-1.99386445644917,-0.0596302191894833,
17.5228605036146));
#14801=CARTESIAN_POINT('Ctrl Pts',(-1.99353720496559,-0.0697467245359906,
17.523503537274));
#14802=CARTESIAN_POINT('Ctrl Pts',(-1.99334649089587,-0.0749997301784337,
17.5238381292959));
#14803=CARTESIAN_POINT('Ctrl Pts',(-1.99279910222661,-0.088594670650877,
17.5247058961218));
#14804=CARTESIAN_POINT('Ctrl Pts',(-1.99241081308839,-0.096935163261249,
17.5252400576319));
#14805=CARTESIAN_POINT('Ctrl Pts',(-1.99053186766449,-0.132488514316083,
17.5275248470496));
#14806=CARTESIAN_POINT('Ctrl Pts',(-1.98853601645113,-0.159670634361929,
17.5292912172278));
#14807=CARTESIAN_POINT('Ctrl Pts',(-1.98188607586114,-0.230369328634577,
17.5339389009797));
#14808=CARTESIAN_POINT('Ctrl Pts',(-1.97635593077795,-0.273786778155299,
17.5368464111109));
#14809=CARTESIAN_POINT('Ctrl Pts',(-1.94137661118417,-0.491110768626978,
17.5516684061906));
#14810=CARTESIAN_POINT('Ctrl Pts',(-1.89037955059374,-0.660744432216657,
17.5642028836821));
#14811=CARTESIAN_POINT('Ctrl Pts',(-1.79409452485747,-0.873818014964737,
17.580231626911));
#14812=CARTESIAN_POINT('Ctrl Pts',(-1.76816224768061,-0.92516850869737,
17.5841092770111));
#14813=CARTESIAN_POINT('Ctrl Pts',(-1.73679189510264,-0.981134921331046,
17.5882967221517));
#14814=CARTESIAN_POINT('Ctrl Pts',(-1.7335100010753,-0.986921932040363,
17.5887292261407));
#14815=CARTESIAN_POINT('Ctrl Pts',(-1.72850362256902,-0.995647727566108,
17.5893805068171));
#14816=CARTESIAN_POINT('Ctrl Pts',(-1.72680050019734,-0.998598619857602,
17.5896006076347));
#14817=CARTESIAN_POINT('Ctrl Pts',(-1.7238256822776,-1.00372253067246,17.5899825094721));
#14818=CARTESIAN_POINT('Ctrl Pts',(-1.72255742440441,-1.00589752025858,
17.5901445305578));
#14819=CARTESIAN_POINT('Ctrl Pts',(-1.71987736205356,-1.01047374085955,
17.5904852309469));
#14820=CARTESIAN_POINT('Ctrl Pts',(-1.71846464118588,-1.01287442391382,
17.59066384791));
#14821=CARTESIAN_POINT('Ctrl Pts',(-1.71501104082833,-1.0187152161917,17.5910981585293));
#14822=CARTESIAN_POINT('Ctrl Pts',(-1.71296481972022,-1.02215218482433,
17.5913535055847));
#14823=CARTESIAN_POINT('Ctrl Pts',(-1.70565533308627,-1.03434608903644,
17.5922587464883));
#14824=CARTESIAN_POINT('Ctrl Pts',(-1.70033503249705,-1.04306890234821,
17.5929050231705));
#14825=CARTESIAN_POINT('Ctrl Pts',(-1.66843616127588,-1.09447549839847,
17.5967085247111));
#14826=CARTESIAN_POINT('Ctrl Pts',(-1.64031599907426,-1.13618669424728,
17.5997733019453));
#14827=CARTESIAN_POINT('Ctrl Pts',(-1.55172863609338,-1.25743386831411,
17.6087578006898));
#14828=CARTESIAN_POINT('Ctrl Pts',(-1.48683394121714,-1.33354003546741,
17.6145054875879));
#14829=CARTESIAN_POINT('Ctrl Pts',(-1.31605458674032,-1.50578331778779,
17.6285860865113));
#14830=CARTESIAN_POINT('Ctrl Pts',(-1.20503863752363,-1.59601271191814,
17.6369558075612));
#14831=CARTESIAN_POINT('Ctrl Pts',(-1.07456229653539,-1.68062756600788,
17.6466635514261));
#14832=CARTESIAN_POINT('Ctrl Pts',(-1.06369866054543,-1.68752430855239,
17.6474705974339));
#14833=CARTESIAN_POINT('Ctrl Pts',(-1.04748760312937,-1.69759711053858,
17.648673415891));
#14834=CARTESIAN_POINT('Ctrl Pts',(-1.04219068212773,-1.70085414103689,
17.6490662014147));
#14835=CARTESIAN_POINT('Ctrl Pts',(-1.03274280632244,-1.70660285267582,
17.6497664233492));
#14836=CARTESIAN_POINT('Ctrl Pts',(-1.02859782792752,-1.70910430005826,
17.6500734988373));
#14837=CARTESIAN_POINT('Ctrl Pts',(-1.01986088364867,-1.71433365130621,
17.6507205199001));
#14838=CARTESIAN_POINT('Ctrl Pts',(-1.0152669918736,-1.71705824720494,17.6510605829325));
#14839=CARTESIAN_POINT('Ctrl Pts',(-1.00313538206474,-1.72418768917835,
17.6519582871014));
#14840=CARTESIAN_POINT('Ctrl Pts',(-0.995579657592115,-1.72856151861411,
17.6525170466032));
#14841=CARTESIAN_POINT('Ctrl Pts',(-0.961174407214186,-1.7481774907725,
17.6550600433646));
#14842=CARTESIAN_POINT('Ctrl Pts',(-0.934003178637936,-1.76284391394069,
17.6570647823076));
#14843=CARTESIAN_POINT('Ctrl Pts',(-0.860300077091477,-1.80044487332619,
17.6624967453241));
#14844=CARTESIAN_POINT('Ctrl Pts',(-0.813198285158574,-1.82220353790668,
17.6659624833597));
#14845=CARTESIAN_POINT('Ctrl Pts',(-0.671797713720952,-1.88094876611135,
17.6763452783997));
#14846=CARTESIAN_POINT('Ctrl Pts',(-0.575475070755421,-1.91261746519453,
17.6833990402685));
#14847=CARTESIAN_POINT('Ctrl Pts',(-0.415910801236494,-1.9519289927508,
17.6948642796277));
#14848=CARTESIAN_POINT('Ctrl Pts',(-0.353963276914826,-1.96410773646576,
17.6992610176573));
#14849=CARTESIAN_POINT('Ctrl Pts',(-0.235304746832726,-1.98163839802535,
17.7074804977728));
#14850=CARTESIAN_POINT('Ctrl Pts',(-0.178733139937995,-1.98753991260297,
17.7113130376734));
#14851=CARTESIAN_POINT('Ctrl Pts',(-0.114628371203731,-1.99146733977011,
17.7155046723049));
#14852=CARTESIAN_POINT('Ctrl Pts',(-0.107273008347744,-1.99187708823847,
17.715983369167));
#14853=CARTESIAN_POINT('Ctrl Pts',(-0.0964549146075904,-1.99241963879861,
17.7166839521736));
#14854=CARTESIAN_POINT('Ctrl Pts',(-0.0929939444592117,-1.99258417497532,
17.7169075632708));
#14855=CARTESIAN_POINT('Ctrl Pts',(-0.0868296987374572,-1.99286113062781,
17.7173048800954));
#14856=CARTESIAN_POINT('Ctrl Pts',(-0.0841266077297025,-1.9929770688,17.7174787815254));
#14857=CARTESIAN_POINT('Ctrl Pts',(-0.0783853087056505,-1.99321161704227,
17.7178474446986));
#14858=CARTESIAN_POINT('Ctrl Pts',(-0.0753470721161254,-1.99332878019652,
17.7180421241848));
#14859=CARTESIAN_POINT('Ctrl Pts',(-0.0671458204932518,-1.99362626642608,
17.7185665446482));
#14860=CARTESIAN_POINT('Ctrl Pts',(-0.0619823089349076,-1.99379348133345,
17.7188955576537));
#14861=CARTESIAN_POINT('Ctrl Pts',(-0.0365014481755044,-1.99451956866293,
17.720513690727));
#14862=CARTESIAN_POINT('Ctrl Pts',(-0.0161761367286923,-1.99478797769539,
17.7217872461601));
#14863=CARTESIAN_POINT('Ctrl Pts',(0.0414048321838454,-1.99466816312559,
17.7253554920779));
#14864=CARTESIAN_POINT('Ctrl Pts',(0.0786519580405387,-1.99354700656881,
17.7276166428052));
#14865=CARTESIAN_POINT('Ctrl Pts',(0.214982634216695,-1.98561601142922,
17.7357905447983));
#14866=CARTESIAN_POINT('Ctrl Pts',(0.313554358590365,-1.97245396449799,
17.7415075736065));
#14867=CARTESIAN_POINT('Ctrl Pts',(0.551441419672148,-1.92239774847684,
17.7556177643597));
#14868=CARTESIAN_POINT('Ctrl Pts',(0.68850604270232,-1.87767188310536,17.7640476713814));
#14869=CARTESIAN_POINT('Ctrl Pts',(0.831279855749553,-1.81333021871249,
17.7738237125587));
#14870=CARTESIAN_POINT('Ctrl Pts',(0.84294350953833,-1.80793775005939,17.7746296383553));
#14871=CARTESIAN_POINT('Ctrl Pts',(0.860169522359573,-1.7997707012786,17.7758311054142));
#14872=CARTESIAN_POINT('Ctrl Pts',(0.865772483585711,-1.79708213213058,
17.7762236696229));
#14873=CARTESIAN_POINT('Ctrl Pts',(0.875717318770753,-1.79225282092793,
17.7769236428986));
#14874=CARTESIAN_POINT('Ctrl Pts',(0.880064155110382,-1.79012236417851,
17.7772306919798));
#14875=CARTESIAN_POINT('Ctrl Pts',(0.889192297766664,-1.78560722656828,
17.7778778069346));
#14876=CARTESIAN_POINT('Ctrl Pts',(0.893971857424668,-1.78321911923274,
17.7782179908361));
#14877=CARTESIAN_POINT('Ctrl Pts',(0.906543280636337,-1.77687456208028,
17.7791163556581));
#14878=CARTESIAN_POINT('Ctrl Pts',(0.914318771834836,-1.77288609574165,
17.7796756579206));
#14879=CARTESIAN_POINT('Ctrl Pts',(0.9495207173819,-1.75453596017913,17.7822246746493));
#14880=CARTESIAN_POINT('Ctrl Pts',(0.976635479038798,-1.73958874169027,
17.7842350098196));
#14881=CARTESIAN_POINT('Ctrl Pts',(1.04838971400838,-1.69782727066911,17.7896858557162));
#14882=CARTESIAN_POINT('Ctrl Pts',(1.09234295313662,-1.66988757639833,17.7931652104746));
#14883=CARTESIAN_POINT('Ctrl Pts',(1.21854033942849,-1.58255219291744,17.8035735862334));
#14884=CARTESIAN_POINT('Ctrl Pts',(1.29740169037872,-1.51857089226017,17.8106392277323));
#14885=CARTESIAN_POINT('Ctrl Pts',(1.45758196066959,-1.36699489872244,17.8260246992894));
#14886=CARTESIAN_POINT('Ctrl Pts',(1.53661544819668,-1.27751332608872,17.8343191784467));
#14887=CARTESIAN_POINT('Ctrl Pts',(1.611717276486,-1.17535239138241,17.8425984509952));
#14888=CARTESIAN_POINT('Ctrl Pts',(1.61620302575589,-1.16917646544714,17.843094622018));
#14889=CARTESIAN_POINT('Ctrl Pts',(1.62270281643937,-1.16011873950325,17.8438158271586));
#14890=CARTESIAN_POINT('Ctrl Pts',(1.62474479742218,-1.15725721598166,17.8440427324922));
#14891=CARTESIAN_POINT('Ctrl Pts',(1.62834884940332,-1.15217834710361,17.8444437818181));
#14892=CARTESIAN_POINT('Ctrl Pts',(1.62991397407453,-1.14996319782766,17.8446181350349));
#14893=CARTESIAN_POINT('Ctrl Pts',(1.63320775995145,-1.14528120938414,17.8449854551085));
#14894=CARTESIAN_POINT('Ctrl Pts',(1.63493534860058,-1.14281365144335,17.8451783485868));
#14895=CARTESIAN_POINT('Ctrl Pts',(1.6395381995543,-1.13620748526903,17.8456929347163));
#14896=CARTESIAN_POINT('Ctrl Pts',(1.64240340316338,-1.13206184459615,17.8460139456953));
#14897=CARTESIAN_POINT('Ctrl Pts',(1.65593668933284,-1.11232111135646,17.8475337048314));
#14898=CARTESIAN_POINT('Ctrl Pts',(1.66639898381683,-1.09658518305492,17.8487190755787));
#14899=CARTESIAN_POINT('Ctrl Pts',(1.69484032405585,-1.05246036571681,17.8519782565764));
#14900=CARTESIAN_POINT('Ctrl Pts',(1.71232872503927,-1.02376127829014,17.854025130412));
#14901=CARTESIAN_POINT('Ctrl Pts',(1.77317573400123,-0.917983873852684,
17.8613598709024));
#14902=CARTESIAN_POINT('Ctrl Pts',(1.81212444557359,-0.838482987201785,
17.8664821872471));
#14903=CARTESIAN_POINT('Ctrl Pts',(1.90162104155844,-0.620178429027883,
17.8801656359342));
#14904=CARTESIAN_POINT('Ctrl Pts',(1.94225469961493,-0.477936660902421,
17.8887286315749));
#14905=CARTESIAN_POINT('Ctrl Pts',(1.96915135884961,-0.318846230820188,
17.8987097158277));
#14906=CARTESIAN_POINT('Ctrl Pts',(1.97132101712113,-0.305144925284576,
17.8995720979636));
#14907=CARTESIAN_POINT('Ctrl Pts',(1.97492179246937,-0.280762509787471,
17.9011122847096));
#14908=CARTESIAN_POINT('Ctrl Pts',(1.97640960494237,-0.270090243249286,
17.9017883000064));
#14909=CARTESIAN_POINT('Ctrl Pts',(1.97864189725565,-0.253070430387111,
17.9028695768465));
#14910=CARTESIAN_POINT('Ctrl Pts',(1.9794424798818,-0.24673035404821,17.9032730676696));
#14911=CARTESIAN_POINT('Ctrl Pts',(1.98080088518131,-0.235540332380596,
17.9039864979108));
#14912=CARTESIAN_POINT('Ctrl Pts',(1.98137139752668,-0.230691957558923,
17.9042960345878));
#14913=CARTESIAN_POINT('Ctrl Pts',(1.98251421188178,-0.220662930169388,
17.9049372190628));
#14914=CARTESIAN_POINT('Ctrl Pts',(1.98308401747772,-0.21548203600036,17.905268943024));
#14915=CARTESIAN_POINT('Ctrl Pts',(1.98449261329214,-0.202195535615407,
17.9061209517925));
#14916=CARTESIAN_POINT('Ctrl Pts',(1.98530204484354,-0.194086976139843,
17.906642156468));
#14917=CARTESIAN_POINT('Ctrl Pts',(1.98844004289059,-0.160575489641808,
17.9088014811636));
#14918=CARTESIAN_POINT('Ctrl Pts',(1.99033081098259,-0.13513494905966,17.9104532723644));
#14919=CARTESIAN_POINT('Ctrl Pts',(2.00178117421162,0.0728242028844208,
17.9240642447832));
#14920=CARTESIAN_POINT('Ctrl Pts',(1.98669830232853,0.255798641183532,17.9368416232503));
#14921=CARTESIAN_POINT('Ctrl Pts',(1.92596965389718,0.528160805176158,17.956257947305));
#14922=CARTESIAN_POINT('Ctrl Pts',(1.89820864899906,0.62058175034428,17.9628942795221));
#14923=CARTESIAN_POINT('Ctrl Pts',(1.86107220839135,0.717982935641215,17.9697034669122));
#14924=CARTESIAN_POINT('Ctrl Pts',(1.85823049033752,0.725305942665645,17.9702142075742));
#14925=CARTESIAN_POINT('Ctrl Pts',(1.85403927112303,0.73592023589072,17.9709525509397));
#14926=CARTESIAN_POINT('Ctrl Pts',(1.85272415162696,0.739224885213897,17.9711821510295));
#14927=CARTESIAN_POINT('Ctrl Pts',(1.85038834141296,0.745048949678202,17.9715862858542));
#14928=CARTESIAN_POINT('Ctrl Pts',(1.84937133110063,0.747569817153153,17.9717610408681));
#14929=CARTESIAN_POINT('Ctrl Pts',(1.84722447603255,0.752860042249826,17.9721274134368));
#14930=CARTESIAN_POINT('Ctrl Pts',(1.84609355743296,0.755628933778719,17.972318964466));
#14931=CARTESIAN_POINT('Ctrl Pts',(1.8430766590256,0.76296817505723,17.972826166518));
#14932=CARTESIAN_POINT('Ctrl Pts',(1.84117989257265,0.767534111061243,17.9731411698098));
#14933=CARTESIAN_POINT('Ctrl Pts',(1.83234257732728,0.788586205315364,17.9745912615566));
#14934=CARTESIAN_POINT('Ctrl Pts',(1.82519718194176,0.804986226480913,17.9757144150661));
#14935=CARTESIAN_POINT('Ctrl Pts',(1.8050171960147,0.84965240281804,17.9787613756287));
#14936=CARTESIAN_POINT('Ctrl Pts',(1.79153971137327,0.877714058296531,17.9806623213574));
#14937=CARTESIAN_POINT('Ctrl Pts',(1.74195088544175,0.975057538678526,17.9872486740085));
#14938=CARTESIAN_POINT('Ctrl Pts',(1.70243057531053,1.04252670875458,17.9918012209703));
#14939=CARTESIAN_POINT('Ctrl Pts',(1.56910509468137,1.24224892322164,18.0057420815429));
#14940=CARTESIAN_POINT('Ctrl Pts',(1.46309232466983,1.36551339394418,18.0150752526007));
#14941=CARTESIAN_POINT('Ctrl Pts',(1.33791686616869,1.47954722867949,18.0255538278731));
#14942=CARTESIAN_POINT('Ctrl Pts',(1.33245834169282,1.48446499053168,18.0260096848435));
#14943=CARTESIAN_POINT('Ctrl Pts',(1.31529664735945,1.4997555970717,18.0274396952075));
#14944=CARTESIAN_POINT('Ctrl Pts',(1.30349880461244,1.51002084948233,18.0284181356453));
#14945=CARTESIAN_POINT('Ctrl Pts',(1.28683674490259,1.52417765464905,18.0297941819199));
#14946=CARTESIAN_POINT('Ctrl Pts',(1.28207293965561,1.52818693455425,18.0301869514299));
#14947=CARTESIAN_POINT('Ctrl Pts',(1.27379388902218,1.53508873155506,18.0308684641422));
#14948=CARTESIAN_POINT('Ctrl Pts',(1.27028734913369,1.53799165652066,18.0311567810533));
#14949=CARTESIAN_POINT('Ctrl Pts',(1.26298564499185,1.54399444149703,18.0317564733145));
#14950=CARTESIAN_POINT('Ctrl Pts',(1.25918893733225,1.54709236770938,18.0320679241215));
#14951=CARTESIAN_POINT('Ctrl Pts',(1.25024065340345,1.55433896599792,18.032801113714));
#14952=CARTESIAN_POINT('Ctrl Pts',(1.24507980499479,1.55847604732731,18.0332233143362));
#14953=CARTESIAN_POINT('Ctrl Pts',(1.22842982330269,1.57168765297546,18.0345833789358));
#14954=CARTESIAN_POINT('Ctrl Pts',(1.21686154192868,1.58066121546026,18.0355252424823));
#14955=CARTESIAN_POINT('Ctrl Pts',(1.1894555371009,1.60144100016847,18.037749812225));
#14956=CARTESIAN_POINT('Ctrl Pts',(1.17353937596763,1.61314073730684,18.0390365497288));
#14957=CARTESIAN_POINT('Ctrl Pts',(1.11701216261136,1.65341372340212,18.0435894678087));
#14958=CARTESIAN_POINT('Ctrl Pts',(1.07551319030384,1.68070336478576,18.0469022662731));
#14959=CARTESIAN_POINT('Ctrl Pts',(0.890261898015245,1.79285218579264,18.0615596729402));
#14960=CARTESIAN_POINT('Ctrl Pts',(0.737220681768395,1.86101584780977,18.0734089144645));
#14961=CARTESIAN_POINT('Ctrl Pts',(0.522176223435725,1.92605801477154,18.0888128446357));
#14962=CARTESIAN_POINT('Ctrl Pts',(0.466151833800666,1.94037918660384,18.092711294495));
#14963=CARTESIAN_POINT('Ctrl Pts',(0.403060921556072,1.95361557407042,18.0969187568469));
#14964=CARTESIAN_POINT('Ctrl Pts',(0.396535932593443,1.95495042774208,18.0973517391718));
#14965=CARTESIAN_POINT('Ctrl Pts',(0.386661123960933,1.95691909862524,18.0980036164436));
#14966=CARTESIAN_POINT('Ctrl Pts',(0.383316244449521,1.95757703309735,18.0982238388772));
#14967=CARTESIAN_POINT('Ctrl Pts',(0.377497576830527,1.95870607373735,18.0986058925785));
#14968=CARTESIAN_POINT('Ctrl Pts',(0.375024566086652,1.95918107351359,18.0987679443388));
#14969=CARTESIAN_POINT('Ctrl Pts',(0.369814652292523,1.96017153373276,18.0991086441019));
#14970=CARTESIAN_POINT('Ctrl Pts',(0.367077560252191,1.96068594721808,18.0992872299656));
#14971=CARTESIAN_POINT('Ctrl Pts',(0.360409201347693,1.96192475633389,18.099721351188));
#14972=CARTESIAN_POINT('Ctrl Pts',(0.356476789919736,1.96264307525741,18.0999765406657));
#14973=CARTESIAN_POINT('Ctrl Pts',(0.34299298172454,1.96506424952078,18.1008488415164));
#14974=CARTESIAN_POINT('Ctrl Pts',(0.333431145975211,1.96670927446056,18.1014627547518));
#14975=CARTESIAN_POINT('Ctrl Pts',(0.209129848934509,1.98716155256814,18.10938743277));
#14976=CARTESIAN_POINT('Ctrl Pts',(0.0929525732555075,1.99597458098033,
18.116182060956));
#14977=CARTESIAN_POINT('Ctrl Pts',(-0.138400077857139,1.99326674061518,
18.1296202051874));
#14978=CARTESIAN_POINT('Ctrl Pts',(-0.253115249334878,1.98196814987794,
18.136244703859));
#14979=CARTESIAN_POINT('Ctrl Pts',(-0.384207628065902,1.95748489703089,
18.1442271810741));
#14980=CARTESIAN_POINT('Ctrl Pts',(-0.402153684666894,1.9538769178248,18.1453286872309));
#14981=CARTESIAN_POINT('Ctrl Pts',(-0.466371061604144,1.9400440887738,18.1493057247579));
#14982=CARTESIAN_POINT('Ctrl Pts',(-0.512321428374567,1.92841884129845,
18.1522183436847));
#14983=CARTESIAN_POINT('Ctrl Pts',(-0.566958277114803,1.91250532861324,
18.1557805492576));
#14984=CARTESIAN_POINT('Ctrl Pts',(-0.576085549471598,1.90977583883887,
18.1563789722728));
#14985=CARTESIAN_POINT('Ctrl Pts',(-0.591008859065501,1.90519634237726,
18.1573630471616));
#14986=CARTESIAN_POINT('Ctrl Pts',(-0.596816674890876,1.90338499251752,
18.1577474332588));
#14987=CARTESIAN_POINT('Ctrl Pts',(-0.607216636834413,1.90008915827409,
18.1584383104895));
#14988=CARTESIAN_POINT('Ctrl Pts',(-0.611811872166747,1.89861451744267,
18.1587444761764));
#14989=CARTESIAN_POINT('Ctrl Pts',(-0.621554167508126,1.89544911041258,
18.1593955086079));
#14990=CARTESIAN_POINT('Ctrl Pts',(-0.626699772984551,1.89375402491891,
18.1597405156441));
#14991=CARTESIAN_POINT('Ctrl Pts',(-0.639904040936078,1.88934451355837,
18.1606288385329));
#14992=CARTESIAN_POINT('Ctrl Pts',(-0.647952302676579,1.88659950234825,
18.1611731614578));
#14993=CARTESIAN_POINT('Ctrl Pts',(-0.685028985473981,1.87368856672921,
18.1636942353336));
#14994=CARTESIAN_POINT('Ctrl Pts',(-0.713836044586039,1.86290404524583,
18.1656914112461));
#14995=CARTESIAN_POINT('Ctrl Pts',(-0.790477493450411,1.83217305166076,
18.1711122870743));
#14996=CARTESIAN_POINT('Ctrl Pts',(-0.837800420342886,1.8110224837659,18.1745745543083));
#14997=CARTESIAN_POINT('Ctrl Pts',(-0.980441267375064,1.74048261193429,
18.1853645608122));
#14998=CARTESIAN_POINT('Ctrl Pts',(-1.07263587421954,1.68522795846736,18.1928532071582));
#14999=CARTESIAN_POINT('Ctrl Pts',(-1.1742396242555,1.61260603314266,18.2015635994442));
#15000=CARTESIAN_POINT('Ctrl Pts',(-1.18841287730972,1.60218967471311,18.2027894499162));
#15001=CARTESIAN_POINT('Ctrl Pts',(-1.27876441131116,1.53392894978689,18.2106674030049));
#15002=CARTESIAN_POINT('Ctrl Pts',(-1.3508467609082,1.47084813557862,18.2172524367816));
#15003=CARTESIAN_POINT('Ctrl Pts',(-1.42365569877746,1.39724504897519,18.2240152465508));
#15004=CARTESIAN_POINT('Ctrl Pts',(-1.4291474241504,1.39162743597586,18.2245260491834));
#15005=CARTESIAN_POINT('Ctrl Pts',(-1.43707727433885,1.38341935842972,18.2252644653367));
#15006=CARTESIAN_POINT('Ctrl Pts',(-1.43954179741868,1.38085467289842,18.2254940767887));
#15007=CARTESIAN_POINT('Ctrl Pts',(-1.44387768747441,1.37631834079527,18.2258982246797));
#15008=CARTESIAN_POINT('Ctrl Pts',(-1.44575189999769,1.37434944450483,18.2260729814441));
#15009=CARTESIAN_POINT('Ctrl Pts',(-1.44967978616557,1.37020619803607,18.226439350284));
#15010=CARTESIAN_POINT('Ctrl Pts',(-1.4517325915474,1.3680310634198,18.2266308958619));
#15011=CARTESIAN_POINT('Ctrl Pts',(-1.45590621420345,1.36358875606364,18.2270205021071));
#15012=CARTESIAN_POINT('Ctrl Pts',(-1.4580266473514,1.36132123179924,18.2272185333485));
#15013=CARTESIAN_POINT('Ctrl Pts',(-1.46705017737417,1.35162648512567,18.2280616889004));
#15014=CARTESIAN_POINT('Ctrl Pts',(-1.4739020388927,1.34415146777639,18.2287030051971));
#15015=CARTESIAN_POINT('Ctrl Pts',(-1.55687066987215,1.2522397910728,18.2364867635286));
#15016=CARTESIAN_POINT('Ctrl Pts',(-1.62570380758713,1.16148429945965,18.2431385889086));
#15017=CARTESIAN_POINT('Ctrl Pts',(-1.71020089168383,1.02772587400507,18.2523307904085));
#15018=CARTESIAN_POINT('Ctrl Pts',(-1.73270026685849,0.989321661939559,
18.2549055760555));
#15019=CARTESIAN_POINT('Ctrl Pts',(-1.77380303863056,0.913453192944326,
18.2599207781885));
#15020=CARTESIAN_POINT('Ctrl Pts',(-1.79254955189127,0.876093548689596,
18.2623585408199));
#15021=CARTESIAN_POINT('Ctrl Pts',(-1.84921892711085,0.753711122927371,
18.2703029728698));
#15022=CARTESIAN_POINT('Ctrl Pts',(-1.88236494324017,0.66662571498682,18.2759001242718));
#15023=CARTESIAN_POINT('Ctrl Pts',(-1.91296499328664,0.565466124660871,
18.2824994027861));
#15024=CARTESIAN_POINT('Ctrl Pts',(-1.91650605563652,0.553345760534934,
18.2832914942293));
#15025=CARTESIAN_POINT('Ctrl Pts',(-1.92160590407678,0.53525357473922,18.2844762595219));
#15026=CARTESIAN_POINT('Ctrl Pts',(-1.92325248021467,0.529306655740876,
18.2848660769413));
#15027=CARTESIAN_POINT('Ctrl Pts',(-1.92614010744719,0.518686062869001,
18.2855629745102));
#15028=CARTESIAN_POINT('Ctrl Pts',(-1.92739181273776,0.514015315771662,
18.2858697062904));
#15029=CARTESIAN_POINT('Ctrl Pts',(-1.92999688028532,0.50415117514907,18.2865180372963));
#15030=CARTESIAN_POINT('Ctrl Pts',(-1.93134628943714,0.498956786369663,
18.2868597617611));
#15031=CARTESIAN_POINT('Ctrl Pts',(-1.93404534686989,0.488392076524176,
18.2875554548888));
#15032=CARTESIAN_POINT('Ctrl Pts',(-1.93539362779187,0.483021457741381,
18.2879094644375));
#15033=CARTESIAN_POINT('Ctrl Pts',(-1.93868125589117,0.469691036640193,
18.2887890514043));
#15034=CARTESIAN_POINT('Ctrl Pts',(-1.94059394643289,0.461724824523402,
18.2893154828785));
#15035=CARTESIAN_POINT('Ctrl Pts',(-1.9495551985194,0.423362377373257,18.2918545668947));
#15036=CARTESIAN_POINT('Ctrl Pts',(-1.95593864292376,0.392816772766463,
18.2938883596265));
#15037=CARTESIAN_POINT('Ctrl Pts',(-1.98377043023989,0.24205848726371,18.3039906943939));
#15038=CARTESIAN_POINT('Ctrl Pts',(-1.99486174487414,0.120222297344481,
18.3123781448069));
#15039=CARTESIAN_POINT('Ctrl Pts',(-1.99474915136337,-0.00184000954739135,
18.3208813519367));
#15040=CARTESIAN_POINT('',(-1.99474949800079,0.00141517687806603,19.9197876209294));
#15041=CARTESIAN_POINT('Ctrl Pts',(-1.99474915155247,-0.00183980452437414,
18.3208813376543));
#15042=CARTESIAN_POINT('Ctrl Pts',(-1.99462759758103,-0.133630806333513,
18.3300622732238));
#15043=CARTESIAN_POINT('Ctrl Pts',(-1.98144557580629,-0.265099424167756,
18.3393350990873));
#15044=CARTESIAN_POINT('Ctrl Pts',(-1.95303027127133,-0.406008020399977,
18.3488600952125));
#15045=CARTESIAN_POINT('Ctrl Pts',(-1.95056824805384,-0.417676045126906,
18.3496454702622));
#15046=CARTESIAN_POINT('Ctrl Pts',(-1.94671783721713,-0.435146879524617,
18.3508156982726));
#15047=CARTESIAN_POINT('Ctrl Pts',(-1.94540785890408,-0.440966449010872,
18.3512045451171));
#15048=CARTESIAN_POINT('Ctrl Pts',(-1.94325116638932,-0.450350852338331,
18.3518299391367));
#15049=CARTESIAN_POINT('Ctrl Pts',(-1.94242071351959,-0.453919329925472,
18.3520673643239));
#15050=CARTESIAN_POINT('Ctrl Pts',(-1.9408036719361,-0.460782096193919,
18.3525232041302));
#15051=CARTESIAN_POINT('Ctrl Pts',(-1.94001851664671,-0.464076705576403,
18.3527416981309));
#15052=CARTESIAN_POINT('Ctrl Pts',(-1.93865430829428,-0.469737126002959,
18.3531164837775));
#15053=CARTESIAN_POINT('Ctrl Pts',(-1.93807931141267,-0.472103884254078,
18.3532730076802));
#15054=CARTESIAN_POINT('Ctrl Pts',(-1.93686976583747,-0.47704307193831,
18.3535992715911));
#15055=CARTESIAN_POINT('Ctrl Pts',(-1.93623442909215,-0.479615281344062,
18.3537689648504));
#15056=CARTESIAN_POINT('Ctrl Pts',(-1.93445094247747,-0.486774560627539,
18.3542406900202));
#15057=CARTESIAN_POINT('Ctrl Pts',(-1.93329159467776,-0.491358863541545,
18.3545420801177));
#15058=CARTESIAN_POINT('Ctrl Pts',(-1.92856563578903,-0.509770602602811,
18.3557500056353));
#15059=CARTESIAN_POINT('Ctrl Pts',(-1.92486678470205,-0.52356410110425,
18.3566491905607));
#15060=CARTESIAN_POINT('Ctrl Pts',(-1.88703482460906,-0.658821185222753,
18.3654205065383));
#15061=CARTESIAN_POINT('Ctrl Pts',(-1.84159328818003,-0.776845797463386,
18.3727194278233));
#15062=CARTESIAN_POINT('Ctrl Pts',(-1.75721826554491,-0.946136273270623,
18.3836897187713));
#15063=CARTESIAN_POINT('Ctrl Pts',(-1.7264890648432,-1.00111192242871,18.3873370462227));
#15064=CARTESIAN_POINT('Ctrl Pts',(-1.64525246181721,-1.13154859111573,
18.3963680846301));
#15065=CARTESIAN_POINT('Ctrl Pts',(-1.59210033830179,-1.20518517772239,
18.4018008303851));
#15066=CARTESIAN_POINT('Ctrl Pts',(-1.52279642022826,-1.28857785250226,
18.4085335397413));
#15067=CARTESIAN_POINT('Ctrl Pts',(-1.51128508331362,-1.30205959328525,
18.409641298453));
#15068=CARTESIAN_POINT('Ctrl Pts',(-1.49598190657535,-1.31950586718404,
18.4111011997342));
#15069=CARTESIAN_POINT('Ctrl Pts',(-1.49235100202034,-1.32361100181805,
18.4114466649023));
#15070=CARTESIAN_POINT('Ctrl Pts',(-1.48515745364468,-1.33167686767978,
18.4121293305835));
#15071=CARTESIAN_POINT('Ctrl Pts',(-1.48159576788444,-1.33563839482039,
18.4124664894086));
#15072=CARTESIAN_POINT('Ctrl Pts',(-1.47476481091289,-1.34317526255086,
18.4131115479566));
#15073=CARTESIAN_POINT('Ctrl Pts',(-1.4714982951989,-1.34675305827823,18.4134193297798));
#15074=CARTESIAN_POINT('Ctrl Pts',(-1.4639913983891,-1.35491540207385,18.4141251243271));
#15075=CARTESIAN_POINT('Ctrl Pts',(-1.45974247347117,-1.35949199005081,
18.4145234999533));
#15076=CARTESIAN_POINT('Ctrl Pts',(-1.44657950290927,-1.37353719239036,
18.4157543144724));
#15077=CARTESIAN_POINT('Ctrl Pts',(-1.43759444168374,-1.38293849647789,
18.4165898048474));
#15078=CARTESIAN_POINT('Ctrl Pts',(-1.34398372145361,-1.4789877113255,18.4252481752068));
#15079=CARTESIAN_POINT('Ctrl Pts',(-1.25174145564546,-1.55782877832362,
18.4334193699797));
#15080=CARTESIAN_POINT('Ctrl Pts',(-1.06112453288347,-1.69283801173296,
18.449576828833));
#15081=CARTESIAN_POINT('Ctrl Pts',(-0.963977295391744,-1.74998090385539,
18.4575021479227));
#15082=CARTESIAN_POINT('Ctrl Pts',(-0.823116780739672,-1.81753050532631,
18.4682428726371));
#15083=CARTESIAN_POINT('Ctrl Pts',(-0.78308818477667,-1.835132640282,18.4712149245023));
#15084=CARTESIAN_POINT('Ctrl Pts',(-0.728556700565041,-1.85700262098791,
18.4751292543194));
#15085=CARTESIAN_POINT('Ctrl Pts',(-0.714539233750911,-1.86244122441266,
18.4761237397397));
#15086=CARTESIAN_POINT('Ctrl Pts',(-0.690829082602297,-1.87133336609236,
18.4777846921561));
#15087=CARTESIAN_POINT('Ctrl Pts',(-0.681168963118902,-1.87487126039451,
18.4784555409911));
#15088=CARTESIAN_POINT('Ctrl Pts',(-0.668558285060478,-1.87937942424264,
18.479323280405));
#15089=CARTESIAN_POINT('Ctrl Pts',(-0.665632450961819,-1.88041767736137,
18.4795240478167));
#15090=CARTESIAN_POINT('Ctrl Pts',(-0.659883170213068,-1.88244275068446,
18.4799174437997));
#15091=CARTESIAN_POINT('Ctrl Pts',(-0.657059905421901,-1.88343005946907,
18.4801101006658));
#15092=CARTESIAN_POINT('Ctrl Pts',(-0.651666465467604,-1.88530256708706,
18.4804771264877));
#15093=CARTESIAN_POINT('Ctrl Pts',(-0.649096732927811,-1.88618885137734,
18.4806515561297));
#15094=CARTESIAN_POINT('Ctrl Pts',(-0.643160428001201,-1.88822267665594,
18.4810534975855));
#15095=CARTESIAN_POINT('Ctrl Pts',(-0.6397925933529,-1.88936646809299,18.4812807857879));
#15096=CARTESIAN_POINT('Ctrl Pts',(-0.628977134240288,-1.89300740337191,
18.4820083662368));
#15097=CARTESIAN_POINT('Ctrl Pts',(-0.621517696367855,-1.89546960477566,
18.4825066369598));
#15098=CARTESIAN_POINT('Ctrl Pts',(-0.525387535355053,-1.92657161611299,
18.4888847514072));
#15099=CARTESIAN_POINT('Ctrl Pts',(-0.434816930272576,-1.94901243781041,
18.4944253753076));
#15100=CARTESIAN_POINT('Ctrl Pts',(-0.21027536994351,-1.98820614528123,
18.5077581318166));
#15101=CARTESIAN_POINT('Ctrl Pts',(-0.0755524049126808,-1.99786659074581,
18.5154384625263));
#15102=CARTESIAN_POINT('Ctrl Pts',(0.126662429618491,-1.99187116151396,
18.5275039937355));
#15103=CARTESIAN_POINT('Ctrl Pts',(0.194056969051639,-1.98643764084671,
18.531610241012));
#15104=CARTESIAN_POINT('Ctrl Pts',(0.27405178554565,-1.9758783894734,18.5366447093487));
#15105=CARTESIAN_POINT('Ctrl Pts',(0.287044998068462,-1.97403266111248,
18.5374674574447));
#15106=CARTESIAN_POINT('Ctrl Pts',(0.306314494665547,-1.97110109986061,
18.5386954565545));
#15107=CARTESIAN_POINT('Ctrl Pts',(0.312605496657503,-1.97011317376604,
18.5390976094803));
#15108=CARTESIAN_POINT('Ctrl Pts',(0.323690580442947,-1.96831796335097,
18.5398084599857));
#15109=CARTESIAN_POINT('Ctrl Pts',(0.32848666697723,-1.96752324145114,18.5401167568242));
#15110=CARTESIAN_POINT('Ctrl Pts',(0.337837774769023,-1.9659385983518,18.5407193173927));
#15111=CARTESIAN_POINT('Ctrl Pts',(0.342393052775504,-1.96515035846332,
18.5410135258707));
#15112=CARTESIAN_POINT('Ctrl Pts',(0.354629517970881,-1.962989137315,18.541805679774));
#15113=CARTESIAN_POINT('Ctrl Pts',(0.362305396317866,-1.96158692011463,
18.5423045524556));
#15114=CARTESIAN_POINT('Ctrl Pts',(0.390477979158265,-1.9562693970089,18.5441428810597));
#15115=CARTESIAN_POINT('Ctrl Pts',(0.410920524660765,-1.95207768115321,
18.5454911058565));
#15116=CARTESIAN_POINT('Ctrl Pts',(0.591873008594086,-1.9120053452765,18.557556942262));
#15117=CARTESIAN_POINT('Ctrl Pts',(0.74740747747759,-1.85672787215594,18.5689313871662));
#15118=CARTESIAN_POINT('Ctrl Pts',(0.992589544051896,-1.73374452907766,
18.5880687800573));
#15119=CARTESIAN_POINT('Ctrl Pts',(1.08658917675904,-1.67643465144908,18.5957244228537));
#15120=CARTESIAN_POINT('Ctrl Pts',(1.18371060915936,-1.6056035139274,18.6036647499401));
#15121=CARTESIAN_POINT('Ctrl Pts',(1.19197776249049,-1.59947568730832,18.6043408114044));
#15122=CARTESIAN_POINT('Ctrl Pts',(1.20629689338689,-1.58868929738754,18.6055115501763));
#15123=CARTESIAN_POINT('Ctrl Pts',(1.21237014618414,-1.58405950388187,18.6060080275575));
#15124=CARTESIAN_POINT('Ctrl Pts',(1.2212638923656,-1.57719846496799,18.6067347807355));
#15125=CARTESIAN_POINT('Ctrl Pts',(1.2241050889327,-1.57499435695499,18.6069669047436));
#15126=CARTESIAN_POINT('Ctrl Pts',(1.22908104566906,-1.5711125730376,18.6073733357633));
#15127=CARTESIAN_POINT('Ctrl Pts',(1.23121835793159,-1.56943820822291,18.6075478755051));
#15128=CARTESIAN_POINT('Ctrl Pts',(1.23541540319,-1.56613640364816,18.6078905462941));
#15129=CARTESIAN_POINT('Ctrl Pts',(1.23747533378436,-1.56450926866605,18.60805869767));
#15130=CARTESIAN_POINT('Ctrl Pts',(1.24314126960825,-1.56001556612682,18.608521133273));
#15131=CARTESIAN_POINT('Ctrl Pts',(1.24674059525025,-1.5571405434131,18.6088148174071));
#15132=CARTESIAN_POINT('Ctrl Pts',(1.26075063719846,-1.5458700650061,18.6099577813468));
#15133=CARTESIAN_POINT('Ctrl Pts',(1.27108706906765,-1.53738222737988,18.6108006682163));
#15134=CARTESIAN_POINT('Ctrl Pts',(1.2834878210131,-1.52698868578518,18.6118125219571));
#15135=CARTESIAN_POINT('Ctrl Pts',(1.28563416903998,-1.52518202743319,18.6119876788632));
#15136=CARTESIAN_POINT('Ctrl Pts',(1.44891520787254,-1.38715291824462,18.6253149467192));
#15137=CARTESIAN_POINT('Ctrl Pts',(1.58744669100734,-1.22621130523688,18.6369208906312));
#15138=CARTESIAN_POINT('Ctrl Pts',(1.72509991501907,-1.00284082721485,18.6525133566531));
#15139=CARTESIAN_POINT('Ctrl Pts',(1.75031802548324,-0.95814698539679,18.65560332213));
#15140=CARTESIAN_POINT('Ctrl Pts',(1.78779610785187,-0.885297004582001,
18.6606316618557));
#15141=CARTESIAN_POINT('Ctrl Pts',(1.80117815393882,-0.857742856546517,
18.6625315733318));
#15142=CARTESIAN_POINT('Ctrl Pts',(1.81754202782522,-0.821975872103614,
18.6649999306644));
#15143=CARTESIAN_POINT('Ctrl Pts',(1.82111215065194,-0.81403555702936,18.6655480360842));
#15144=CARTESIAN_POINT('Ctrl Pts',(1.82678626980328,-0.80119158540571,18.6664349427594));
#15145=CARTESIAN_POINT('Ctrl Pts',(1.82892279605632,-0.79630235289724,18.6667726278791));
#15146=CARTESIAN_POINT('Ctrl Pts',(1.83296093642385,-0.786959477264073,
18.6674180766912));
#15147=CARTESIAN_POINT('Ctrl Pts',(1.83486600175896,-0.782507359851042,
18.6677257198896));
#15148=CARTESIAN_POINT('Ctrl Pts',(1.83918425599522,-0.772313168227375,
18.6684303254765));
#15149=CARTESIAN_POINT('Ctrl Pts',(1.84158679087301,-0.76656666216677,18.6688276464452));
#15150=CARTESIAN_POINT('Ctrl Pts',(1.84889038619227,-0.748865039447626,
18.6700520218467));
#15151=CARTESIAN_POINT('Ctrl Pts',(1.85370215796984,-0.736873668913815,
18.6708820816968));
#15152=CARTESIAN_POINT('Ctrl Pts',(1.89849001249891,-0.622042807307998,
18.6788383052211));
#15153=CARTESIAN_POINT('Ctrl Pts',(1.9299783331343,-0.51611797389255,18.6862507378249));
#15154=CARTESIAN_POINT('Ctrl Pts',(1.98774285460882,-0.239778097251125,
18.7057040007797));
#15155=CARTESIAN_POINT('Ctrl Pts',(2.00101247593706,-0.0675661981849562,
18.7179758740718));
#15156=CARTESIAN_POINT('Ctrl Pts',(1.99105329750384,0.122804526027687,18.7306176191976));
#15157=CARTESIAN_POINT('Ctrl Pts',(1.98982035192278,0.14138321626499,18.7318407105203));
#15158=CARTESIAN_POINT('Ctrl Pts',(1.98792540381359,0.164940256753106,18.7333757488135));
#15159=CARTESIAN_POINT('Ctrl Pts',(1.98750455287962,0.169936320523003,18.7337004019351));
#15160=CARTESIAN_POINT('Ctrl Pts',(1.98680121171316,0.177925676545154,18.7342180618197));
#15161=CARTESIAN_POINT('Ctrl Pts',(1.98653078677484,0.180919967745124,18.7344117351217));
#15162=CARTESIAN_POINT('Ctrl Pts',(1.98600337900854,0.186615931642054,18.734779497184));
#15163=CARTESIAN_POINT('Ctrl Pts',(1.98574765564003,0.18931765785895,18.7349536515509));
#15164=CARTESIAN_POINT('Ctrl Pts',(1.98514697628989,0.195528716707812,18.7353533787729));
#15165=CARTESIAN_POINT('Ctrl Pts',(1.98479822826952,0.199037659892524,18.735578736046));
#15166=CARTESIAN_POINT('Ctrl Pts',(1.98365926390856,0.210196656186417,18.7362939683203));
#15167=CARTESIAN_POINT('Ctrl Pts',(1.98283409777959,0.217843188690037,18.7367819170554));
#15168=CARTESIAN_POINT('Ctrl Pts',(1.96891227422089,0.340213078106433,18.7445589595946));
#15169=CARTESIAN_POINT('Ctrl Pts',(1.9459204166028,0.453610810322624,18.7513247974727));
#15170=CARTESIAN_POINT('Ctrl Pts',(1.88420965684906,0.662803283733112,18.7640012259607));
#15171=CARTESIAN_POINT('Ctrl Pts',(1.84763235638712,0.758820121710295,18.7699058932705));
#15172=CARTESIAN_POINT('Ctrl Pts',(1.78093284945403,0.900101642474769,18.7791732225278));
#15173=CARTESIAN_POINT('Ctrl Pts',(1.75608743554031,0.947660815068347,18.7823985816048));
#15174=CARTESIAN_POINT('Ctrl Pts',(1.7135919535303,1.02158249716475,18.7876275879875));
#15175=CARTESIAN_POINT('Ctrl Pts',(1.69717732333449,1.04862631083313,18.7895886939736));
#15176=CARTESIAN_POINT('Ctrl Pts',(1.67538117404773,1.08268324384145,18.7921258388849));
#15177=CARTESIAN_POINT('Ctrl Pts',(1.67058603883131,1.09006759776965,18.7926800964343));
#15178=CARTESIAN_POINT('Ctrl Pts',(1.66279470007617,1.10189384803548,18.7935745595206));
#15179=CARTESIAN_POINT('Ctrl Pts',(1.6598291765474,1.10635589694647,18.7939136138198));
#15180=CARTESIAN_POINT('Ctrl Pts',(1.65415187629761,1.11482399261759,18.794560100361));
#15181=CARTESIAN_POINT('Ctrl Pts',(1.65144342823373,1.11883223364406,18.7948674054245));
#15182=CARTESIAN_POINT('Ctrl Pts',(1.64523763387576,1.12794457922984,18.7955690268544));
#15183=CARTESIAN_POINT('Ctrl Pts',(1.64173107923765,1.13304232391135,18.7959636909271));
#15184=CARTESIAN_POINT('Ctrl Pts',(1.6309484016413,1.14856277504649,18.7971719297165));
#15185=CARTESIAN_POINT('Ctrl Pts',(1.62359643371152,1.15893215722208,18.7979883959766));
#15186=CARTESIAN_POINT('Ctrl Pts',(1.60895909472359,1.17916433516313,18.7995999503035));
#15187=CARTESIAN_POINT('Ctrl Pts',(1.60168088446205,1.18903163582935,18.8003947378128));
#15188=CARTESIAN_POINT('Ctrl Pts',(1.49754442605915,1.3275215751273,18.811676579866));
#15189=CARTESIAN_POINT('Ctrl Pts',(1.38556985143681,1.44399741018749,18.8227969336188));
#15190=CARTESIAN_POINT('Ctrl Pts',(1.19977304147385,1.59555153108657,18.839526078278));
#15191=CARTESIAN_POINT('Ctrl Pts',(1.13579364657578,1.64171072887518,18.8450237703146));
#15192=CARTESIAN_POINT('Ctrl Pts',(1.04283352101743,1.70073655021552,18.8525151666493));
#15193=CARTESIAN_POINT('Ctrl Pts',(1.01602681260715,1.7168856432162,18.8546211553225));
#15194=CARTESIAN_POINT('Ctrl Pts',(0.973255789743627,1.74129926494946,18.8578844805762));
#15195=CARTESIAN_POINT('Ctrl Pts',(0.957541666725978,1.74998970693847,18.8590634312595));
#15196=CARTESIAN_POINT('Ctrl Pts',(0.93734735555561,1.76080436376682,18.8605511360423));
#15197=CARTESIAN_POINT('Ctrl Pts',(0.932974290446479,1.76312536340153,18.8608716782923));
#15198=CARTESIAN_POINT('Ctrl Pts',(0.925944194897727,1.76682309947044,18.8613843307796));
#15199=CARTESIAN_POINT('Ctrl Pts',(0.923292664123198,1.76821016102545,18.8615770854072));
#15200=CARTESIAN_POINT('Ctrl Pts',(0.918226926846699,1.77084563416485,18.8619441807123));
#15201=CARTESIAN_POINT('Ctrl Pts',(0.915813319758448,1.77209506309847,18.8621185825521));
#15202=CARTESIAN_POINT('Ctrl Pts',(0.910237862333229,1.77496682373411,18.8625203050492));
#15203=CARTESIAN_POINT('Ctrl Pts',(0.90707422588605,1.77658564122103,18.8627474028874));
#15204=CARTESIAN_POINT('Ctrl Pts',(0.89691846924848,1.78174809341721,18.8634737601523));
#15205=CARTESIAN_POINT('Ctrl Pts',(0.889909672188349,1.78525902577176,18.8639710075975));
#15206=CARTESIAN_POINT('Ctrl Pts',(0.80465094407919,1.82734100733099,18.8699732100781));
#15207=CARTESIAN_POINT('Ctrl Pts',(0.723961451506604,1.86078540840954,18.8751811442561));
#15208=CARTESIAN_POINT('Ctrl Pts',(0.474923381145423,1.9453429548555,18.8906032763594));
#15209=CARTESIAN_POINT('Ctrl Pts',(0.301791225474709,1.97960416794822,18.900540973221));
#15210=CARTESIAN_POINT('Ctrl Pts',(0.0874065022654165,1.993217241716,18.9136362010896));
#15211=CARTESIAN_POINT('Ctrl Pts',(0.0483421880211279,1.99454696076952,
18.9160498261827));
#15212=CARTESIAN_POINT('Ctrl Pts',(-0.000184182018821294,1.99477237698326,
18.9190919929695));
#15213=CARTESIAN_POINT('Ctrl Pts',(-0.00963439826761239,1.99474911789121,
18.9196864903936));
#15214=CARTESIAN_POINT('Ctrl Pts',(-0.024584807190945,1.99460607935654,
18.9206303805908));
#15215=CARTESIAN_POINT('Ctrl Pts',(-0.0300853641101711,1.9945306952837,
18.9209783816573));
#15216=CARTESIAN_POINT('Ctrl Pts',(-0.0403996229948302,1.99434666399179,
18.9216323167224));
#15217=CARTESIAN_POINT('Ctrl Pts',(-0.0452133898834948,1.99424333881827,
18.9219380817066));
#15218=CARTESIAN_POINT('Ctrl Pts',(-0.0559827783491645,1.99397316637189,
18.9226234308082));
#15219=CARTESIAN_POINT('Ctrl Pts',(-0.0619381021696555,1.99379706337182,
18.9230033022824));
#15220=CARTESIAN_POINT('Ctrl Pts',(-0.0770067850007071,1.9932838945299,
18.9239667622487));
#15221=CARTESIAN_POINT('Ctrl Pts',(-0.0861187111557444,1.99291100958607,
18.9245514675075));
#15222=CARTESIAN_POINT('Ctrl Pts',(-0.111788007053477,1.9916841808652,18.9262047313863));
#15223=CARTESIAN_POINT('Ctrl Pts',(-0.128337435444675,1.99068629117969,
18.9272777638642));
#15224=CARTESIAN_POINT('Ctrl Pts',(-0.304701315740075,1.97784365080766,
18.9387915399578));
#15225=CARTESIAN_POINT('Ctrl Pts',(-0.462514645459761,1.94698956524212,
18.9498561227056));
#15226=CARTESIAN_POINT('Ctrl Pts',(-0.690388617649494,1.87314908885194,
18.9665692310685));
#15227=CARTESIAN_POINT('Ctrl Pts',(-0.764351364330066,1.84420504166587,
18.9721050536836));
#15228=CARTESIAN_POINT('Ctrl Pts',(-0.864915374895666,1.79775854592652,
18.9796419834379));
#15229=CARTESIAN_POINT('Ctrl Pts',(-0.893121025354515,1.78391408473116,
18.981756613516));
#15230=CARTESIAN_POINT('Ctrl Pts',(-0.93696221813571,1.76109443668826,18.9850318270928));
#15231=CARTESIAN_POINT('Ctrl Pts',(-0.952822370918598,1.75256423523097,
18.9862142063184));
#15232=CARTESIAN_POINT('Ctrl Pts',(-0.972897816596316,1.74141378199585,
18.9877055941949));
#15233=CARTESIAN_POINT('Ctrl Pts',(-0.977221205534696,1.73899132786698,
18.9880264611269));
#15234=CARTESIAN_POINT('Ctrl Pts',(-0.984141603076149,1.73507977586952,
18.9885395091405));
#15235=CARTESIAN_POINT('Ctrl Pts',(-0.986744330563269,1.73360092002989,
18.9887323363509));
#15236=CARTESIAN_POINT('Ctrl Pts',(-0.991703465782193,1.73076837947129,
18.9890994834311));
#15237=CARTESIAN_POINT('Ctrl Pts',(-0.994060407424666,1.7294157550719,18.989273864816));
#15238=CARTESIAN_POINT('Ctrl Pts',(-0.999491283842019,1.72628426080426,
18.9896754255931));
#15239=CARTESIAN_POINT('Ctrl Pts',(-1.00256323622078,1.72450199577505,18.9899023827516));
#15240=CARTESIAN_POINT('Ctrl Pts',(-1.0123897958372,1.71876575533445,18.9906278369023));
#15241=CARTESIAN_POINT('Ctrl Pts',(-1.01912600303422,1.71478016527551,18.9911243289434));
#15242=CARTESIAN_POINT('Ctrl Pts',(-1.11527861181748,1.65712312439682,18.9982021436406));
#15243=CARTESIAN_POINT('Ctrl Pts',(-1.20038931483934,1.59655114342592,19.0043577097433));
#15244=CARTESIAN_POINT('Ctrl Pts',(-1.29377169615538,1.51838310720742,19.0114543864536));
#15245=CARTESIAN_POINT('Ctrl Pts',(-1.30701356560473,1.50699967121291,19.0124693331214));
#15246=CARTESIAN_POINT('Ctrl Pts',(-1.38993866161861,1.43379746776894,19.018891373008));
#15247=CARTESIAN_POINT('Ctrl Pts',(-1.45536769441989,1.367336348808,19.0242651121018));
#15248=CARTESIAN_POINT('Ctrl Pts',(-1.55204766831419,1.25429922722888,19.0330748031148));
#15249=CARTESIAN_POINT('Ctrl Pts',(-1.58639959137859,1.2105594195541,19.0364131852246));
#15250=CARTESIAN_POINT('Ctrl Pts',(-1.63784172652565,1.13910295306852,19.0418090721298));
#15251=CARTESIAN_POINT('Ctrl Pts',(-1.65615861181991,1.11230370069679,19.0438204543072));
#15252=CARTESIAN_POINT('Ctrl Pts',(-1.67864507651206,1.07761643745878,19.0464140125854));
#15253=CARTESIAN_POINT('Ctrl Pts',(-1.68342746359027,1.0701301088647,19.0469731851214));
#15254=CARTESIAN_POINT('Ctrl Pts',(-1.69102301814097,1.05806313962287,19.0478736857798));
#15255=CARTESIAN_POINT('Ctrl Pts',(-1.69386799071595,1.05350257921687,19.0482138343073));
#15256=CARTESIAN_POINT('Ctrl Pts',(-1.69923633291403,1.04481903386631,19.0488611722867));
#15257=CARTESIAN_POINT('Ctrl Pts',(-1.7017632206451,1.040698260212,19.0491682292814));
#15258=CARTESIAN_POINT('Ctrl Pts',(-1.70747390642219,1.03130902959119,19.0498675729913));
#15259=CARTESIAN_POINT('Ctrl Pts',(-1.71064833331723,1.02603495746683,19.0502601990836));
#15260=CARTESIAN_POINT('Ctrl Pts',(-1.72022119555614,1.0099624482373,19.051456141146));
#15261=CARTESIAN_POINT('Ctrl Pts',(-1.72654207019005,0.999118399581432,
19.0522622633811));
#15262=CARTESIAN_POINT('Ctrl Pts',(-1.81034008412279,0.85218502913537,19.0631762960184));
#15263=CARTESIAN_POINT('Ctrl Pts',(-1.87161514653113,0.707521813089579,
19.0738885840095));
#15264=CARTESIAN_POINT('Ctrl Pts',(-1.95127628739698,0.433700962961726,
19.0937666322128));
#15265=CARTESIAN_POINT('Ctrl Pts',(-1.9751813042528,0.306985718346887,19.1028022149009));
#15266=CARTESIAN_POINT('Ctrl Pts',(-1.98771019595702,0.167805072338022,
19.112047353306));
#15267=CARTESIAN_POINT('Ctrl Pts',(-1.98861177279394,0.15675967393898,19.1127763069781));
#15268=CARTESIAN_POINT('Ctrl Pts',(-1.99001848749443,0.137552997706097,
19.1140349845805));
#15269=CARTESIAN_POINT('Ctrl Pts',(-1.99056557319754,0.12939517818003,19.1145668112959));
#15270=CARTESIAN_POINT('Ctrl Pts',(-1.99128461251944,0.117586184358204,
19.1153324192907));
#15271=CARTESIAN_POINT('Ctrl Pts',(-1.99149670501233,0.113937672679454,
19.1155683756559));
#15272=CARTESIAN_POINT('Ctrl Pts',(-1.99184935975692,0.107569088295612,
19.1159791973249));
#15273=CARTESIAN_POINT('Ctrl Pts',(-1.99199437964554,0.104849284916977,
19.116154311442));
#15274=CARTESIAN_POINT('Ctrl Pts',(-1.99228610422705,0.0991588976492834,
19.1165199796931));
#15275=CARTESIAN_POINT('Ctrl Pts',(-1.9924317358545,0.0961882857901529,
19.1167104728276));
#15276=CARTESIAN_POINT('Ctrl Pts',(-1.99279826689133,0.088353487577497,
19.1172118564511));
#15277=CARTESIAN_POINT('Ctrl Pts',(-1.9930080028155,0.0834887609890627,
19.117522125465));
#15278=CARTESIAN_POINT('Ctrl Pts',(-1.99380599890046,0.0632585406961544,
19.1188082258013));
#15279=CARTESIAN_POINT('Ctrl Pts',(-1.99423441356957,0.047886768939276,
19.1197754603846));
#15280=CARTESIAN_POINT('Ctrl Pts',(-1.9946576362865,0.0219229165871689,
19.1213946140827));
#15281=CARTESIAN_POINT('Ctrl Pts',(-1.99474591490793,0.0113333676914158,
19.1220509090515));
#15282=CARTESIAN_POINT('Ctrl Pts',(-1.99476839303552,-0.048983006416836,
19.1257683116931));
#15283=CARTESIAN_POINT('Ctrl Pts',(-1.99292749707664,-0.0986965709033473,
19.1287521200525));
#15284=CARTESIAN_POINT('Ctrl Pts',(-1.97716859296675,-0.310089713484085,
19.1412897896345));
#15285=CARTESIAN_POINT('Ctrl Pts',(-1.94541352259528,-0.469809221487074,
19.1504385273581));
#15286=CARTESIAN_POINT('Ctrl Pts',(-1.8742613111753,-0.685876414871118,
19.1640443629668));
#15287=CARTESIAN_POINT('Ctrl Pts',(-1.8508355279696,-0.74678537698661,19.1680190355975));
#15288=CARTESIAN_POINT('Ctrl Pts',(-1.82023017919837,-0.816026759479792,
19.172751580658));
#15289=CARTESIAN_POINT('Ctrl Pts',(-1.81591425457809,-0.825586452630829,
19.1734097952444));
#15290=CARTESIAN_POINT('Ctrl Pts',(-1.80888297058829,-0.840838707910833,
19.174467906899));
#15291=CARTESIAN_POINT('Ctrl Pts',(-1.80621561883299,-0.846553288816695,
19.1748661512205));
#15292=CARTESIAN_POINT('Ctrl Pts',(-1.80144121860599,-0.856656757236279,
19.175573492567));
#15293=CARTESIAN_POINT('Ctrl Pts',(-1.79934510765298,-0.861050780551459,
19.1758822088685));
#15294=CARTESIAN_POINT('Ctrl Pts',(-1.79495618389666,-0.870165156154452,
19.1765248622556));
#15295=CARTESIAN_POINT('Ctrl Pts',(-1.79266078974096,-0.874884216997918,
19.1768588873432));
#15296=CARTESIAN_POINT('Ctrl Pts',(-1.78668250115603,-0.887052567836725,
19.1777235444016));
#15297=CARTESIAN_POINT('Ctrl Pts',(-1.78297165922339,-0.894487941217826,
19.1782551497565));
#15298=CARTESIAN_POINT('Ctrl Pts',(-1.76705150854837,-0.925894270987347,
19.1805146460061));
#15299=CARTESIAN_POINT('Ctrl Pts',(-1.75440489313891,-0.949639188376966,
19.1822578490267));
#15300=CARTESIAN_POINT('Ctrl Pts',(-1.72030560483097,-1.01065579717979,
19.1868313393125));
#15301=CARTESIAN_POINT('Ctrl Pts',(-1.69812193986251,-1.04750080433859,
19.1896867957139));
#15302=CARTESIAN_POINT('Ctrl Pts',(-1.58360803362604,-1.22448897400096,
19.2038714932848));
#15303=CARTESIAN_POINT('Ctrl Pts',(-1.47503888079859,-1.35330497143333,
19.2157573295699));
#15304=CARTESIAN_POINT('Ctrl Pts',(-1.33863676598694,-1.4789836508341,19.2285350574922));
#15305=CARTESIAN_POINT('Ctrl Pts',(-1.3254566144096,-1.49080710433722,19.2297497642909));
#15306=CARTESIAN_POINT('Ctrl Pts',(-1.27455659047977,-1.53525903134374,
19.2343604340685));
#15307=CARTESIAN_POINT('Ctrl Pts',(-1.23577175977686,-1.56664735245848,
19.2377088687697));
#15308=CARTESIAN_POINT('Ctrl Pts',(-1.19012837665718,-1.60083511549484,
19.2414292448915));
#15309=CARTESIAN_POINT('Ctrl Pts',(-1.18438624525612,-1.60508811151589,
19.2418934381641));
#15310=CARTESIAN_POINT('Ctrl Pts',(-1.1758307125715,-1.61135398408785,19.242579228929));
#15311=CARTESIAN_POINT('Ctrl Pts',(-1.17303480856813,-1.61339048744984,
19.2428024237873));
#15312=CARTESIAN_POINT('Ctrl Pts',(-1.16804833011863,-1.61700276511912,
19.2431988384401));
#15313=CARTESIAN_POINT('Ctrl Pts',(-1.16585984748929,-1.61858137275435,
19.2433722535158));
#15314=CARTESIAN_POINT('Ctrl Pts',(-1.16116722341014,-1.62195182507142,
19.2437428846018));
#15315=CARTESIAN_POINT('Ctrl Pts',(-1.15866214290623,-1.62374230790631,
19.2439400065799));
#15316=CARTESIAN_POINT('Ctrl Pts',(-1.15180119584587,-1.62862214311728,
19.2444779149781));
#15317=CARTESIAN_POINT('Ctrl Pts',(-1.14743701401561,-1.63169984379864,
19.2448179078511));
#15318=CARTESIAN_POINT('Ctrl Pts',(-1.12464457279186,-1.64763682419787,
19.2465826130695));
#15319=CARTESIAN_POINT('Ctrl Pts',(-1.10601145432191,-1.66020218236204,
19.2479881723778));
#15320=CARTESIAN_POINT('Ctrl Pts',(-1.05107035289388,-1.69591639934581,
19.2520380519196));
#15321=CARTESIAN_POINT('Ctrl Pts',(-1.01421880307146,-1.71820896810674,
19.2546369334057));
#15322=CARTESIAN_POINT('Ctrl Pts',(-0.904327494207502,-1.7799166836451,
19.2621356140406));
#15323=CARTESIAN_POINT('Ctrl Pts',(-0.829515123935788,-1.81598943981576,
19.2669303912729));
#15324=CARTESIAN_POINT('Ctrl Pts',(-0.611798877444507,-1.90469654178063,
19.2805670291109));
#15325=CARTESIAN_POINT('Ctrl Pts',(-0.464847824657405,-1.94578370274167,
19.2894465545446));
#15326=CARTESIAN_POINT('Ctrl Pts',(-0.302142015231538,-1.97177549886785,
19.2997343912466));
#15327=CARTESIAN_POINT('Ctrl Pts',(-0.289599475004221,-1.97365664378116,
19.3005299457173));
#15328=CARTESIAN_POINT('Ctrl Pts',(-0.270918257092855,-1.97627656825619,
19.3017188939477));
#15329=CARTESIAN_POINT('Ctrl Pts',(-0.264792537492503,-1.97710664531663,
19.3021094013073));
#15330=CARTESIAN_POINT('Ctrl Pts',(-0.253867072191385,-1.97853543500308,
19.3028070695785));
#15331=CARTESIAN_POINT('Ctrl Pts',(-0.249068800022455,-1.97914519176484,
19.3031138792046));
#15332=CARTESIAN_POINT('Ctrl Pts',(-0.238948011232242,-1.98039393753044,
19.3037618957626));
#15333=CARTESIAN_POINT('Ctrl Pts',(-0.233625049232619,-1.98102893349015,
19.3041032260982));
#15334=CARTESIAN_POINT('Ctrl Pts',(-0.219539099495734,-1.98265173742433,
19.3050078570906));
#15335=CARTESIAN_POINT('Ctrl Pts',(-0.21077208682156,-1.9836028965983,19.3055723074751));
#15336=CARTESIAN_POINT('Ctrl Pts',(-0.170386904903891,-1.98771365003396,
19.3081791674521));
#15337=CARTESIAN_POINT('Ctrl Pts',(-0.138703890513937,-1.99017544176523,
19.3102433602147));
#15338=CARTESIAN_POINT('Ctrl Pts',(-0.0530774929440565,-1.9947741436719,
19.3158770728432));
#15339=CARTESIAN_POINT('Ctrl Pts',(0.00091289138800443,-1.99547974140178,
19.3194887166107));
#15340=CARTESIAN_POINT('Ctrl Pts',(0.157733712683046,-1.99116506483945,
19.3301446071597));
#15341=CARTESIAN_POINT('Ctrl Pts',(0.260224995331925,-1.9803782276437,19.337324491093));
#15342=CARTESIAN_POINT('Ctrl Pts',(0.474155444052555,-1.94096509563844,
19.3524974236475));
#15343=CARTESIAN_POINT('Ctrl Pts',(0.58490847222163,-1.91051240722891,19.3604622101961));
#15344=CARTESIAN_POINT('Ctrl Pts',(0.699578072011126,-1.86806744222649,
19.3684472071921));
#15345=CARTESIAN_POINT('Ctrl Pts',(0.706698156315862,-1.8653855279601,19.3689418496829));
#15346=CARTESIAN_POINT('Ctrl Pts',(0.71713160345363,-1.86138726051182,19.3696647822078));
#15347=CARTESIAN_POINT('Ctrl Pts',(0.720456953983365,-1.86010269829635,
19.3698949116593));
#15348=CARTESIAN_POINT('Ctrl Pts',(0.726313033624408,-1.85782247142042,
19.3702996557139));
#15349=CARTESIAN_POINT('Ctrl Pts',(0.728845192026877,-1.85683053738073,
19.3704744927677));
#15350=CARTESIAN_POINT('Ctrl Pts',(0.734154262788085,-1.85473825717146,
19.3708406938882));
#15351=CARTESIAN_POINT('Ctrl Pts',(0.736930728580738,-1.85363685379489,
19.371031992736));
#15352=CARTESIAN_POINT('Ctrl Pts',(0.744279783292718,-1.85070241663658,
19.3715378078947));
#15353=CARTESIAN_POINT('Ctrl Pts',(0.748848110106667,-1.84885865874066,
19.3718516827719));
#15354=CARTESIAN_POINT('Ctrl Pts',(0.769802485695587,-1.84031115173197,
19.3732890645036));
#15355=CARTESIAN_POINT('Ctrl Pts',(0.786106290284432,-1.83340610745724,
19.3744008901022));
#15356=CARTESIAN_POINT('Ctrl Pts',(0.830407735590246,-1.81394375877727,
19.37740971865));
#15357=CARTESIAN_POINT('Ctrl Pts',(0.85821194795794,-1.80095570001954,19.3792845533385));
#15358=CARTESIAN_POINT('Ctrl Pts',(0.954030039250381,-1.75347329833501,
19.3857353190476));
#15359=CARTESIAN_POINT('Ctrl Pts',(1.02036054452499,-1.71572372907188,19.3901841556255));
#15360=CARTESIAN_POINT('Ctrl Pts',(1.22261733967541,-1.5847282583496,19.4041786494978));
#15361=CARTESIAN_POINT('Ctrl Pts',(1.3492244997805,-1.47842582543381,19.4136540525626));
#15362=CARTESIAN_POINT('Ctrl Pts',(1.47549225304111,-1.34252875701256,19.4251349004271));
#15363=CARTESIAN_POINT('Ctrl Pts',(1.48942093545346,-1.32705918406338,19.4264327682386));
#15364=CARTESIAN_POINT('Ctrl Pts',(1.50822903482301,-1.30550124512892,19.4282306553767));
#15365=CARTESIAN_POINT('Ctrl Pts',(1.51331895316874,-1.29959765531884,19.4287219147869));
#15366=CARTESIAN_POINT('Ctrl Pts',(1.52137123390345,-1.29014669270614,19.429506714626));
#15367=CARTESIAN_POINT('Ctrl Pts',(1.52435613193959,-1.28661855360503,19.429799325983));
#15368=CARTESIAN_POINT('Ctrl Pts',(1.53045622720997,-1.27935723708179,19.4304008308354));
#15369=CARTESIAN_POINT('Ctrl Pts',(1.5335700871459,-1.27562298137129,19.4307097760893));
#15370=CARTESIAN_POINT('Ctrl Pts',(1.54073370236568,-1.26696796927881,19.4314249555176));
#15371=CARTESIAN_POINT('Ctrl Pts',(1.54477357385966,-1.26203913597407,19.4318315865641));
#15372=CARTESIAN_POINT('Ctrl Pts',(1.55740458190825,-1.24647719635869,19.4331134877558));
#15373=CARTESIAN_POINT('Ctrl Pts',(1.56590992835681,-1.23577526824021,19.4339921875742));
#15374=CARTESIAN_POINT('Ctrl Pts',(1.65083171511155,-1.12663717349122,19.4429260621571));
#15375=CARTESIAN_POINT('Ctrl Pts',(1.71796008638762,-1.02135170846673,19.4513504643823));
#15376=CARTESIAN_POINT('Ctrl Pts',(1.83574210664646,-0.791764391708617,
19.4692242591229));
#15377=CARTESIAN_POINT('Ctrl Pts',(1.88459073080402,-0.667202286636079,
19.4786593256417));
#15378=CARTESIAN_POINT('Ctrl Pts',(1.93109057120555,-0.501413899195394,
19.4903108470931));
#15379=CARTESIAN_POINT('Ctrl Pts',(1.94045999604452,-0.463834221967416,
19.4928924240836));
#15380=CARTESIAN_POINT('Ctrl Pts',(1.95014130214841,-0.419547523949938,
19.4958473087531));
#15381=CARTESIAN_POINT('Ctrl Pts',(1.95152038051191,-0.413085258302716,
19.4962763188432));
#15382=CARTESIAN_POINT('Ctrl Pts',(1.95355938964025,-0.403292449171764,
19.4969230388686));
#15383=CARTESIAN_POINT('Ctrl Pts',(1.95424295373218,-0.399966956908765,
19.4971420640202));
#15384=CARTESIAN_POINT('Ctrl Pts',(1.95545345057473,-0.394000781382996,
19.4975339313515));
#15385=CARTESIAN_POINT('Ctrl Pts',(1.95598352714996,-0.391360773335032,
19.497706951255));
#15386=CARTESIAN_POINT('Ctrl Pts',(1.95711678186754,-0.385656862491291,
19.498079949533));
#15387=CARTESIAN_POINT('Ctrl Pts',(1.95771810965317,-0.382592625278867,
19.4982798210231));
#15388=CARTESIAN_POINT('Ctrl Pts',(1.95936579969838,-0.374090748190541,
19.4988329938481));
#15389=CARTESIAN_POINT('Ctrl Pts',(1.96039672930861,-0.368650092072454,
19.4991854244682));
#15390=CARTESIAN_POINT('Ctrl Pts',(1.9659934612328,-0.338426240792695,19.5011349195552));
#15391=CARTESIAN_POINT('Ctrl Pts',(1.97011221114455,-0.313561205596149,
19.5027077389574));
#15392=CARTESIAN_POINT('Ctrl Pts',(1.99728902559753,-0.127711838216945,
19.5142779357084));
#15393=CARTESIAN_POINT('Ctrl Pts',(2.00105681247822,0.0354939515073905,
19.5234447187878));
#15394=CARTESIAN_POINT('Ctrl Pts',(1.98296508720919,0.217449997489708,19.5341341875849));
#15395=CARTESIAN_POINT('Ctrl Pts',(1.98066309160486,0.237505229415738,19.5353181439386));
#15396=CARTESIAN_POINT('Ctrl Pts',(1.96612913265591,0.349142386546518,19.5419518897035));
#15397=CARTESIAN_POINT('Ctrl Pts',(1.94785169654975,0.439811924896973,19.5475097644353));
#15398=CARTESIAN_POINT('Ctrl Pts',(1.92001813227682,0.541033055582209,19.5540650021422));
#15399=CARTESIAN_POINT('Ctrl Pts',(1.91656161764104,0.553152736294349,19.5548555968101));
#15400=CARTESIAN_POINT('Ctrl Pts',(1.91124336186034,0.571151812234453,19.5560385537288));
#15401=CARTESIAN_POINT('Ctrl Pts',(1.90946878039123,0.577056805001016,19.5564280724569));
#15402=CARTESIAN_POINT('Ctrl Pts',(1.90625385994332,0.58757736630923,19.5571246367674));
#15403=CARTESIAN_POINT('Ctrl Pts',(1.90482405738415,0.592196124340333,19.5574313352424));
#15404=CARTESIAN_POINT('Ctrl Pts',(1.90177098821307,0.601933137743208,19.558079804301));
#15405=CARTESIAN_POINT('Ctrl Pts',(1.90014382185789,0.607050120869674,19.5584217009231));
#15406=CARTESIAN_POINT('Ctrl Pts',(1.895777681335,0.620590853041795,19.5593294273112));
#15407=CARTESIAN_POINT('Ctrl Pts',(1.89300324776476,0.629002959993402,19.5598964209307));
#15408=CARTESIAN_POINT('Ctrl Pts',(1.87988804530172,0.667895567992703,19.5625323625652));
#15409=CARTESIAN_POINT('Ctrl Pts',(1.86886702568252,0.69813995137732,19.564623691124));
#15410=CARTESIAN_POINT('Ctrl Pts',(1.83706195017677,0.779262849624398,19.5703503303172));
#15411=CARTESIAN_POINT('Ctrl Pts',(1.81490048429291,0.829567665639743,19.5740294898851));
#15412=CARTESIAN_POINT('Ctrl Pts',(1.74501600509554,0.97195364741234,19.5848111966556));
#15413=CARTESIAN_POINT('Ctrl Pts',(1.69215724610676,1.06130832576484,19.5920487764715));
#15414=CARTESIAN_POINT('Ctrl Pts',(1.59697525989306,1.19688839243667,19.6036014060277));
#15415=CARTESIAN_POINT('Ctrl Pts',(1.55900191879886,1.24594764334008,19.6079132913364));
#15416=CARTESIAN_POINT('Ctrl Pts',(1.48563751044459,1.33211338625452,19.6156409856782));
#15417=CARTESIAN_POINT('Ctrl Pts',(1.45098180929269,1.36978017117031,19.6190785459187));
#15418=CARTESIAN_POINT('Ctrl Pts',(1.40984365532526,1.4111768650237,19.6228862631286));
#15419=CARTESIAN_POINT('Ctrl Pts',(1.40474697358939,1.41625040895099,19.6233534613281));
#15420=CARTESIAN_POINT('Ctrl Pts',(1.39715188823104,1.42372967604132,19.6240428221016));
#15421=CARTESIAN_POINT('Ctrl Pts',(1.39467453985458,1.42615655436457,19.6242666059536));
#15422=CARTESIAN_POINT('Ctrl Pts',(1.39025767596323,1.43046091988443,19.6246636704338));
#15423=CARTESIAN_POINT('Ctrl Pts',(1.38832067092181,1.43234093843091,19.6248371488174));
#15424=CARTESIAN_POINT('Ctrl Pts',(1.38417004653905,1.43635312184936,19.6252074801518));
#15425=CARTESIAN_POINT('Ctrl Pts',(1.38195532142411,1.43848409733394,19.625404240789));
#15426=CARTESIAN_POINT('Ctrl Pts',(1.37589763094082,1.4442858145237,19.6259401501067));
#15427=CARTESIAN_POINT('Ctrl Pts',(1.37204487285791,1.44794636409177,19.6262785151126));
#15428=CARTESIAN_POINT('Ctrl Pts',(1.35206714848454,1.46677609141313,19.6280205743258));
#15429=CARTESIAN_POINT('Ctrl Pts',(1.33570432662753,1.4816921838507,19.6294056958277));
#15430=CARTESIAN_POINT('Ctrl Pts',(1.28749237698159,1.52419352282174,19.6333794615361));
#15431=CARTESIAN_POINT('Ctrl Pts',(1.25501206974719,1.55104729485839,19.6359246791852));
#15432=CARTESIAN_POINT('Ctrl Pts',(1.11929795674476,1.65619489474771,19.6461486394356));
#15433=CARTESIAN_POINT('Ctrl Pts',(1.00940302885524,1.72537490426838,19.6535166351076));
#15434=CARTESIAN_POINT('Ctrl Pts',(0.798341270827465,1.83112644503387,19.6673447423129));
#15435=CARTESIAN_POINT('Ctrl Pts',(0.699456781502086,1.87113021093521,19.6737083273922));
#15436=CARTESIAN_POINT('Ctrl Pts',(0.585583691370159,1.90690453422303,19.6811593534654));
#15437=CARTESIAN_POINT('Ctrl Pts',(0.573269927538925,1.9106424940467,19.6819664416302));
#15438=CARTESIAN_POINT('Ctrl Pts',(0.554953670335571,1.91600956517889,19.6831693109417));
#15439=CARTESIAN_POINT('Ctrl Pts',(0.548978168530095,1.91773022063343,19.6835621047909));
#15440=CARTESIAN_POINT('Ctrl Pts',(0.538336269393341,1.92074075866265,19.684262336082));
#15441=CARTESIAN_POINT('Ctrl Pts',(0.533673017053685,1.92204165176616,19.6845694125659));
#15442=CARTESIAN_POINT('Ctrl Pts',(0.528996770175458,1.92332783989592,19.6848775917535));
#15443=CARTESIAN_POINT('Ctrl Pts',(0.528988431769083,1.92333013329206,19.6848781412812));
#15444=CARTESIAN_POINT('Ctrl Pts',(0.528971774508747,1.92333471459013,19.6848792390495));
#15445=CARTESIAN_POINT('Ctrl Pts',(0.528963455439792,1.92333700255146,19.6848797873043));
#15446=CARTESIAN_POINT('Ctrl Pts',(0.528946836530065,1.92334157306988,19.6848808825483));
#15447=CARTESIAN_POINT('Ctrl Pts',(0.528938536674659,1.92334385563127,19.6848814295385));
#15448=CARTESIAN_POINT('Ctrl Pts',(0.528921956022896,1.92334841539713,19.6848825222643));
#15449=CARTESIAN_POINT('Ctrl Pts',(0.528913675266873,1.92335069259078,19.6848830679972));
#15450=CARTESIAN_POINT('Ctrl Pts',(0.528897132834853,1.92335524161619,19.6848841582073));
#15451=CARTESIAN_POINT('Ctrl Pts',(0.52888887113718,1.92335751345418,19.6848847026858));
#15452=CARTESIAN_POINT('Ctrl Pts',(0.528872366698314,1.92336205180304,19.6848857903951));
#15453=CARTESIAN_POINT('Ctrl Pts',(0.528864123974618,1.92336431830936,19.6848863336246));
#15454=CARTESIAN_POINT('Ctrl Pts',(0.52884765740287,1.9233688460179,19.6848874188414));
#15455=CARTESIAN_POINT('Ctrl Pts',(0.528839433581744,1.92337110721298,19.6848879608267));
#15456=CARTESIAN_POINT('Ctrl Pts',(0.523767009059326,1.9247657695497,19.6852222559986));
#15457=CARTESIAN_POINT('Ctrl Pts',(0.518697369340324,1.926138153295,19.6855566576926));
#15458=CARTESIAN_POINT('Ctrl Pts',(0.505457569011053,1.9296661904875,19.6864307625936));
#15459=CARTESIAN_POINT('Ctrl Pts',(0.497279093834176,1.9317899626959,19.6869714932033));
#15460=CARTESIAN_POINT('Ctrl Pts',(0.479334087869849,1.93632838327724,19.688159749012));
#15461=CARTESIAN_POINT('Ctrl Pts',(0.469562331226193,1.93872122457047,19.6888079628767));
#15462=CARTESIAN_POINT('Ctrl Pts',(0.440789333833013,1.94553666803724,19.690720216513));
#15463=CARTESIAN_POINT('Ctrl Pts',(0.421741266328446,1.94975445197798,19.6919907404962));
#15464=CARTESIAN_POINT('Ctrl Pts',(0.354849177478144,1.9635401929018,19.6964695151028));
#15465=CARTESIAN_POINT('Ctrl Pts',(0.306721796246643,1.97163107906789,19.6997227287004));
#15466=CARTESIAN_POINT('Ctrl Pts',(0.140754504018667,1.99330885840251,19.7110433475078));
#15467=CARTESIAN_POINT('Ctrl Pts',(0.0220338853879719,1.99814947685828,
19.7193332512861));
#15468=CARTESIAN_POINT('Ctrl Pts',(-0.16861596155308,1.98892525505808,19.7326368020005));
#15469=CARTESIAN_POINT('Ctrl Pts',(-0.240594339664068,1.98150720372225,
19.7376519979553));
#15470=CARTESIAN_POINT('Ctrl Pts',(-0.347870086339265,1.96451820581839,
19.7449868298044));
#15471=CARTESIAN_POINT('Ctrl Pts',(-0.383566160362162,1.95786178977921,
19.7474034302511));
#15472=CARTESIAN_POINT('Ctrl Pts',(-0.424841420474535,1.94899262659045,
19.7501545771088));
#15473=CARTESIAN_POINT('Ctrl Pts',(-0.430614109898085,1.94772533524217,
19.7505383566897));
#15474=CARTESIAN_POINT('Ctrl Pts',(-0.439825355828883,1.94566021636343,
19.7511490604085));
#15475=CARTESIAN_POINT('Ctrl Pts',(-0.44326751951239,1.94487889797425,19.7513769001245));
#15476=CARTESIAN_POINT('Ctrl Pts',(-0.449352983855655,1.94348059568533,
19.7517790162262));
#15477=CARTESIAN_POINT('Ctrl Pts',(-0.451997119432893,1.9428673486079,19.7519535056696));
#15478=CARTESIAN_POINT('Ctrl Pts',(-0.457565585880516,1.94156388638086,
19.7523204826375));
#15479=CARTESIAN_POINT('Ctrl Pts',(-0.460489604128814,1.94087246233817,
19.752512899199));
#15480=CARTESIAN_POINT('Ctrl Pts',(-0.468280637801568,1.93901156828188,
19.7530248616521));
#15481=CARTESIAN_POINT('Ctrl Pts',(-0.473144872205223,1.93783037154559,
19.7533437380114));
#15482=CARTESIAN_POINT('Ctrl Pts',(-0.495995359310248,1.93219035009836,
19.7548383495802));
#15483=CARTESIAN_POINT('Ctrl Pts',(-0.513924080764138,1.92749916844414,
19.756001238207));
#15484=CARTESIAN_POINT('Ctrl Pts',(-0.697586910028123,1.87669746826354,
19.7678374729394));
#15485=CARTESIAN_POINT('Ctrl Pts',(-0.856784177585974,1.80957464040822,
19.777502249278));
#15486=CARTESIAN_POINT('Ctrl Pts',(-1.10075860959072,1.66719702552204,19.7940254301368));
#15487=CARTESIAN_POINT('Ctrl Pts',(-1.19131115462912,1.60374186942225,19.8006085318692));
#15488=CARTESIAN_POINT('Ctrl Pts',(-1.28607029787913,1.52486640889814,19.8083045050831));
#15489=CARTESIAN_POINT('Ctrl Pts',(-1.29591634681992,1.51650756200604,19.8091145155165));
#15490=CARTESIAN_POINT('Ctrl Pts',(-1.31038844955407,1.50397754511282,19.810320909472));
#15491=CARTESIAN_POINT('Ctrl Pts',(-1.31507739272414,1.49987926002241,19.8107142798681));
#15492=CARTESIAN_POINT('Ctrl Pts',(-1.32337814762155,1.4925552889251,19.8114151595231));
#15493=CARTESIAN_POINT('Ctrl Pts',(-1.32699756514698,1.4893382669887,19.8117223053826));
#15494=CARTESIAN_POINT('Ctrl Pts',(-1.33396467964407,1.48310017522629,19.8123165374281));
#15495=CARTESIAN_POINT('Ctrl Pts',(-1.33731392036838,1.48008086743015,19.8126035483229));
#15496=CARTESIAN_POINT('Ctrl Pts',(-1.34613465986495,1.47207467417824,19.8133630345146));
#15497=CARTESIAN_POINT('Ctrl Pts',(-1.35158864412761,1.4670686771462,19.8138363187944));
#15498=CARTESIAN_POINT('Ctrl Pts',(-1.37260447468016,1.4475624154564,19.8156744776291));
#15499=CARTESIAN_POINT('Ctrl Pts',(-1.38796140542261,1.43284439815516,19.8170486632067));
#15500=CARTESIAN_POINT('Ctrl Pts',(-1.4256472744616,1.39555201765806,19.8205005852092));
#15501=CARTESIAN_POINT('Ctrl Pts',(-1.44767746247111,1.3726854558754,19.8225908999529));
#15502=CARTESIAN_POINT('Ctrl Pts',(-1.51759829961032,1.29655412155817,19.8294685569744));
#15503=CARTESIAN_POINT('Ctrl Pts',(-1.56316421686485,1.24123850464797,19.8343430623945));
#15504=CARTESIAN_POINT('Ctrl Pts',(-1.6631517477396,1.10559666915233,19.8459759612245));
#15505=CARTESIAN_POINT('Ctrl Pts',(-1.71488871361407,1.02351037431295,19.8527803439846));
#15506=CARTESIAN_POINT('Ctrl Pts',(-1.79990058259537,0.863957685751478,
19.8653189250707));
#15507=CARTESIAN_POINT('Ctrl Pts',(-1.83464359959019,0.787496943212655,
19.8710596827132));
#15508=CARTESIAN_POINT('Ctrl Pts',(-1.86725083618624,0.701757103145022,
19.8770513451247));
#15509=CARTESIAN_POINT('Ctrl Pts',(-1.86998768077486,0.694431275005862,
19.8775598086447));
#15510=CARTESIAN_POINT('Ctrl Pts',(-1.87390431186957,0.683756387065318,
19.8782954767469));
#15511=CARTESIAN_POINT('Ctrl Pts',(-1.87511830866236,0.680420087809079,
19.8785246587431));
#15512=CARTESIAN_POINT('Ctrl Pts',(-1.87724574141984,0.674524552974935,
19.8789283130932));
#15513=CARTESIAN_POINT('Ctrl Pts',(-1.87816286291818,0.671966671019204,
19.8791030040108));
#15514=CARTESIAN_POINT('Ctrl Pts',(-1.8800795470413,0.666586396500776,19.8794695152996));
#15515=CARTESIAN_POINT('Ctrl Pts',(-1.88107798050172,0.66376363169755,19.8796612681041));
#15516=CARTESIAN_POINT('Ctrl Pts',(-1.88371299409546,0.656260241596638,
19.8801695798418));
#15517=CARTESIAN_POINT('Ctrl Pts',(-1.88533849720944,0.651575706297139,
19.8804854859878));
#15518=CARTESIAN_POINT('Ctrl Pts',(-1.8927953063312,0.629824393445433,19.8819458308175));
#15519=CARTESIAN_POINT('Ctrl Pts',(-1.89841267591128,0.612684425602411,
19.8830781277802));
#15520=CARTESIAN_POINT('Ctrl Pts',(-1.94958707766242,0.449073010482196,
19.893733024));
#15521=CARTESIAN_POINT('Ctrl Pts',(-1.97834515292007,0.297860772534878,
19.9024453692807));
#15522=CARTESIAN_POINT('Ctrl Pts',(-1.99295987685804,0.0971005213254474,
19.9141562793086));
#15523=CARTESIAN_POINT('Ctrl Pts',(-1.99471555074445,0.0492652185206632,
19.9169542660838));
#15524=CARTESIAN_POINT('Ctrl Pts',(-1.99474949800079,0.00141517687806603,
19.9197876209294));
#15525=CARTESIAN_POINT('',(-1.9947498118588,-0.000866365563652432,21.5209548813952));
#15526=CARTESIAN_POINT('Ctrl Pts',(-1.9947494997464,0.00141271422995681,
19.9197877667508));
#15527=CARTESIAN_POINT('Ctrl Pts',(-1.99479242181115,-0.0591931502589759,
19.9233764363657));
#15528=CARTESIAN_POINT('Ctrl Pts',(-1.99207330674086,-0.119766089450529,
19.92701909106));
#15529=CARTESIAN_POINT('Ctrl Pts',(-1.98427649614867,-0.205760107810383,
19.9323275983535));
#15530=CARTESIAN_POINT('Ctrl Pts',(-1.98145557484169,-0.23135285878207,
19.9339246943544));
#15531=CARTESIAN_POINT('Ctrl Pts',(-1.97720826146773,-0.264059509659338,
19.9359905909697));
#15532=CARTESIAN_POINT('Ctrl Pts',(-1.97623727196789,-0.271230854685799,
19.9364450986454));
#15533=CARTESIAN_POINT('Ctrl Pts',(-1.9745091744404,-0.283491724204659,
19.9372248656381));
#15534=CARTESIAN_POINT('Ctrl Pts',(-1.97377135266513,-0.288583929276865,
19.9375495162768));
#15535=CARTESIAN_POINT('Ctrl Pts',(-1.97235065208835,-0.298128763649968,
19.9381595609322));
#15536=CARTESIAN_POINT('Ctrl Pts',(-1.97167237512711,-0.302582053542001,
19.9384448078909));
#15537=CARTESIAN_POINT('Ctrl Pts',(-1.97022956283687,-0.311844096913889,
19.939039380726));
#15538=CARTESIAN_POINT('Ctrl Pts',(-1.96946249399423,-0.316652420037105,
19.9393487850847));
#15539=CARTESIAN_POINT('Ctrl Pts',(-1.96766076359161,-0.327686609082672,
19.9400605227809));
#15540=CARTESIAN_POINT('Ctrl Pts',(-1.96661414820451,-0.33391044445781,
19.9404632330166));
#15541=CARTESIAN_POINT('Ctrl Pts',(-1.96374678398932,-0.350480366210433,
19.9415387778681));
#15542=CARTESIAN_POINT('Ctrl Pts',(-1.96187383131615,-0.360817102841638,
19.9422132651641));
#15543=CARTESIAN_POINT('Ctrl Pts',(-1.94771184974379,-0.43560414074995,
19.9471194231022));
#15544=CARTESIAN_POINT('Ctrl Pts',(-1.93233255721125,-0.49942131411221,
19.9514492071957));
#15545=CARTESIAN_POINT('Ctrl Pts',(-1.91156642651027,-0.570093272099501,
19.9564107267023));
#15546=CARTESIAN_POINT('Ctrl Pts',(-1.90924704253492,-0.577813351980916,
19.9569549558359));
#15547=CARTESIAN_POINT('Ctrl Pts',(-1.89464786547637,-0.625359014479997,
19.9603204373245));
#15548=CARTESIAN_POINT('Ctrl Pts',(-1.8811698387206,-0.664803844915511,
19.963172451783));
#15549=CARTESIAN_POINT('Ctrl Pts',(-1.80943664049553,-0.855040321389873,
19.9771980535711));
#15550=CARTESIAN_POINT('Ctrl Pts',(-1.73423640267897,-0.998789196798814,
19.9886997930666));
#15551=CARTESIAN_POINT('Ctrl Pts',(-1.62836430537238,-1.15242317448586,
20.0011597777289));
#15552=CARTESIAN_POINT('Ctrl Pts',(-1.61382876731584,-1.17269191890948,
20.0028059757612));
#15553=CARTESIAN_POINT('Ctrl Pts',(-1.59561595972442,-1.19710807213246,
20.0047867453344));
#15554=CARTESIAN_POINT('Ctrl Pts',(-1.59229739590086,-1.20151863575145,
20.0051444606489));
#15555=CARTESIAN_POINT('Ctrl Pts',(-1.58707511269118,-1.20839971682064,
20.0057023245488));
#15556=CARTESIAN_POINT('Ctrl Pts',(-1.58518386567472,-1.21087959817152,
20.0059033286226));
#15557=CARTESIAN_POINT('Ctrl Pts',(-1.58164862772257,-1.21549267127319,
20.0062771357978));
#15558=CARTESIAN_POINT('Ctrl Pts',(-1.58000614996346,-1.21762694685455,
20.006450038568));
#15559=CARTESIAN_POINT('Ctrl Pts',(-1.57628001318787,-1.22244854511872,
20.0068405593417));
#15560=CARTESIAN_POINT('Ctrl Pts',(-1.57419380750376,-1.22513386300254,
20.0070579935741));
#15561=CARTESIAN_POINT('Ctrl Pts',(-1.56801802592562,-1.23304137328696,
20.0076981413747));
#15562=CARTESIAN_POINT('Ctrl Pts',(-1.56390920793133,-1.23824858174801,
20.0081195131413));
#15563=CARTESIAN_POINT('Ctrl Pts',(-1.53533827365717,-1.27408817308612,
20.011019232702));
#15564=CARTESIAN_POINT('Ctrl Pts',(-1.51000183529451,-1.30401658030183,
20.0134384331073));
#15565=CARTESIAN_POINT('Ctrl Pts',(-1.36971462689488,-1.46015279329921,
20.026167868741));
#15566=CARTESIAN_POINT('Ctrl Pts',(-1.23979731203901,-1.57196657313992,
20.0357332527269));
#15567=CARTESIAN_POINT('Ctrl Pts',(-1.0469137785901,-1.69900765564511,20.0493668248969));
#15568=CARTESIAN_POINT('Ctrl Pts',(-0.995140993583359,-1.72984073468567,
20.0529719496541));
#15569=CARTESIAN_POINT('Ctrl Pts',(-0.922120102045771,-1.76896398912641,
20.0580409048379));
#15570=CARTESIAN_POINT('Ctrl Pts',(-0.90200492531467,-1.77930495690598,
20.0594355188257));
#15571=CARTESIAN_POINT('Ctrl Pts',(-0.871674559966865,-1.79425093291625,
20.0615381590494));
#15572=CARTESIAN_POINT('Ctrl Pts',(-0.861588918620203,-1.79911574837504,
20.0622373030771));
#15573=CARTESIAN_POINT('Ctrl Pts',(-0.843107877248631,-1.80783905012206,
20.0635186459925));
#15574=CARTESIAN_POINT('Ctrl Pts',(-0.834725559921038,-1.81172463658849,
20.0640998984985));
#15575=CARTESIAN_POINT('Ctrl Pts',(-0.821378830990571,-1.81779916694763,
20.0650256544875));
#15576=CARTESIAN_POINT('Ctrl Pts',(-0.816431890768744,-1.82002636303509,
20.0653688398655));
#15577=CARTESIAN_POINT('Ctrl Pts',(-0.811452372601198,-1.82224383938231,
20.0657143557928));
#15578=CARTESIAN_POINT('Ctrl Pts',(-0.811428779107624,-1.82225434547509,
20.0657159928861));
#15579=CARTESIAN_POINT('Ctrl Pts',(-0.811381288711448,-1.82227549166231,
20.0657192881286));
#15580=CARTESIAN_POINT('Ctrl Pts',(-0.811357391962236,-1.82228613167428,
20.0657209462673));
#15581=CARTESIAN_POINT('Ctrl Pts',(-0.811309290455628,-1.82230754770491,
20.0657242839199));
#15582=CARTESIAN_POINT('Ctrl Pts',(-0.811285085828311,-1.82231832365107,
20.0657259634248));
#15583=CARTESIAN_POINT('Ctrl Pts',(-0.811236363870772,-1.82234001359621,
20.0657293441357));
#15584=CARTESIAN_POINT('Ctrl Pts',(-0.81121184665814,-1.82235092752785,
20.0657310453336));
#15585=CARTESIAN_POINT('Ctrl Pts',(-0.811162494767885,-1.82237289551859,
20.0657344697611));
#15586=CARTESIAN_POINT('Ctrl Pts',(-0.811137660191363,-1.82238394951727,
20.0657361929838));
#15587=CARTESIAN_POINT('Ctrl Pts',(-0.811087668688827,-1.82240619976971,
20.0657396617998));
#15588=CARTESIAN_POINT('Ctrl Pts',(-0.811062511872667,-1.82241739595872,
20.0657414073856));
#15589=CARTESIAN_POINT('Ctrl Pts',(-0.811011871336272,-1.82243993257105,
20.0657449212442));
#15590=CARTESIAN_POINT('Ctrl Pts',(-0.810986387715586,-1.82245127293383,
20.06574668951));
#15591=CARTESIAN_POINT('Ctrl Pts',(-0.806558507015552,-1.82442159490524,
20.0660539330803));
#15592=CARTESIAN_POINT('Ctrl Pts',(-0.80214905969472,-1.82636460394891,
20.0663599532106));
#15593=CARTESIAN_POINT('Ctrl Pts',(-0.792229842600683,-1.83069262432347,
20.0670485029469));
#15594=CARTESIAN_POINT('Ctrl Pts',(-0.786716276654396,-1.83306876766923,
20.0674313319715));
#15595=CARTESIAN_POINT('Ctrl Pts',(-0.77266487932607,-1.83904932854881,
20.0684072753684));
#15596=CARTESIAN_POINT('Ctrl Pts',(-0.76411257462137,-1.84261917309844,
20.0690015574059));
#15597=CARTESIAN_POINT('Ctrl Pts',(-0.715195050354891,-1.86263886677943,
20.0724026295087));
#15598=CARTESIAN_POINT('Ctrl Pts',(-0.674326864209431,-1.87782062308033,
20.0752517724722));
#15599=CARTESIAN_POINT('Ctrl Pts',(-0.442531567006431,-1.95538550791613,
20.091468764879));
#15600=CARTESIAN_POINT('Ctrl Pts',(-0.243544485317435,-1.98998074044987,
20.1057669371418));
#15601=CARTESIAN_POINT('Ctrl Pts',(0.0149965974241431,-1.99553169137539,
20.1234889706565));
#15602=CARTESIAN_POINT('Ctrl Pts',(0.0728444019736701,-1.99425845241336,
20.127386943109));
#15603=CARTESIAN_POINT('Ctrl Pts',(0.137358847003102,-1.99002676398459,
20.1316021771146));
#15604=CARTESIAN_POINT('Ctrl Pts',(0.14415464525435,-1.98954603257756,20.1320445499404));
#15605=CARTESIAN_POINT('Ctrl Pts',(0.154330615376551,-1.98877377594213,
20.1327043492917));
#15606=CARTESIAN_POINT('Ctrl Pts',(0.157712635383516,-1.98850843492736,
20.1329232044504));
#15607=CARTESIAN_POINT('Ctrl Pts',(0.163522320692667,-1.98803771307875,
20.1332983965466));
#15608=CARTESIAN_POINT('Ctrl Pts',(0.165950295365517,-1.98783651181328,
20.1334549672031));
#15609=CARTESIAN_POINT('Ctrl Pts',(0.171015416410893,-1.98740743081919,
20.1337811155609));
#15610=CARTESIAN_POINT('Ctrl Pts',(0.173652468767516,-1.98717875114867,
20.1339506472422));
#15611=CARTESIAN_POINT('Ctrl Pts',(0.18098642003887,-1.98652805592749,20.1344214006493));
#15612=CARTESIAN_POINT('Ctrl Pts',(0.185682328377892,-1.98609462897701,
20.1347219849775));
#15613=CARTESIAN_POINT('Ctrl Pts',(0.204495594539168,-1.98429087825898,
20.1359230190562));
#15614=CARTESIAN_POINT('Ctrl Pts',(0.218600118751808,-1.98278661314207,
20.1368162231703));
#15615=CARTESIAN_POINT('Ctrl Pts',(0.386972575220258,-1.96301093468113,
20.14740523603));
#15616=CARTESIAN_POINT('Ctrl Pts',(0.538637684361655,-1.92692624618761,
20.1562329312064));
#15617=CARTESIAN_POINT('Ctrl Pts',(0.802024509770539,-1.83068703996755,
20.1725392943375));
#15618=CARTESIAN_POINT('Ctrl Pts',(0.915143355373243,-1.77684123458739,
20.1799071661889));
#15619=CARTESIAN_POINT('Ctrl Pts',(1.03276503576493,-1.70662463783894,20.1884146737901));
#15620=CARTESIAN_POINT('Ctrl Pts',(1.04300257482063,-1.7003872772655,20.1891624092736));
#15621=CARTESIAN_POINT('Ctrl Pts',(1.05922868764331,-1.69029962586952,20.1903594957024));
#15622=CARTESIAN_POINT('Ctrl Pts',(1.06525404988323,-1.68650883337295,20.1908066778012));
#15623=CARTESIAN_POINT('Ctrl Pts',(1.07666168239751,-1.67924632042429,20.191658453532));
#15624=CARTESIAN_POINT('Ctrl Pts',(1.08204778591495,-1.67578076443359,20.1920628162118));
#15625=CARTESIAN_POINT('Ctrl Pts',(1.09144223189616,-1.66967196471206,20.1927720062544));
#15626=CARTESIAN_POINT('Ctrl Pts',(1.09545791589045,-1.66704006225553,20.1930764083502));
#15627=CARTESIAN_POINT('Ctrl Pts',(1.10326116963773,-1.66188539435368,20.1936703931438));
#15628=CARTESIAN_POINT('Ctrl Pts',(1.10704968818211,-1.65936411306473,20.1939599187794));
#15629=CARTESIAN_POINT('Ctrl Pts',(1.11599653188098,-1.6533656589976,20.1946463830493));
#15630=CARTESIAN_POINT('Ctrl Pts',(1.12114726076934,-1.64987729232838,20.195043743059));
#15631=CARTESIAN_POINT('Ctrl Pts',(1.13916154660351,-1.6375536833124,20.1964411451163));
#15632=CARTESIAN_POINT('Ctrl Pts',(1.15193739497465,-1.62859181811261,20.1974459903224));
#15633=CARTESIAN_POINT('Ctrl Pts',(1.17061080672154,-1.61516333459023,20.1989355249391));
#15634=CARTESIAN_POINT('Ctrl Pts',(1.17659100265964,-1.610812176584,20.1994157518666));
#15635=CARTESIAN_POINT('Ctrl Pts',(1.31301858295191,-1.51038314581824,20.2104452930694));
#15636=CARTESIAN_POINT('Ctrl Pts',(1.43127827499866,-1.39881974470935,20.2216387844796));
#15637=CARTESIAN_POINT('Ctrl Pts',(1.58463474830905,-1.21411048565386,20.2383891589667));
#15638=CARTESIAN_POINT('Ctrl Pts',(1.63097000502012,-1.15111670860131,20.2438371815435));
#15639=CARTESIAN_POINT('Ctrl Pts',(1.69043175016869,-1.05945122359411,20.2512692480526));
#15640=CARTESIAN_POINT('Ctrl Pts',(1.70675840794183,-1.03294354199485,20.2533639637883));
#15641=CARTESIAN_POINT('Ctrl Pts',(1.73148089291526,-0.990616711170692,
20.2566117704436));
#15642=CARTESIAN_POINT('Ctrl Pts',(1.74029512342846,-0.975048967630145,
20.2577862395534));
#15643=CARTESIAN_POINT('Ctrl Pts',(1.75127700569248,-0.955029244193715,
20.2592691283358));
#15644=CARTESIAN_POINT('Ctrl Pts',(1.75363881324052,-0.950685501046682,
20.2595892447869));
#15645=CARTESIAN_POINT('Ctrl Pts',(1.7574034095743,-0.943700039306297,20.26010137856));
#15646=CARTESIAN_POINT('Ctrl Pts',(1.75881643072066,-0.941063904039953,
20.260294037995));
#15647=CARTESIAN_POINT('Ctrl Pts',(1.76150234204841,-0.936025881358682,
20.2606610656389));
#15648=CARTESIAN_POINT('Ctrl Pts',(1.76277623615511,-0.933624599579384,
20.2608354945467));
#15649=CARTESIAN_POINT('Ctrl Pts',(1.76570560807453,-0.928075383702448,
20.2612374302321));
#15650=CARTESIAN_POINT('Ctrl Pts',(1.76735757764585,-0.924925621570219,
20.2614647134193));
#15651=CARTESIAN_POINT('Ctrl Pts',(1.77263074876813,-0.914805709640665,
20.2621922616264));
#15652=CARTESIAN_POINT('Ctrl Pts',(1.77621926551058,-0.907818475030365,
20.2626905053746));
#15653=CARTESIAN_POINT('Ctrl Pts',(1.82172275233032,-0.817915417753545,
20.2690513521827));
#15654=CARTESIAN_POINT('Ctrl Pts',(1.85784268602966,-0.732178205888365,
20.2745767373536));
#15655=CARTESIAN_POINT('Ctrl Pts',(1.94344577454608,-0.4813238441476,20.2900825155914));
#15656=CARTESIAN_POINT('Ctrl Pts',(1.97771413277032,-0.311927668813766,
20.2998443312433));
#15657=CARTESIAN_POINT('Ctrl Pts',(1.99243410422429,-0.103065153755157,
20.3126263748458));
#15658=CARTESIAN_POINT('Ctrl Pts',(1.99401157475412,-0.0658304146854652,
20.3149298343639));
#15659=CARTESIAN_POINT('Ctrl Pts',(1.9946786197535,-0.0192706417985699,
20.3178495623386));
#15660=CARTESIAN_POINT('Ctrl Pts',(1.99474681062649,-0.0099654660445462,
20.3184350355625));
#15661=CARTESIAN_POINT('Ctrl Pts',(1.99475170100866,0.00480872997366494,
20.3193678440524));
#15662=CARTESIAN_POINT('Ctrl Pts',(1.99473101969195,0.0102776781660031,
20.3197138431944));
#15663=CARTESIAN_POINT('Ctrl Pts',(1.99464981067008,0.020564877771902,20.3203660238381));
#15664=CARTESIAN_POINT('Ctrl Pts',(1.99459431389083,0.0253831386789562,
20.3206720454563));
#15665=CARTESIAN_POINT('Ctrl Pts',(1.99443045653339,0.0362044934741236,
20.3213606129202));
#15666=CARTESIAN_POINT('Ctrl Pts',(1.99431244983192,0.0422073742234864,
20.321743458251));
#15667=CARTESIAN_POINT('Ctrl Pts',(1.99394334663295,0.0574751610892135,
20.3227194705791));
#15668=CARTESIAN_POINT('Ctrl Pts',(1.99365477777623,0.0667389388400438,
20.3233138055254));
#15669=CARTESIAN_POINT('Ctrl Pts',(1.99266731392193,0.0926377164936513,
20.3249815143098));
#15670=CARTESIAN_POINT('Ctrl Pts',(1.99182470320534,0.109266162367065,20.3260593511536));
#15671=CARTESIAN_POINT('Ctrl Pts',(1.98133160514239,0.275210751262127,20.3368886728175));
#15672=CARTESIAN_POINT('Ctrl Pts',(1.95511937340708,0.42297449776889,20.3471770189872));
#15673=CARTESIAN_POINT('Ctrl Pts',(1.8879712910272,0.649727796131091,20.3636706248955));
#15674=CARTESIAN_POINT('Ctrl Pts',(1.8578711453071,0.731367165901559,20.3697508510924));
#15675=CARTESIAN_POINT('Ctrl Pts',(1.80903980370499,0.84113364971112,20.3779395117561));
#15676=CARTESIAN_POINT('Ctrl Pts',(1.79478231045014,0.871141524241555,20.3801789723188));
#15677=CARTESIAN_POINT('Ctrl Pts',(1.77131853760501,0.917501715654971,20.3836251952925));
#15678=CARTESIAN_POINT('Ctrl Pts',(1.76262029176508,0.934103061649808,20.3848564521717));
#15679=CARTESIAN_POINT('Ctrl Pts',(1.75129434072319,0.95499787745647,20.3864002269747));
#15680=CARTESIAN_POINT('Ctrl Pts',(1.74888297380177,0.959406670330965,20.3867256244546));
#15681=CARTESIAN_POINT('Ctrl Pts',(1.74500108018825,0.966440813857832,20.3872441909134));
#15682=CARTESIAN_POINT('Ctrl Pts',(1.74354124880967,0.969071994509439,20.3874380304731));
#15683=CARTESIAN_POINT('Ctrl Pts',(1.74075380771411,0.974069353061834,20.387805915784));
#15684=CARTESIAN_POINT('Ctrl Pts',(1.73942734069538,0.976436096305653,20.3879800279408));
#15685=CARTESIAN_POINT('Ctrl Pts',(1.7363681396033,0.981868446485246,20.3883794056964));
#15686=CARTESIAN_POINT('Ctrl Pts',(1.73463211517322,0.984932174267653,20.3886044569844));
#15687=CARTESIAN_POINT('Ctrl Pts',(1.72909159917604,0.994649965661014,20.3893177444066));
#15688=CARTESIAN_POINT('Ctrl Pts',(1.72525680647491,1.00128680647013,20.3898040690614));
#15689=CARTESIAN_POINT('Ctrl Pts',(1.66205887503232,1.10922185105847,20.397702513933));
#15690=CARTESIAN_POINT('Ctrl Pts',(1.59389398038868,1.20512394107381,20.4045734217356));
#15691=CARTESIAN_POINT('Ctrl Pts',(1.45151610834776,1.37205044870794,20.4173206131978));
#15692=CARTESIAN_POINT('Ctrl Pts',(1.37950954412721,1.44442856191274,20.4231912272128));
#15693=CARTESIAN_POINT('Ctrl Pts',(1.26228600791003,1.54546122065721,20.4323767514708));
#15694=CARTESIAN_POINT('Ctrl Pts',(1.22093359471928,1.57833356897252,20.4355540437508));
#15695=CARTESIAN_POINT('Ctrl Pts',(1.15309023831855,1.62800147221333,20.4407119061672));
#15696=CARTESIAN_POINT('Ctrl Pts',(1.12742252343561,1.64588097243942,20.4426514091995));
#15697=CARTESIAN_POINT('Ctrl Pts',(1.09403386983818,1.66799111822129,20.4451642864853));
#15698=CARTESIAN_POINT('Ctrl Pts',(1.08668984643283,1.67278499889293,20.4457163938856));
#15699=CARTESIAN_POINT('Ctrl Pts',(1.07481535912721,1.68042498449573,20.446608215898));
#15700=CARTESIAN_POINT('Ctrl Pts',(1.0703045850078,1.68330160076405,20.44694679159));
#15701=CARTESIAN_POINT('Ctrl Pts',(1.06169170776679,1.68874559913378,20.4475929117929));
#15702=CARTESIAN_POINT('Ctrl Pts',(1.05759172133641,1.69131627178864,20.4479003314515));
#15703=CARTESIAN_POINT('Ctrl Pts',(1.04821632604041,1.69714718139791,20.4486029785833));
#15704=CARTESIAN_POINT('Ctrl Pts',(1.04293500640171,1.70039777478409,20.4489985575047));
#15705=CARTESIAN_POINT('Ctrl Pts',(1.02672118213745,1.71027324866801,20.4502123390152));
#15706=CARTESIAN_POINT('Ctrl Pts',(1.01574025088417,1.71681760855535,20.4510334720099));
#15707=CARTESIAN_POINT('Ctrl Pts',(0.917374144094689,1.77416728787789,20.4583822378194));
#15708=CARTESIAN_POINT('Ctrl Pts',(0.826321905547917,1.81835947875799,20.4651482406193));
#15709=CARTESIAN_POINT('Ctrl Pts',(0.605075010338799,1.90568285797185,20.4814756537266));
#15710=CARTESIAN_POINT('Ctrl Pts',(0.473003692761791,1.94268050614358,20.4911502714083));
#15711=CARTESIAN_POINT('Ctrl Pts',(0.297829671004234,1.97281581792902,20.5033462977443));
#15712=CARTESIAN_POINT('Ctrl Pts',(0.257261759115728,1.97851500154823,20.5061249824409));
#15713=CARTESIAN_POINT('Ctrl Pts',(0.194962608905754,1.98531823103365,20.5102956576953));
#15714=CARTESIAN_POINT('Ctrl Pts',(0.173342507588657,1.98732266338522,20.5117253456603));
#15715=CARTESIAN_POINT('Ctrl Pts',(0.146427683155607,1.98937537435739,20.5134796909425));
#15716=CARTESIAN_POINT('Ctrl Pts',(0.141160797328923,1.98975603462713,20.5138217830972));
#15717=CARTESIAN_POINT('Ctrl Pts',(0.132833602318584,1.99032464598095,20.5143606679976));
#15718=CARTESIAN_POINT('Ctrl Pts',(0.129774312197578,1.99052646064033,20.5145582245351));
#15719=CARTESIAN_POINT('Ctrl Pts',(0.124019357671447,1.99089277834887,20.5149290472526));
#15720=CARTESIAN_POINT('Ctrl Pts',(0.121323856507004,1.99105885847344,20.5151023973534));
#15721=CARTESIAN_POINT('Ctrl Pts',(0.11515408525755,1.9914264259324,20.5154984224195));
#15722=CARTESIAN_POINT('Ctrl Pts',(0.111679625980287,1.99162429560499,20.5157208922369));
#15723=CARTESIAN_POINT('Ctrl Pts',(0.10096244672493,1.99220650308178,20.5164054709382));
#15724=CARTESIAN_POINT('Ctrl Pts',(0.0937180333631,1.99256043840029,20.516865907245));
#15725=CARTESIAN_POINT('Ctrl Pts',(0.0335271412239369,1.99517214770625,
20.5206734701203));
#15726=CARTESIAN_POINT('Ctrl Pts',(-0.0194934466101668,1.99535889247161,
20.5239118451415));
#15727=CARTESIAN_POINT('Ctrl Pts',(-0.0844524814965636,1.99299755764539,
20.5278057348098));
#15728=CARTESIAN_POINT('Ctrl Pts',(-0.0964374010264595,1.99245359365059,
20.5285210672771));
#15729=CARTESIAN_POINT('Ctrl Pts',(-0.125170213864799,1.99088962186312,
20.5302300962095));
#15730=CARTESIAN_POINT('Ctrl Pts',(-0.141911683615441,1.98976635867055,
20.5312210529331));
#15731=CARTESIAN_POINT('Ctrl Pts',(-0.290806118425057,1.97788754877191,
20.540006184642));
#15732=CARTESIAN_POINT('Ctrl Pts',(-0.421593539049683,1.95419227140571,
20.5475487826682));
#15733=CARTESIAN_POINT('Ctrl Pts',(-0.603448879475862,1.90212436001939,
20.558744292095));
#15734=CARTESIAN_POINT('Ctrl Pts',(-0.657142043551478,1.88424817580111,
20.5621387694196));
#15735=CARTESIAN_POINT('Ctrl Pts',(-0.740710876634706,1.85241867079597,
20.5676172748485));
#15736=CARTESIAN_POINT('Ctrl Pts',(-0.771126394859202,1.83996506003104,
20.5696533426045));
#15737=CARTESIAN_POINT('Ctrl Pts',(-0.809389311769057,1.82318295781121,
20.5722745680411));
#15738=CARTESIAN_POINT('Ctrl Pts',(-0.8175352652182,1.81954478967146,20.5728361093579));
#15739=CARTESIAN_POINT('Ctrl Pts',(-0.8305572653057,1.81362376896694,20.5737395199621));
#15740=CARTESIAN_POINT('Ctrl Pts',(-0.835449015815305,1.8113755787689,20.5740801958878));
#15741=CARTESIAN_POINT('Ctrl Pts',(-0.844714031626783,1.80707197343552,
20.5747279508996));
#15742=CARTESIAN_POINT('Ctrl Pts',(-0.849089053415256,1.8050204129313,20.5750348950033));
#15743=CARTESIAN_POINT('Ctrl Pts',(-0.859006997116744,1.80032559613853,
20.5757331731187));
#15744=CARTESIAN_POINT('Ctrl Pts',(-0.864545233652749,1.79767260945412,
20.5761248426012));
#15745=CARTESIAN_POINT('Ctrl Pts',(-0.878811565815129,1.79075742074562,
20.5771383374503));
#15746=CARTESIAN_POINT('Ctrl Pts',(-0.887520857897589,1.78645700463712,
20.5777614897655));
#15747=CARTESIAN_POINT('Ctrl Pts',(-0.941189212997062,1.75946768302033,
20.5816293786211));
#15748=CARTESIAN_POINT('Ctrl Pts',(-0.985303481227544,1.73514839473152,
20.5849311254791));
#15749=CARTESIAN_POINT('Ctrl Pts',(-1.03949924452423,1.7025378852015,20.5891483143672));
#15750=CARTESIAN_POINT('Ctrl Pts',(-1.05048614523531,1.69578087522475,20.5900117981823));
#15751=CARTESIAN_POINT('Ctrl Pts',(-1.21378610460489,1.5931544266316,20.602973923477));
#15752=CARTESIAN_POINT('Ctrl Pts',(-1.35249743114452,1.47721084274037,20.6157695875899));
#15753=CARTESIAN_POINT('Ctrl Pts',(-1.50040907552634,1.31505319330308,20.6308128725818));
#15754=CARTESIAN_POINT('Ctrl Pts',(-1.52619330470094,1.28503957650769,20.6334938675085));
#15755=CARTESIAN_POINT('Ctrl Pts',(-1.56439614818339,1.23779701381252,20.6375348915239));
#15756=CARTESIAN_POINT('Ctrl Pts',(-1.57745999806839,1.22110474568321,20.6389300467152));
#15757=CARTESIAN_POINT('Ctrl Pts',(-1.59341856218805,1.20003012189358,20.6406479728508));
#15758=CARTESIAN_POINT('Ctrl Pts',(-1.59656475554194,1.19584112266082,20.6409873390003));
#15759=CARTESIAN_POINT('Ctrl Pts',(-1.60152045472826,1.18918843698579,20.6415229084615));
#15760=CARTESIAN_POINT('Ctrl Pts',(-1.60334083569106,1.18673293983441,20.6417198600094));
#15761=CARTESIAN_POINT('Ctrl Pts',(-1.60675994161487,1.18209870785874,20.6420901828289));
#15762=CARTESIAN_POINT('Ctrl Pts',(-1.60835986416405,1.17992093487049,20.6422636352126));
#15763=CARTESIAN_POINT('Ctrl Pts',(-1.61201912293962,1.17491877481369,20.6426607357722));
#15764=CARTESIAN_POINT('Ctrl Pts',(-1.61407546096146,1.17209222628186,20.6428841746914));
#15765=CARTESIAN_POINT('Ctrl Pts',(-1.6204217721527,1.16332050233936,20.6435746964268));
#15766=CARTESIAN_POINT('Ctrl Pts',(-1.62468646825637,1.15735698671764,20.6440400643391));
#15767=CARTESIAN_POINT('Ctrl Pts',(-1.66100985819509,1.10596791605636,20.6480165773126));
#15768=CARTESIAN_POINT('Ctrl Pts',(-1.69119265516384,1.05923910265295,20.6514079180133));
#15769=CARTESIAN_POINT('Ctrl Pts',(-1.79926703275165,0.875494821153208,
20.6641514014759));
#15770=CARTESIAN_POINT('Ctrl Pts',(-1.86277918839679,0.73069352628767,20.6730280035329));
#15771=CARTESIAN_POINT('Ctrl Pts',(-1.92526130054272,0.525056429637518,
20.6857407611268));
#15772=CARTESIAN_POINT('Ctrl Pts',(-1.93955662679941,0.469504650158746,
20.6891795882415));
#15773=CARTESIAN_POINT('Ctrl Pts',(-1.95831579792431,0.380956437260862,
20.6947233178837));
#15774=CARTESIAN_POINT('Ctrl Pts',(-1.96438138607436,0.34833050436023,20.6967787786271));
#15775=CARTESIAN_POINT('Ctrl Pts',(-1.97104627442373,0.30673158863422,20.6994217252029));
#15776=CARTESIAN_POINT('Ctrl Pts',(-1.97240280381546,0.297883968488223,
20.6999851073734));
#15777=CARTESIAN_POINT('Ctrl Pts',(-1.97448073489066,0.283694280298412,
20.7008907794232));
#15778=CARTESIAN_POINT('Ctrl Pts',(-1.97524012111888,0.278357827481949,
20.701231865197));
#15779=CARTESIAN_POINT('Ctrl Pts',(-1.97663906246905,0.268232952779412,
20.7018799471772));
#15780=CARTESIAN_POINT('Ctrl Pts',(-1.97728287118298,0.263445149674797,
20.7021868064467));
#15781=CARTESIAN_POINT('Ctrl Pts',(-1.9787040825883,0.252577289975345,20.7028842704407));
#15782=CARTESIAN_POINT('Ctrl Pts',(-1.97947086257799,0.246495916155972,
20.7032752076468));
#15783=CARTESIAN_POINT('Ctrl Pts',(-1.98137576863466,0.230805657671517,
20.7042855777556));
#15784=CARTESIAN_POINT('Ctrl Pts',(-1.98247201949211,0.221191940618317,
20.7049063239957));
#15785=CARTESIAN_POINT('Ctrl Pts',(-1.98877561538315,0.162095063971895,
20.7087327770602));
#15786=CARTESIAN_POINT('Ctrl Pts',(-1.99219954589707,0.112443290831706,
20.7119940994087));
#15787=CARTESIAN_POINT('Ctrl Pts',(-1.99417609501043,0.0496110026008232,
20.7161836792089));
#15788=CARTESIAN_POINT('Ctrl Pts',(-1.99445915379104,0.0364996015807987,
20.7170613192942));
#15789=CARTESIAN_POINT('Ctrl Pts',(-1.99470984809288,0.0151182046908656,
20.7184979916602));
#15790=CARTESIAN_POINT('Ctrl Pts',(-1.99475537897366,0.00684938086552253,
20.719054926578));
#15791=CARTESIAN_POINT('Ctrl Pts',(-1.9946100620358,-0.197369456595239,
20.7328422358179));
#15792=CARTESIAN_POINT('Ctrl Pts',(-1.96560205531286,-0.392193577328893,
20.7468804505239));
#15793=CARTESIAN_POINT('Ctrl Pts',(-1.89853482066006,-0.613033905744123,
20.7624479192687));
#15794=CARTESIAN_POINT('Ctrl Pts',(-1.88752054710186,-0.646151364402517,
20.7647685248146));
#15795=CARTESIAN_POINT('Ctrl Pts',(-1.8736545560808,-0.684456185077023,
20.7674228128994));
#15796=CARTESIAN_POINT('Ctrl Pts',(-1.87164272227315,-0.68993853859147,
20.7678019826271));
#15797=CARTESIAN_POINT('Ctrl Pts',(-1.86838349125195,-0.698700941296271,
20.7684067565021));
#15798=CARTESIAN_POINT('Ctrl Pts',(-1.86715148340375,-0.701986619699435,
20.7686332489318));
#15799=CARTESIAN_POINT('Ctrl Pts',(-1.86495215540258,-0.707805320815279,
20.7690338279411));
#15800=CARTESIAN_POINT('Ctrl Pts',(-1.8639883341604,-0.710339640300019,
20.7692081220512));
#15801=CARTESIAN_POINT('Ctrl Pts',(-1.86194164043274,-0.715688468442729,
20.769575598871));
#15802=CARTESIAN_POINT('Ctrl Pts',(-1.86085755515423,-0.718502481527094,
20.7697687071209));
#15803=CARTESIAN_POINT('Ctrl Pts',(-1.85793932084751,-0.726026577473509,
20.7702844750227));
#15804=CARTESIAN_POINT('Ctrl Pts',(-1.85609362848988,-0.730732204555316,
20.7706064475051));
#15805=CARTESIAN_POINT('Ctrl Pts',(-1.84720254326062,-0.75314915631005,
20.7721376799633));
#15806=CARTESIAN_POINT('Ctrl Pts',(-1.83992112339173,-0.770766639069918,
20.7733333165269));
#15807=CARTESIAN_POINT('Ctrl Pts',(-1.81894529539213,-0.819525914191428,
20.7766279722166));
#15808=CARTESIAN_POINT('Ctrl Pts',(-1.80470467243861,-0.85042697394291,
20.7786993374704));
#15809=CARTESIAN_POINT('Ctrl Pts',(-1.74995624745865,-0.961650197362051,
20.7861468898134));
#15810=CARTESIAN_POINT('Ctrl Pts',(-1.70481705014267,-1.03957635876646,
20.7913528236881));
#15811=CARTESIAN_POINT('Ctrl Pts',(-1.57339024153744,-1.23474414577757,
20.8049988208855));
#15812=CARTESIAN_POINT('Ctrl Pts',(-1.47929207904489,-1.34604527304376,
20.8134457532166));
#15813=CARTESIAN_POINT('Ctrl Pts',(-1.36524178585288,-1.45440248027703,
20.8231773110015));
#15814=CARTESIAN_POINT('Ctrl Pts',(-1.35646341169134,-1.46259314627146,
20.823923189817));
#15815=CARTESIAN_POINT('Ctrl Pts',(-1.33790159393532,-1.47960141263342,
20.8254942409664));
#15816=CARTESIAN_POINT('Ctrl Pts',(-1.32810372194146,-1.48840233332446,
20.8263200478444));
#15817=CARTESIAN_POINT('Ctrl Pts',(-1.31355905234826,-1.50120909247444,
20.8275412303598));
#15818=CARTESIAN_POINT('Ctrl Pts',(-1.308879409405,-1.50529093983634,20.8279334318287));
#15819=CARTESIAN_POINT('Ctrl Pts',(-1.30050801611161,-1.51252438774131,
20.8286338283504));
#15820=CARTESIAN_POINT('Ctrl Pts',(-1.29682366189243,-1.51568450304025,
20.8289416678805));
#15821=CARTESIAN_POINT('Ctrl Pts',(-1.28909777334214,-1.5222622992407,20.8295863492634));
#15822=CARTESIAN_POINT('Ctrl Pts',(-1.28505410194472,-1.52567740073389,
20.829923293616));
#15823=CARTESIAN_POINT('Ctrl Pts',(-1.27447089750961,-1.53454357170409,
20.8308039444234));
#15824=CARTESIAN_POINT('Ctrl Pts',(-1.26791002823204,-1.53996889534798,
20.8313486934817));
#15825=CARTESIAN_POINT('Ctrl Pts',(-1.23903432563877,-1.56353721434392,
20.8337412327279));
#15826=CARTESIAN_POINT('Ctrl Pts',(-1.21636429349494,-1.58123762998937,
20.8356066694672));
#15827=CARTESIAN_POINT('Ctrl Pts',(-1.15560645527117,-1.62659655852417,
20.8405756204348));
#15828=CARTESIAN_POINT('Ctrl Pts',(-1.11691054209888,-1.65340645121867,
20.8437100519143));
#15829=CARTESIAN_POINT('Ctrl Pts',(-0.91038837707266,-1.78593242263189,
20.8602822007481));
#15830=CARTESIAN_POINT('Ctrl Pts',(-0.728463023318176,-1.86753483391751,
20.874504795066));
#15831=CARTESIAN_POINT('Ctrl Pts',(-0.50650362552567,-1.92964204842676,
20.8900137602047));
#15832=CARTESIAN_POINT('Ctrl Pts',(-0.475287560147974,-1.93756713064289,
20.8921513836738));
#15833=CARTESIAN_POINT('Ctrl Pts',(-0.438336246375368,-1.94600137787034,
20.8946201474641));
#15834=CARTESIAN_POINT('Ctrl Pts',(-0.432775812642055,-1.94724552264663,
20.8949900164422));
#15835=CARTESIAN_POINT('Ctrl Pts',(-0.4238234159628,-1.94920837654142,20.895582807777));
#15836=CARTESIAN_POINT('Ctrl Pts',(-0.420434827394113,-1.9499420861806,
20.8958065644607));
#15837=CARTESIAN_POINT('Ctrl Pts',(-0.414398269748004,-1.95123267656597,
20.8962040452472));
#15838=CARTESIAN_POINT('Ctrl Pts',(-0.411751065246293,-1.95179300764166,
20.8963779656506));
#15839=CARTESIAN_POINT('Ctrl Pts',(-0.406128125515926,-1.9529712605796,
20.8967465648302));
#15840=CARTESIAN_POINT('Ctrl Pts',(-0.40315212482149,-1.95358776704287,
20.8969411617546));
#15841=CARTESIAN_POINT('Ctrl Pts',(-0.395119347344425,-1.95523269514151,
20.8974651271883));
#15842=CARTESIAN_POINT('Ctrl Pts',(-0.390059926392017,-1.95624830889371,
20.897793769896));
#15843=CARTESIAN_POINT('Ctrl Pts',(-0.365121032815253,-1.96115387337369,
20.8994072014873));
#15844=CARTESIAN_POINT('Ctrl Pts',(-0.345186175856508,-1.96476066347969,
20.9006765342936));
#15845=CARTESIAN_POINT('Ctrl Pts',(-0.288619592715493,-1.97410761441455,
20.9042297547318));
#15846=CARTESIAN_POINT('Ctrl Pts',(-0.251876475528161,-1.97913130842792,
20.9064804421477));
#15847=CARTESIAN_POINT('Ctrl Pts',(-0.116588878985594,-1.9937993041374,
20.9146271748516));
#15848=CARTESIAN_POINT('Ctrl Pts',(-0.0175012433060566,-1.99712914866581,
20.9203279107129));
#15849=CARTESIAN_POINT('Ctrl Pts',(0.225683976457441,-1.98719362009591,
20.93445414833));
#15850=CARTESIAN_POINT('Ctrl Pts',(0.368849238669334,-1.96565853077005,
20.942916317776));
#15851=CARTESIAN_POINT('Ctrl Pts',(0.520833112324559,-1.9255973166994,20.9527283576347));
#15852=CARTESIAN_POINT('Ctrl Pts',(0.533206745406368,-1.92220777008531,
20.9535330174232));
#15853=CARTESIAN_POINT('Ctrl Pts',(0.55152045498289,-1.91700060571973,20.954732957018));
#15854=CARTESIAN_POINT('Ctrl Pts',(0.557486293815827,-1.91527417499024,
20.9551252709088));
#15855=CARTESIAN_POINT('Ctrl Pts',(0.568087184320572,-1.91215269859454,
20.9558249630875));
#15856=CARTESIAN_POINT('Ctrl Pts',(0.572725424275385,-1.91076858343534,
20.9561319824491));
#15857=CARTESIAN_POINT('Ctrl Pts',(0.58247486618747,-1.90782052692217,20.9567792043199));
#15858=CARTESIAN_POINT('Ctrl Pts',(0.587584904571797,-1.90625289814548,
20.9571195255037));
#15859=CARTESIAN_POINT('Ctrl Pts',(0.601041792041376,-1.90206541951755,
20.9580186406849));
#15860=CARTESIAN_POINT('Ctrl Pts',(0.609377741369181,-1.89941118775901,
20.9585785594084));
#15861=CARTESIAN_POINT('Ctrl Pts',(0.647225144674249,-1.8870854871126,20.9611344314811));
#15862=CARTESIAN_POINT('Ctrl Pts',(0.676524347806539,-1.87678092742672,
20.963151141521));
#15863=CARTESIAN_POINT('Ctrl Pts',(0.754480109971616,-1.84730117953563,
20.9686235246129));
#15864=CARTESIAN_POINT('Ctrl Pts',(0.802640332179603,-1.82689068730709,
20.9721184201241));
#15865=CARTESIAN_POINT('Ctrl Pts',(0.941846148511684,-1.76132729666965,
20.9825559635148));
#15866=CARTESIAN_POINT('Ctrl Pts',(1.03030424240772,-1.71108675512941,20.9896351315254));
#15867=CARTESIAN_POINT('Ctrl Pts',(1.21290803591734,-1.58806450054347,21.0049958740511));
#15868=CARTESIAN_POINT('Ctrl Pts',(1.30517895326536,-1.51314563847197,21.0132515933771));
#15869=CARTESIAN_POINT('Ctrl Pts',(1.39573191626292,-1.42513800682212,21.0214969120381));
#15870=CARTESIAN_POINT('Ctrl Pts',(1.4011796000356,-1.41978225569463,21.0219935012636));
#15871=CARTESIAN_POINT('Ctrl Pts',(1.4090899295764,-1.41191554244734,21.0227151990423));
#15872=CARTESIAN_POINT('Ctrl Pts',(1.41157683404156,-1.40942923579045,21.0229421823796));
#15873=CARTESIAN_POINT('Ctrl Pts',(1.41597030656416,-1.40501352688308,21.0233433206312));
#15874=CARTESIAN_POINT('Ctrl Pts',(1.41787952821951,-1.40308679831506,21.0235176850901));
#15875=CARTESIAN_POINT('Ctrl Pts',(1.42190022054802,-1.39901264994102,21.023884975909));
#15876=CARTESIAN_POINT('Ctrl Pts',(1.42401075449825,-1.39686434676299,21.0240778290937));
#15877=CARTESIAN_POINT('Ctrl Pts',(1.42963789061094,-1.39111050255342,21.0245921935277));
#15878=CARTESIAN_POINT('Ctrl Pts',(1.43314574539413,-1.38749637922964,21.0249130241341));
#15879=CARTESIAN_POINT('Ctrl Pts',(1.44972671799818,-1.37028312579255,21.0264306411278));
#15880=CARTESIAN_POINT('Ctrl Pts',(1.46262072175605,-1.35651173559781,21.0276140957702));
#15881=CARTESIAN_POINT('Ctrl Pts',(1.49788040817889,-1.31776539128471,21.0308666699606));
#15882=CARTESIAN_POINT('Ctrl Pts',(1.51981562555559,-1.29240553945169,21.0329089855605));
#15883=CARTESIAN_POINT('Ctrl Pts',(1.59705604680829,-1.19841810458524,21.0402218338353));
#15884=CARTESIAN_POINT('Ctrl Pts',(1.6484401232475,-1.12669484232694,21.045327754139));
#15885=CARTESIAN_POINT('Ctrl Pts',(1.77290117628542,-0.926133810089712,
21.0590172826626));
#15886=CARTESIAN_POINT('Ctrl Pts',(1.83665920948988,-0.792198367766934,
21.0676016713935));
#15887=CARTESIAN_POINT('Ctrl Pts',(1.88920826161322,-0.640377274174271,
21.0775399959862));
#15888=CARTESIAN_POINT('Ctrl Pts',(1.89327240423629,-0.628259898985119,
21.0783342255829));
#15889=CARTESIAN_POINT('Ctrl Pts',(1.90113095664229,-0.604060432197417,
21.0799229024063));
#15890=CARTESIAN_POINT('Ctrl Pts',(1.90492731057444,-0.591979602429236,
21.0807172436709));
#15891=CARTESIAN_POINT('Ctrl Pts',(1.91040418666343,-0.573952586946305,
21.0819047266506));
#15892=CARTESIAN_POINT('Ctrl Pts',(1.91217257300423,-0.568033254430364,
21.0822949924822));
#15893=CARTESIAN_POINT('Ctrl Pts',(1.91527628550666,-0.557465428217436,
21.0829923908085));
#15894=CARTESIAN_POINT('Ctrl Pts',(1.916622262665,-0.552820092854428,21.0832991730387));
#15895=CARTESIAN_POINT('Ctrl Pts',(1.91942506882256,-0.543013561396558,
21.0839472989757));
#15896=CARTESIAN_POINT('Ctrl Pts',(1.92087800236137,-0.537851300828639,
21.0842887667269));
#15897=CARTESIAN_POINT('Ctrl Pts',(1.92466755075472,-0.524175844298953,
21.0851941488291));
#15898=CARTESIAN_POINT('Ctrl Pts',(1.92696847776183,-0.515652962980549,
21.0857592163292));
#15899=CARTESIAN_POINT('Ctrl Pts',(1.93731611958467,-0.476287544190206,
21.0883731017618));
#15900=CARTESIAN_POINT('Ctrl Pts',(1.94467902536546,-0.445271675272963,
21.0904438463828));
#15901=CARTESIAN_POINT('Ctrl Pts',(1.96254928289318,-0.361063408537297,
21.0960999470022));
#15902=CARTESIAN_POINT('Ctrl Pts',(1.97163577217638,-0.307600343180028,
21.0997278388892));
#15903=CARTESIAN_POINT('Ctrl Pts',(1.99165227990602,-0.151581874465548,
21.1104140314671));
#15904=CARTESIAN_POINT('Ctrl Pts',(1.99682328000519,-0.0484705651595451,
21.1176078296984));
#15905=CARTESIAN_POINT('Ctrl Pts',(1.99379232062132,0.0622841673958293,
21.125335662298));
#15906=CARTESIAN_POINT('Ctrl Pts',(1.99353639737591,0.0699983432818144,
21.1258738519295));
#15907=CARTESIAN_POINT('Ctrl Pts',(1.98909753291257,0.183852493546946,21.1338148660226));
#15908=CARTESIAN_POINT('Ctrl Pts',(1.9764871354067,0.289508541748631,21.1411657672692));
#15909=CARTESIAN_POINT('Ctrl Pts',(1.95397852476055,0.401318295830868,21.148615230746));
#15910=CARTESIAN_POINT('Ctrl Pts',(1.95239367482064,0.408958913811939,21.1491225711915));
#15911=CARTESIAN_POINT('Ctrl Pts',(1.95002321099888,0.420059068435008,21.1498569194152));
#15912=CARTESIAN_POINT('Ctrl Pts',(1.9492731648176,0.423526001336987,21.1500858947915));
#15913=CARTESIAN_POINT('Ctrl Pts',(1.94793230925023,0.429644809430461,21.1504893119248));
#15914=CARTESIAN_POINT('Ctrl Pts',(1.94734532519913,0.432297499965828,21.1506639713979));
#15915=CARTESIAN_POINT('Ctrl Pts',(1.94609970927008,0.437872650808429,21.1510305523355));
#15916=CARTESIAN_POINT('Ctrl Pts',(1.9454399146961,0.440794822275182,21.1512224057161));
#15917=CARTESIAN_POINT('Ctrl Pts',(1.9436689804174,0.448556701140902,21.1517312705918));
#15918=CARTESIAN_POINT('Ctrl Pts',(1.94254633909445,0.453393803799022,21.1520476267737));
#15919=CARTESIAN_POINT('Ctrl Pts',(1.93724556342371,0.47585202186095,21.1535131104189));
#15920=CARTESIAN_POINT('Ctrl Pts',(1.93284548940349,0.493420601163006,21.1546499918112));
#15921=CARTESIAN_POINT('Ctrl Pts',(1.88853711373006,0.660637459966116,21.1654007722305));
#15922=CARTESIAN_POINT('Ctrl Pts',(1.83156112754935,0.80524075626327,21.1741895899601));
#15923=CARTESIAN_POINT('Ctrl Pts',(1.69804571279293,1.05452216612797,21.1906474539205));
#15924=CARTESIAN_POINT('Ctrl Pts',(1.62698926676855,1.16115251718609,21.1982054511876));
#15925=CARTESIAN_POINT('Ctrl Pts',(1.53800063199992,1.27033504213925,21.2069966860118));
#15926=CARTESIAN_POINT('Ctrl Pts',(1.52967688789764,1.28034591777179,21.207813127801));
#15927=CARTESIAN_POINT('Ctrl Pts',(1.51725793794711,1.29498807506561,21.2090230532045));
#15928=CARTESIAN_POINT('Ctrl Pts',(1.5132381278138,1.29968308904885,21.2094134471023));
#15929=CARTESIAN_POINT('Ctrl Pts',(1.50602527257307,1.30802865501071,21.210111782075));
#15930=CARTESIAN_POINT('Ctrl Pts',(1.50284059824372,1.31168640289811,21.2104193751378));
#15931=CARTESIAN_POINT('Ctrl Pts',(1.4961430018652,1.3193224959066,21.2110647405154));
#15932=CARTESIAN_POINT('Ctrl Pts',(1.49262748267046,1.32329850272519,21.2114026198667));
#15933=CARTESIAN_POINT('Ctrl Pts',(1.48338819313383,1.33366435904992,21.2122883855493));
#15934=CARTESIAN_POINT('Ctrl Pts',(1.47763904447411,1.34003134461906,21.212837336993));
#15935=CARTESIAN_POINT('Ctrl Pts',(1.45201974401431,1.36803850222311,21.2152740314479));
#15936=CARTESIAN_POINT('Ctrl Pts',(1.43171486662948,1.38927429546161,21.2171802351394));
#15937=CARTESIAN_POINT('Ctrl Pts',(1.37669986162268,1.44432426930366,21.2222833051189));
#15938=CARTESIAN_POINT('Ctrl Pts',(1.3412157213491,1.47733369619487,21.225513191772));
#15939=CARTESIAN_POINT('Ctrl Pts',(1.14722572461027,1.64504095987245,21.2428521327635));
#15940=CARTESIAN_POINT('Ctrl Pts',(0.969608390870513,1.75559930403204,21.2578261174242));
#15941=CARTESIAN_POINT('Ctrl Pts',(0.758076266883175,1.84521612858551,21.2731232882376));
#15942=CARTESIAN_POINT('Ctrl Pts',(0.737877424147387,1.85338587215017,21.2745587947379));
#15943=CARTESIAN_POINT('Ctrl Pts',(0.712426568041568,1.8631978082461,21.2763326532876));
#15944=CARTESIAN_POINT('Ctrl Pts',(0.707297145329823,1.86515104949738,21.2766884023554));
#15945=CARTESIAN_POINT('Ctrl Pts',(0.699216112055657,1.86819010836508,21.2772460241247));
#15946=CARTESIAN_POINT('Ctrl Pts',(0.696269932511647,1.86929014167604,21.2774487308661));
#15947=CARTESIAN_POINT('Ctrl Pts',(0.690860328089097,1.87129539550569,21.2778198302121));
#15948=CARTESIAN_POINT('Ctrl Pts',(0.688397740493991,1.87220271370261,21.2779883454065));
#15949=CARTESIAN_POINT('Ctrl Pts',(0.682866618728271,1.87422821699942,21.2783659072095));
#15950=CARTESIAN_POINT('Ctrl Pts',(0.679797134702418,1.87534372433257,21.2785747925397));
#15951=CARTESIAN_POINT('Ctrl Pts',(0.673378296120105,1.87765861892346,21.2790102967682));
#15952=CARTESIAN_POINT('Ctrl Pts',(0.670028440402363,1.87885659602409,21.2792368325837));
#15953=CARTESIAN_POINT('Ctrl Pts',(0.661295213569867,1.88195345024514,21.2798255284858));
#15954=CARTESIAN_POINT('Ctrl Pts',(0.655906819036435,1.88383820828055,21.2801868837038));
#15955=CARTESIAN_POINT('Ctrl Pts',(0.639905861027281,1.88935806265989,21.2812546084325));
#15956=CARTESIAN_POINT('Ctrl Pts',(0.629270445442786,1.89292686584507,21.2819573690833));
#15957=CARTESIAN_POINT('Ctrl Pts',(0.492998142387599,1.9373787206482,21.2908804117389));
#15958=CARTESIAN_POINT('Ctrl Pts',(0.363612019889337,1.96577718373651,21.2984846259256));
#15959=CARTESIAN_POINT('Ctrl Pts',(0.0807314232905281,1.99895350571148,
21.3150051523248));
#15960=CARTESIAN_POINT('Ctrl Pts',(-0.0724047272334247,1.99927015113472,
21.323913934323));
#15961=CARTESIAN_POINT('Ctrl Pts',(-0.236652603846043,1.98070277337642,
21.3342347931947));
#15962=CARTESIAN_POINT('Ctrl Pts',(-0.249222069166602,1.97916049875238,
21.3350291622058));
#15963=CARTESIAN_POINT('Ctrl Pts',(-0.267900292353994,1.97668792755281,
21.3362166786983));
#15964=CARTESIAN_POINT('Ctrl Pts',(-0.274020957726963,1.97584873988561,
21.336606950056));
#15965=CARTESIAN_POINT('Ctrl Pts',(-0.284926072165954,1.97430192396778,
21.3373043545567));
#15966=CARTESIAN_POINT('Ctrl Pts',(-0.289712052823314,1.97360529978933,
21.3376111374119));
#15967=CARTESIAN_POINT('Ctrl Pts',(-0.299799455714704,1.9720995432572,21.338259260838));
#15968=CARTESIAN_POINT('Ctrl Pts',(-0.30510023537524,1.97128642454866,21.3386007254386));
#15969=CARTESIAN_POINT('Ctrl Pts',(-0.319117912143108,1.96907827446178,
21.3395060903192));
#15970=CARTESIAN_POINT('Ctrl Pts',(-0.327828861419671,1.96764674834489,
21.3400711436698));
#15971=CARTESIAN_POINT('Ctrl Pts',(-0.367945671243436,1.96078030631115,
21.3426848677974));
#15972=CARTESIAN_POINT('Ctrl Pts',(-0.399226427436191,1.95465124531873,
21.3447554619619));
#15973=CARTESIAN_POINT('Ctrl Pts',(-0.483275315968002,1.93608131477752,
21.350411048117));
#15974=CARTESIAN_POINT('Ctrl Pts',(-0.535702070232386,1.92223523459837,
21.3540385665032));
#15975=CARTESIAN_POINT('Ctrl Pts',(-0.681220041163365,1.87738789108652,
21.3643833192158));
#15976=CARTESIAN_POINT('Ctrl Pts',(-0.772679098247907,1.84163247082297,
21.3712174510201));
#15977=CARTESIAN_POINT('Ctrl Pts',(-0.893370244615706,1.78387069910344,
21.3805522947377));
#15978=CARTESIAN_POINT('Ctrl Pts',(-0.925190250563382,1.76757691118878,
21.3830441283775));
#15979=CARTESIAN_POINT('Ctrl Pts',(-1.02954274245299,1.71055173330923,21.3912898174433));
#15980=CARTESIAN_POINT('Ctrl Pts',(-1.09997358277768,1.66613538522129,21.3969795042038));
#15981=CARTESIAN_POINT('Ctrl Pts',(-1.17377049805303,1.6128705706331,21.4029241522094));
#15982=CARTESIAN_POINT('Ctrl Pts',(-1.18008167613837,1.60825865527067,21.403432374985));
#15983=CARTESIAN_POINT('Ctrl Pts',(-1.1892192744445,1.60149857301408,21.4041677601809));
#15984=CARTESIAN_POINT('Ctrl Pts',(-1.19206722919607,1.5993798434493,21.404396897909));
#15985=CARTESIAN_POINT('Ctrl Pts',(-1.19704267703937,1.59565769785177,21.4047970745962));
#15986=CARTESIAN_POINT('Ctrl Pts',(-1.19917263184068,1.59405760835466,21.4049683441796));
#15987=CARTESIAN_POINT('Ctrl Pts',(-1.20362893308726,1.5906959070808,21.4053265767195));
#15988=CARTESIAN_POINT('Ctrl Pts',(-1.20595461654526,1.58893346005113,21.4055134790407));
#15989=CARTESIAN_POINT('Ctrl Pts',(-1.2119853985493,1.58434235094546,21.4059980224421));
#15990=CARTESIAN_POINT('Ctrl Pts',(-1.21568449108141,1.58150577314775,21.40629511083));
#15991=CARTESIAN_POINT('Ctrl Pts',(-1.22380616509327,1.57523249137289,21.4069472233459));
#15992=CARTESIAN_POINT('Ctrl Pts',(-1.22822430173893,1.57179006167214,21.4073018561508));
#15993=CARTESIAN_POINT('Ctrl Pts',(-1.24121725117295,1.56157825514952,21.4083446316888));
#15994=CARTESIAN_POINT('Ctrl Pts',(-1.24975117467722,1.55475687007307,21.4090293630749));
#15995=CARTESIAN_POINT('Ctrl Pts',(-1.27968530665324,1.53042401491538,21.4114322802541));
#15996=CARTESIAN_POINT('Ctrl Pts',(-1.30077794136407,1.51253729155804,21.4131274972556));
#15997=CARTESIAN_POINT('Ctrl Pts',(-1.40638286874237,1.41913976159621,21.4216657757238));
#15998=CARTESIAN_POINT('Ctrl Pts',(-1.48472803919417,1.33695835454334,21.4281796005928));
#15999=CARTESIAN_POINT('Ctrl Pts',(-1.64581356421066,1.1362500414249,21.4431171330949));
#16000=CARTESIAN_POINT('Ctrl Pts',(-1.72351187809355,1.01452686542029,21.4515594516503));
#16001=CARTESIAN_POINT('Ctrl Pts',(-1.79312880497959,0.874003190847164,
21.4613493612533));
#16002=CARTESIAN_POINT('Ctrl Pts',(-1.79871842421699,0.862441016507123,
21.4621548235912));
#16003=CARTESIAN_POINT('Ctrl Pts',(-1.80684603313699,0.845206234413241,
21.4633557314999));
#16004=CARTESIAN_POINT('Ctrl Pts',(-1.80946986351918,0.839574283640657,
21.4637482040969));
#16005=CARTESIAN_POINT('Ctrl Pts',(-1.81409102551261,0.829532848004732,
21.4644480744782));
#16006=CARTESIAN_POINT('Ctrl Pts',(-1.81609870769831,0.825128158520763,
21.4647551126643));
#16007=CARTESIAN_POINT('Ctrl Pts',(-1.82028894971991,0.815845731621414,
21.4654022666595));
#16008=CARTESIAN_POINT('Ctrl Pts',(-1.82246797844415,0.810966451159789,
21.4657425007329));
#16009=CARTESIAN_POINT('Ctrl Pts',(-1.82816011398378,0.798081817633999,
21.4666411397859));
#16010=CARTESIAN_POINT('Ctrl Pts',(-1.83164021465107,0.790062092519377,
21.4672006673437));
#16011=CARTESIAN_POINT('Ctrl Pts',(-1.84721845289589,0.753506604056222,
21.4697521872498));
#16012=CARTESIAN_POINT('Ctrl Pts',(-1.85870265210972,0.724715451980229,
21.4717648499011));
#16013=CARTESIAN_POINT('Ctrl Pts',(-1.88769758749171,0.64679579237316,21.477223555745));
#16014=CARTESIAN_POINT('Ctrl Pts',(-1.90395925273267,0.597231404802596,
21.4807085808336));
#16015=CARTESIAN_POINT('Ctrl Pts',(-1.9690839704532,0.368885002774501,21.4968136172544));
#16016=CARTESIAN_POINT('Ctrl Pts',(-1.99482013392882,0.184503243835848,
21.5100601477585));
#16017=CARTESIAN_POINT('Ctrl Pts',(-1.99474985647505,-0.000756698609384009,
21.5225779118923));
#16018=CARTESIAN_POINT('',(-1.99474917376081,0.00181556617883987,22.3209548813952));
#16019=CARTESIAN_POINT('Ctrl Pts',(-1.9947498118588,-0.000866365563652432,
21.5209548813952));
#16020=CARTESIAN_POINT('Ctrl Pts',(-1.99472877578325,-0.0493005479633061,
21.524063142322));
#16021=CARTESIAN_POINT('Ctrl Pts',(-1.99294386346395,-0.0976946259360165,
21.5271714032488));
#16022=CARTESIAN_POINT('Ctrl Pts',(-1.989402859888,-0.145958293938546,21.5302796641756));
#16023=CARTESIAN_POINT('Ctrl Pts',(-1.98432871476336,-0.215118590007016,
21.5347337028936));
#16024=CARTESIAN_POINT('Ctrl Pts',(-1.97563375315188,-0.284150938386916,
21.5391877416116));
#16025=CARTESIAN_POINT('Ctrl Pts',(-1.96333095162286,-0.352645908667128,
21.5436417803296));
#16026=CARTESIAN_POINT('Ctrl Pts',(-1.95104664311606,-0.421037920364781,
21.5480891239353));
#16027=CARTESIAN_POINT('Ctrl Pts',(-1.93516534412893,-0.488893679248685,
21.5525364675411));
#16028=CARTESIAN_POINT('Ctrl Pts',(-1.91575188852089,-0.555807758247975,
21.5569838111469));
#16029=CARTESIAN_POINT('Ctrl Pts',(-1.89636131938151,-0.622642952426204,
21.5614259117917));
#16030=CARTESIAN_POINT('Ctrl Pts',(-1.87344699969841,-0.688538203701612,
21.5658680124364));
#16031=CARTESIAN_POINT('Ctrl Pts',(-1.84712466402983,-0.753098956334872,
21.5703101130812));
#16032=CARTESIAN_POINT('Ctrl Pts',(-1.8208189326072,-0.817618983759374,
21.5747494116293));
#16033=CARTESIAN_POINT('Ctrl Pts',(-1.79110963429111,-0.880805730216488,
21.5791887101773));
#16034=CARTESIAN_POINT('Ctrl Pts',(-1.75816163279785,-0.942281929922031,
21.5836280087253));
#16035=CARTESIAN_POINT('Ctrl Pts',(-1.72522321924043,-1.00374023992769,
21.5880660154284));
#16036=CARTESIAN_POINT('Ctrl Pts',(-1.68904820459707,-1.06348856006338,
21.5925040221314));
#16037=CARTESIAN_POINT('Ctrl Pts',(-1.64984788249783,-1.1211732814857,21.5969420288345));
#16038=CARTESIAN_POINT('Ctrl Pts',(-1.61064564779819,-1.17886081737014,
21.6013802520698));
#16039=CARTESIAN_POINT('Ctrl Pts',(-1.56841808973195,-1.2344841510782,21.6058184753051));
#16040=CARTESIAN_POINT('Ctrl Pts',(-1.52341939076268,-1.28771927156048,
21.6102566985404));
#16041=CARTESIAN_POINT('Ctrl Pts',(-1.47837302063779,-1.34101078877803,
21.6146996235834));
#16042=CARTESIAN_POINT('Ctrl Pts',(-1.43054996672539,-1.39190866828392,
21.6191425486265));
#16043=CARTESIAN_POINT('Ctrl Pts',(-1.38024358553733,-1.44012333051133,
21.6235854736695));
#16044=CARTESIAN_POINT('Ctrl Pts',(-1.32990783844394,-1.48836613762162,
21.6280309922308));
#16045=CARTESIAN_POINT('Ctrl Pts',(-1.27708624961189,-1.5339222900707,21.632476510792));
#16046=CARTESIAN_POINT('Ctrl Pts',(-1.22210568159205,-1.57654218640683,
21.6369220293533));
#16047=CARTESIAN_POINT('Ctrl Pts',(-1.16702917094622,-1.61923645565182,
21.6413753054685));
#16048=CARTESIAN_POINT('Ctrl Pts',(-1.10978656263195,-1.65898396146875,
21.6458285815837));
#16049=CARTESIAN_POINT('Ctrl Pts',(-1.05073345595025,-1.69557859359183,
21.650281857699));
#16050=CARTESIAN_POINT('Ctrl Pts',(-1.01911221549959,-1.71517396674983,
21.6526664589968));
#16051=CARTESIAN_POINT('Ctrl Pts',(-0.986972274373024,-1.73386610538307,
21.6550510602946));
#16052=CARTESIAN_POINT('Ctrl Pts',(-0.954370742035125,-1.75162897020097,
21.6574356615924));
#16053=CARTESIAN_POINT('Ctrl Pts',(-0.893476500539938,-1.78480704811022,
21.6618897003104));
#16054=CARTESIAN_POINT('Ctrl Pts',(-0.830729479086657,-1.81487162492435,
21.6663437390284));
#16055=CARTESIAN_POINT('Ctrl Pts',(-0.766480935041935,-1.84161194031675,
21.6707977777464));
#16056=CARTESIAN_POINT('Ctrl Pts',(-0.702328966541362,-1.86831206086041,
21.6752451213521));
#16057=CARTESIAN_POINT('Ctrl Pts',(-0.636680403370564,-1.89169765097144,
21.6796924649579));
#16058=CARTESIAN_POINT('Ctrl Pts',(-0.569911213208941,-1.91160371718584,
21.6841398085636));
#16059=CARTESIAN_POINT('Ctrl Pts',(-0.503220737059332,-1.93148631619431,
21.6885819092084));
#16060=CARTESIAN_POINT('Ctrl Pts',(-0.435412724688168,-1.94789739920132,
21.6930240098532));
#16061=CARTESIAN_POINT('Ctrl Pts',(-0.366881561862411,-1.96072065375601,
21.697466110498));
#16062=CARTESIAN_POINT('Ctrl Pts',(-0.298393628797768,-1.97353581934492,
21.701905409046));
#16063=CARTESIAN_POINT('Ctrl Pts',(-0.229183930300444,-1.98276755635265,
21.706344707594));
#16064=CARTESIAN_POINT('Ctrl Pts',(-0.159658914585722,-1.98835021902413,
21.7107840061421));
#16065=CARTESIAN_POINT('Ctrl Pts',(-0.0901541307927484,-1.99393125712935,
21.7152220128451));
#16066=CARTESIAN_POINT('Ctrl Pts',(-0.0203346996770724,-1.99586528974961,
21.7196600195482));
#16067=CARTESIAN_POINT('Ctrl Pts',(0.04938768259161,-1.99413851557715,21.7240980262513));
#16068=CARTESIAN_POINT('Ctrl Pts',(0.119113466645032,-1.99241165715464,
21.7285362494866));
#16069=CARTESIAN_POINT('Ctrl Pts',(0.188741703099653,-1.9870236518403,21.7329744727219));
#16070=CARTESIAN_POINT('Ctrl Pts',(0.257862359831198,-1.97801278203208,
21.7374126959572));
#16071=CARTESIAN_POINT('Ctrl Pts',(0.327056242270525,-1.96899236620172,
21.7418556210002));
#16072=CARTESIAN_POINT('Ctrl Pts',(0.395740985292811,-1.95634148877475,
21.7462985460433));
#16073=CARTESIAN_POINT('Ctrl Pts',(0.463514296007958,-1.94015000963746,
21.7507414710863));
#16074=CARTESIAN_POINT('Ctrl Pts',(0.531327168794214,-1.92394907886734,
21.7551869896475));
#16075=CARTESIAN_POINT('Ctrl Pts',(0.598227080627999,-1.90420357129347,
21.7596325082088));
#16076=CARTESIAN_POINT('Ctrl Pts',(0.663827209953822,-1.88105316188164,
21.7640780267701));
#16077=CARTESIAN_POINT('Ctrl Pts',(0.729541813336523,-1.85786235435916,
21.7685313028853));
#16078=CARTESIAN_POINT('Ctrl Pts',(0.793951654136786,-1.83125497129768,
21.7729845790005));
#16079=CARTESIAN_POINT('Ctrl Pts',(0.856690917923904,-1.80141839494513,
21.7774378551158));
#16080=CARTESIAN_POINT('Ctrl Pts',(0.890285989502041,-1.78544176631252,
21.7798224564136));
#16081=CARTESIAN_POINT('Ctrl Pts',(0.923402490549147,-1.76854001431263,
21.7822070577113));
#16082=CARTESIAN_POINT('Ctrl Pts',(0.955987608595106,-1.75074705617705,
21.7845916590091));
#16083=CARTESIAN_POINT('Ctrl Pts',(1.016851190923,-1.71751276895384,21.7890456977271));
#16084=CARTESIAN_POINT('Ctrl Pts',(1.07610019080042,-1.68103505666552,21.7934997364451));
#16085=CARTESIAN_POINT('Ctrl Pts',(1.13336723499775,-1.64149513344802,21.7979537751631));
#16086=CARTESIAN_POINT('Ctrl Pts',(1.19054819792991,-1.60201464487856,21.8024011187688));
#16087=CARTESIAN_POINT('Ctrl Pts',(1.24575271854935,-1.55948135703953,21.8068484623746));
#16088=CARTESIAN_POINT('Ctrl Pts',(1.29863852400445,-1.51412203816982,21.8112958059804));
#16089=CARTESIAN_POINT('Ctrl Pts',(1.35146198253106,-1.46881619327457,21.8157379066251));
#16090=CARTESIAN_POINT('Ctrl Pts',(1.40197178521234,-1.42069125150546,21.8201800072699));
#16091=CARTESIAN_POINT('Ctrl Pts',(1.44985661635391,-1.37001582272425,21.8246221079147));
#16092=CARTESIAN_POINT('Ctrl Pts',(1.49771124153186,-1.31937236022801,21.8290614064627));
#16093=CARTESIAN_POINT('Ctrl Pts',(1.54294384452758,-1.26618195732962,21.8335007050108));
#16094=CARTESIAN_POINT('Ctrl Pts',(1.58527917729993,-1.21075079703433,21.8379400035588));
#16095=CARTESIAN_POINT('Ctrl Pts',(1.62760219040385,-1.15533576732006,21.8423780102618));
#16096=CARTESIAN_POINT('Ctrl Pts',(1.66702930999776,-1.09768166352848,21.8468160169649));
#16097=CARTESIAN_POINT('Ctrl Pts',(1.70332603534491,-1.03812715011996,21.851254023668));
#16098=CARTESIAN_POINT('Ctrl Pts',(1.73962453162478,-0.978569731021327,
21.8556922469033));
#16099=CARTESIAN_POINT('Ctrl Pts',(1.77279207768687,-0.917112137501394,
21.8601304701386));
#16100=CARTESIAN_POINT('Ctrl Pts',(1.80263886349575,-0.854119833697089,
21.8645686933739));
#16101=CARTESIAN_POINT('Ctrl Pts',(1.83251726868036,-0.791060796498634,
21.8690116184169));
#16102=CARTESIAN_POINT('Ctrl Pts',(1.85906768185369,-0.726464247178823,
21.87345454346));
#16103=CARTESIAN_POINT('Ctrl Pts',(1.88214784725472,-0.660717067718424,
21.877897468503));
#16104=CARTESIAN_POINT('Ctrl Pts',(1.9052414854983,-0.594931508923145,21.8823429870642));
#16105=CARTESIAN_POINT('Ctrl Pts',(1.92486070625319,-0.527994453044673,
21.8867885056255));
#16106=CARTESIAN_POINT('Ctrl Pts',(1.94091351252505,-0.460306744896983,
21.8912340241867));
#16107=CARTESIAN_POINT('Ctrl Pts',(1.95699433139197,-0.392500919809078,
21.895687300302));
#16108=CARTESIAN_POINT('Ctrl Pts',(1.96949622475257,-0.323942309207001,
21.9001405764172));
#16109=CARTESIAN_POINT('Ctrl Pts',(1.97837867937509,-0.255039925294245,
21.9045938525325));
#16110=CARTESIAN_POINT('Ctrl Pts',(1.98313497839465,-0.218144680119672,
21.9069784538303));
#16111=CARTESIAN_POINT('Ctrl Pts',(1.98685436922854,-0.181150923968879,
21.9093630551281));
#16112=CARTESIAN_POINT('Ctrl Pts',(1.98953677474743,-0.144121422514414,
21.9117476564259));
#16113=CARTESIAN_POINT('Ctrl Pts',(1.99454706223212,-0.0749564709830513,
21.9162016951439));
#16114=CARTESIAN_POINT('Ctrl Pts',(1.99595626162719,-0.00539296304012958,
21.9206557338619));
#16115=CARTESIAN_POINT('Ctrl Pts',(1.99371782986213,0.0641621180278543,
21.9251097725799));
#16116=CARTESIAN_POINT('Ctrl Pts',(1.99148276280781,0.133612647002035,21.9295571161856));
#16117=CARTESIAN_POINT('Ctrl Pts',(1.98561096251939,0.203054288922361,21.9340044597914));
#16118=CARTESIAN_POINT('Ctrl Pts',(1.97610777552311,0.272076500302983,21.9384518033971));
#16119=CARTESIAN_POINT('Ctrl Pts',(1.96661579180746,0.34101734159118,21.9428939040419));
#16120=CARTESIAN_POINT('Ctrl Pts',(1.9535009905037,0.409539251765541,21.9473360046867));
#16121=CARTESIAN_POINT('Ctrl Pts',(1.93682065736895,0.477235061252748,21.9517781053315));
#16122=CARTESIAN_POINT('Ctrl Pts',(1.92015084626223,0.544888167923446,21.9562174038795));
#16123=CARTESIAN_POINT('Ctrl Pts',(1.89992008198059,0.611715733424842,21.9606567024275));
#16124=CARTESIAN_POINT('Ctrl Pts',(1.87623676763892,0.677320569789411,21.9650960009756));
#16125=CARTESIAN_POINT('Ctrl Pts',(1.85256034519017,0.742906315012403,21.9695340076786));
#16126=CARTESIAN_POINT('Ctrl Pts',(1.82543353331394,0.807269577211512,21.9739720143817));
#16127=CARTESIAN_POINT('Ctrl Pts',(1.79501410522617,0.870029841177362,21.9784100210848));
#16128=CARTESIAN_POINT('Ctrl Pts',(1.76459319296152,0.932793167243267,21.9828482443201));
#16129=CARTESIAN_POINT('Ctrl Pts',(1.73087956121856,0.993952900301384,21.9872864675554));
#16130=CARTESIAN_POINT('Ctrl Pts',(1.69407771131804,1.05315158952329,21.9917246907907));
#16131=CARTESIAN_POINT('Ctrl Pts',(1.65723687391894,1.11241299322336,21.9961676158337));
#16132=CARTESIAN_POINT('Ctrl Pts',(1.61730154733726,1.16970878987996,22.0006105408767));
#16133=CARTESIAN_POINT('Ctrl Pts',(1.57451998655462,1.22470991440424,22.0050534659197));
#16134=CARTESIAN_POINT('Ctrl Pts',(1.531713452414,1.27974314534883,22.009498984481));
#16135=CARTESIAN_POINT('Ctrl Pts',(1.48605769765005,1.33247866781368,22.0139445030422));
#16136=CARTESIAN_POINT('Ctrl Pts',(1.4378399272931,1.38262211250283,22.0183900216035));
#16137=CARTESIAN_POINT('Ctrl Pts',(1.38953801558089,1.43285305890269,22.0228432977187));
#16138=CARTESIAN_POINT('Ctrl Pts',(1.33866552111773,1.48048256375399,22.027296573834));
#16139=CARTESIAN_POINT('Ctrl Pts',(1.28554438964709,1.52525512120002,22.0317498499492));
#16140=CARTESIAN_POINT('Ctrl Pts',(1.25709955133765,1.54922953819746,22.034134451247));
#16141=CARTESIAN_POINT('Ctrl Pts',(1.22801049480845,1.57238550184667,22.0365190525448));
#16142=CARTESIAN_POINT('Ctrl Pts',(1.19832994901216,1.5946889652219,22.0389036538426));
#16143=CARTESIAN_POINT('Ctrl Pts',(1.14289162468103,1.63634812623567,22.0433576925606));
#16144=CARTESIAN_POINT('Ctrl Pts',(1.08516853929668,1.67519542850972,22.0478117312785));
#16145=CARTESIAN_POINT('Ctrl Pts',(1.02547766814925,1.71097139503476,22.0522657699965));
#16146=CARTESIAN_POINT('Ctrl Pts',(0.965876521655493,1.7466935847235,22.0567131136023));
#16147=CARTESIAN_POINT('Ctrl Pts',(0.904313876563793,1.7793533520302,22.061160457208));
#16148=CARTESIAN_POINT('Ctrl Pts',(0.84113779507104,1.80873291898031,22.0656078008138));
#16149=CARTESIAN_POINT('Ctrl Pts',(0.778036191684482,1.83807785044091,22.0700499014586));
#16150=CARTESIAN_POINT('Ctrl Pts',(0.713325371423766,1.8641500564919,22.0744920021034));
#16151=CARTESIAN_POINT('Ctrl Pts',(0.64737868035834,1.88677725413402,22.0789341027481));
#16152=CARTESIAN_POINT('Ctrl Pts',(0.581473588757775,1.90939017843962,22.0833734012962));
#16153=CARTESIAN_POINT('Ctrl Pts',(0.514334634872293,1.92856224680548,22.0878126998442));
#16154=CARTESIAN_POINT('Ctrl Pts',(0.446354448204243,1.94416955769508,22.0922519983922));
#16155=CARTESIAN_POINT('Ctrl Pts',(0.378394043909549,1.95977232682529,22.0966900050953));
#16156=CARTESIAN_POINT('Ctrl Pts',(0.309593369703032,1.97181228829576,22.1011280117983));
#16157=CARTESIAN_POINT('Ctrl Pts',(0.240357766897769,1.98021607568263,22.1055660185014));
#16158=CARTESIAN_POINT('Ctrl Pts',(0.171118786057906,1.98862027309387,22.1100042417367));
#16159=CARTESIAN_POINT('Ctrl Pts',(0.101445320770596,1.9933878875812,22.114442464972));
#16160=CARTESIAN_POINT('Ctrl Pts',(0.0317486199466149,1.99449732705549,
22.1188806882073));
#16161=CARTESIAN_POINT('Ctrl Pts',(-0.0380219168402537,1.99560794185846,
22.1233236132503));
#16162=CARTESIAN_POINT('Ctrl Pts',(-0.107815247820187,1.99305263866246,
22.1277665382934));
#16163=CARTESIAN_POINT('Ctrl Pts',(-0.177220300856193,1.98686197997356,
22.1322094633364));
#16164=CARTESIAN_POINT('Ctrl Pts',(-0.246665868478446,1.98066770754236,
22.1366549818977));
#16165=CARTESIAN_POINT('Ctrl Pts',(-0.315722222209281,1.97083392484672,
22.1411005004589));
#16166=CARTESIAN_POINT('Ctrl Pts',(-0.383986372642777,1.95744272665247,
22.1455460190202));
#16167=CARTESIAN_POINT('Ctrl Pts',(-0.452369645924388,1.94402816044355,
22.1499992951354));
#16168=CARTESIAN_POINT('Ctrl Pts',(-0.519957481606996,1.92704390617596,
22.1544525712506));
#16169=CARTESIAN_POINT('Ctrl Pts',(-0.58636075597997,1.90662230825788,22.1589058473659));
#16170=CARTESIAN_POINT('Ctrl Pts',(-0.62191779986246,1.89568712983211,22.1612904486637));
#16171=CARTESIAN_POINT('Ctrl Pts',(-0.65713551031104,1.88376719975309,22.1636750499615));
#16172=CARTESIAN_POINT('Ctrl Pts',(-0.691956714037148,1.8708884168755,22.1660596512594));
#16173=CARTESIAN_POINT('Ctrl Pts',(-0.756996932602777,1.84683299191644,
22.1705136899774));
#16174=CARTESIAN_POINT('Ctrl Pts',(-0.820910056479831,1.81933426328133,
22.1749677286953));
#16175=CARTESIAN_POINT('Ctrl Pts',(-0.88330631424359,1.78851824640326,22.1794217674133));
#16176=CARTESIAN_POINT('Ctrl Pts',(-0.945608780737224,1.75774855078654,
22.1838691110191));
#16177=CARTESIAN_POINT('Ctrl Pts',(-1.00639847115222,1.72367167871072,22.1883164546248));
#16178=CARTESIAN_POINT('Ctrl Pts',(-1.0653038420214,1.68646235851099,22.1927637982306));
#16179=CARTESIAN_POINT('Ctrl Pts',(-1.12413976951322,1.64929690427501,22.1972058988754));
#16180=CARTESIAN_POINT('Ctrl Pts',(-1.1810953775753,1.60900659653896,22.2016479995202));
#16181=CARTESIAN_POINT('Ctrl Pts',(-1.23582368399509,1.56581205276266,22.206090100165));
#16182=CARTESIAN_POINT('Ctrl Pts',(-1.29051746755672,1.52264475629594,22.210529398713));
#16183=CARTESIAN_POINT('Ctrl Pts',(-1.34298635325931,1.47657716066309,22.214968697261));
#16184=CARTESIAN_POINT('Ctrl Pts',(-1.39291359569009,1.4278722903123,22.219407995809));
#16185=CARTESIAN_POINT('Ctrl Pts',(-1.44282630919121,1.3791815931784,22.2238460025121));
#16186=CARTESIAN_POINT('Ctrl Pts',(-1.4901984974338,1.32785548652114,22.2282840092151));
#16187=CARTESIAN_POINT('Ctrl Pts',(-1.53474902045629,1.27419504264789,22.2327220159182));
#16188=CARTESIAN_POINT('Ctrl Pts',(-1.57930171711783,1.22053198065866,22.2371602391535));
#16189=CARTESIAN_POINT('Ctrl Pts',(-1.62103216435493,1.16453473352599,22.2415984623888));
#16190=CARTESIAN_POINT('Ctrl Pts',(-1.65969955342409,1.10653737165261,22.2460366856241));
#16191=CARTESIAN_POINT('Ctrl Pts',(-1.69840790632471,1.0484785679748,22.2504796106671));
#16192=CARTESIAN_POINT('Ctrl Pts',(-1.73404645213506,0.988415828474916,
22.2549225357102));
#16193=CARTESIAN_POINT('Ctrl Pts',(-1.76641832718732,0.926711312047483,
22.2593654607532));
#16194=CARTESIAN_POINT('Ctrl Pts',(-1.7988090990355,0.864970776153984,22.2638109793144));
#16195=CARTESIAN_POINT('Ctrl Pts',(-1.82792920023711,0.8015870007953,22.2682564978757));
#16196=CARTESIAN_POINT('Ctrl Pts',(-1.85362946934576,0.736943249424911,
22.2727020164369));
#16197=CARTESIAN_POINT('Ctrl Pts',(-1.87937458614142,0.672186692903873,
22.2771552925522));
#16198=CARTESIAN_POINT('Ctrl Pts',(-1.90168780150769,0.606166235125184,
22.2816085686674));
#16199=CARTESIAN_POINT('Ctrl Pts',(-1.9204697088147,0.539280687606346,22.2860618447827));
#16200=CARTESIAN_POINT('Ctrl Pts',(-1.93052688007029,0.503465400323477,
22.2884464460804));
#16201=CARTESIAN_POINT('Ctrl Pts',(-1.93957239482412,0.467402253967104,
22.2908310473782));
#16202=CARTESIAN_POINT('Ctrl Pts',(-1.94759707343737,0.431153339356435,
22.293215648676));
#16203=CARTESIAN_POINT('Ctrl Pts',(-1.96820349956193,0.338070411426196,
22.2993390229378));
#16204=CARTESIAN_POINT('Ctrl Pts',(-1.98214332905318,0.243462071757729,
22.3054623971996));
#16205=CARTESIAN_POINT('Ctrl Pts',(-1.98924225493863,0.148131069214597,
22.3115857714614));
#16206=CARTESIAN_POINT('Ctrl Pts',(-1.99286284135548,0.0995104555497706,
22.314708808106));
#16207=CARTESIAN_POINT('Ctrl Pts',(-1.99470467848154,0.0507022014321492,
22.3178318447506));
#16208=CARTESIAN_POINT('Ctrl Pts',(-1.99474917376081,0.00181556617883987,
22.3209548813952));
#16209=CARTESIAN_POINT('',(-1.99474923905662,-0.00174234986216392,23.9213503181716));
#16210=CARTESIAN_POINT('Ctrl Pts',(-1.99474916465735,0.00182554069043293,
22.3211268459801));
#16211=CARTESIAN_POINT('Ctrl Pts',(-1.99487395450769,-0.134531019874973,
22.3290365499321));
#16212=CARTESIAN_POINT('Ctrl Pts',(-1.98101782205593,-0.270531511972645,
22.3369252531668));
#16213=CARTESIAN_POINT('Ctrl Pts',(-1.94710944369394,-0.434461115772628,
22.3471604031875));
#16214=CARTESIAN_POINT('Ctrl Pts',(-1.94011124694327,-0.464714787064044,
22.3490789461331));
#16215=CARTESIAN_POINT('Ctrl Pts',(-1.93038366978814,-0.502705870542994,
22.3515307718075));
#16216=CARTESIAN_POINT('Ctrl Pts',(-1.92830864928981,-0.510607534976442,
22.3520430636427));
#16217=CARTESIAN_POINT('Ctrl Pts',(-1.92474835120962,-0.523833850233449,
22.3529046033478));
#16218=CARTESIAN_POINT('Ctrl Pts',(-1.92328936086948,-0.529165523732292,
22.3532530023818));
#16219=CARTESIAN_POINT('Ctrl Pts',(-1.92037199803809,-0.539655151635728,
22.3539406561053));
#16220=CARTESIAN_POINT('Ctrl Pts',(-1.91891495862294,-0.544813430629328,
22.3542798651057));
#16221=CARTESIAN_POINT('Ctrl Pts',(-1.91610356291509,-0.554615267846382,
22.3549264708628));
#16222=CARTESIAN_POINT('Ctrl Pts',(-1.91475307036602,-0.559259902005289,
22.3552337396913));
#16223=CARTESIAN_POINT('Ctrl Pts',(-1.91163787845738,-0.569830160003168,
22.3559350334784));
#16224=CARTESIAN_POINT('Ctrl Pts',(-1.90986250206253,-0.575752560910539,
22.3563294049467));
#16225=CARTESIAN_POINT('Ctrl Pts',(-1.90435976351267,-0.593803372294288,
22.3575358739453));
#16226=CARTESIAN_POINT('Ctrl Pts',(-1.90054424744259,-0.60590436950045,
22.3583508506658));
#16227=CARTESIAN_POINT('Ctrl Pts',(-1.84952423541691,-0.762490572959903,
22.368978717291));
#16228=CARTESIAN_POINT('Ctrl Pts',(-1.7860807614038,-0.901126382508468,
22.3793579959026));
#16229=CARTESIAN_POINT('Ctrl Pts',(-1.67596060795108,-1.08347321158767,
22.3941981638717));
#16230=CARTESIAN_POINT('Ctrl Pts',(-1.64200104140563,-1.13427988143001,
22.3984709038721));
#16231=CARTESIAN_POINT('Ctrl Pts',(-1.5583125971607,-1.24783265163207,22.4082529300103));
#16232=CARTESIAN_POINT('Ctrl Pts',(-1.50702614251558,-1.3093126967328,22.413728134514));
#16233=CARTESIAN_POINT('Ctrl Pts',(-1.44522760339684,-1.37493548274255,
22.4196396335748));
#16234=CARTESIAN_POINT('Ctrl Pts',(-1.43821863180487,-1.38226538151872,
22.4203009061064));
#16235=CARTESIAN_POINT('Ctrl Pts',(-1.42899124246175,-1.3917691007664,22.4211591902352));
#16236=CARTESIAN_POINT('Ctrl Pts',(-1.42682338304109,-1.39399147587231,
22.4213599586059));
#16237=CARTESIAN_POINT('Ctrl Pts',(-1.42255686900396,-1.39834490110462,
22.4217533562102));
#16238=CARTESIAN_POINT('Ctrl Pts',(-1.42045859312581,-1.40047630951062,
22.4219460137397));
#16239=CARTESIAN_POINT('Ctrl Pts',(-1.41644414808854,-1.40453584041459,
22.4223130400321));
#16240=CARTESIAN_POINT('Ctrl Pts',(-1.41452885499875,-1.40646474186768,
22.4224874694846));
#16241=CARTESIAN_POINT('Ctrl Pts',(-1.41009838865867,-1.41090848283683,
22.42288940945));
#16242=CARTESIAN_POINT('Ctrl Pts',(-1.4075804287362,-1.41342051412752,22.4231166963572));
#16243=CARTESIAN_POINT('Ctrl Pts',(-1.39948008423508,-1.42145867217602,
22.423844268479));
#16244=CARTESIAN_POINT('Ctrl Pts',(-1.39387168546872,-1.42695865119918,
22.4243425322353));
#16245=CARTESIAN_POINT('Ctrl Pts',(-1.31909535599593,-1.49942790603792,
22.4309160123608));
#16246=CARTESIAN_POINT('Ctrl Pts',(-1.24518908697355,-1.56134754712361,
22.436628900454));
#16247=CARTESIAN_POINT('Ctrl Pts',(-1.09135981255622,-1.67232807643898,
22.4477112811479));
#16248=CARTESIAN_POINT('Ctrl Pts',(-1.01188806633998,-1.72157781333676,
22.4530741377689));
#16249=CARTESIAN_POINT('Ctrl Pts',(-0.864721201832706,-1.79905649938952,
22.4628163271807));
#16250=CARTESIAN_POINT('Ctrl Pts',(-0.798374361419991,-1.82946549577,22.4671451795131));
#16251=CARTESIAN_POINT('Ctrl Pts',(-0.706530623005226,-1.86561154098105,
22.473161268282));
#16252=CARTESIAN_POINT('Ctrl Pts',(-0.682365869914973,-1.87458493319584,
22.4747459691639));
#16253=CARTESIAN_POINT('Ctrl Pts',(-0.640980396582672,-1.88904686650893,
22.4774672084792));
#16254=CARTESIAN_POINT('Ctrl Pts',(-0.623846252970294,-1.89477432734875,
22.4785958978355));
#16255=CARTESIAN_POINT('Ctrl Pts',(-0.601395855381872,-1.9019413392695,
22.4800783362717));
#16256=CARTESIAN_POINT('Ctrl Pts',(-0.596147741509026,-1.90359284044834,
22.4804251284474));
#16257=CARTESIAN_POINT('Ctrl Pts',(-0.585790564057796,-1.90680505443428,
22.4811100490443));
#16258=CARTESIAN_POINT('Ctrl Pts',(-0.580681928207997,-1.90836699769781,
22.48144813397));
#16259=CARTESIAN_POINT('Ctrl Pts',(-0.570931946440271,-1.91130523754168,
22.4820938825083));
#16260=CARTESIAN_POINT('Ctrl Pts',(-0.566291737200668,-1.91268519788796,
22.4824014236653));
#16261=CARTESIAN_POINT('Ctrl Pts',(-0.555681758800476,-1.91579852491365,
22.4831051418711));
#16262=CARTESIAN_POINT('Ctrl Pts',(-0.549708841161825,-1.91752089783329,
22.4835016742704));
#16263=CARTESIAN_POINT('Ctrl Pts',(-0.531356591316559,-1.92272022723358,
22.4847212477045));
#16264=CARTESIAN_POINT('Ctrl Pts',(-0.518951804649607,-1.92610537378607,
22.4855472600358));
#16265=CARTESIAN_POINT('Ctrl Pts',(-0.404201076652255,-1.95623075228686,
22.4932049159982));
#16266=CARTESIAN_POINT('Ctrl Pts',(-0.299929795218202,-1.97490576431392,
22.500298653188));
#16267=CARTESIAN_POINT('Ctrl Pts',(-0.0623218021041458,-1.99820717833908,
22.5167200655941));
#16268=CARTESIAN_POINT('Ctrl Pts',(0.0709996732814402,-1.99791713716561,
22.5261210426059));
#16269=CARTESIAN_POINT('Ctrl Pts',(0.243327821427617,-1.98026221060951,
22.5380005699284));
#16270=CARTESIAN_POINT('Ctrl Pts',(0.283228240406341,-1.9749503930941,22.5407293573752));
#16271=CARTESIAN_POINT('Ctrl Pts',(0.344040504107337,-1.96497347873874,
22.5448293420469));
#16272=CARTESIAN_POINT('Ctrl Pts',(0.365081916101651,-1.96117309968721,
22.5462370083217));
#16273=CARTESIAN_POINT('Ctrl Pts',(0.391207605213068,-1.9560193531349,22.5479677705432));
#16274=CARTESIAN_POINT('Ctrl Pts',(0.396352069611487,-1.95498341134752,
22.5483077513314));
#16275=CARTESIAN_POINT('Ctrl Pts',(0.404511858954576,-1.95330673991214,
22.5488456259945));
#16276=CARTESIAN_POINT('Ctrl Pts',(0.40752984465648,-1.95267931065289,22.5490442647244));
#16277=CARTESIAN_POINT('Ctrl Pts',(0.41318653923977,-1.95148961693505,22.5494160003781));
#16278=CARTESIAN_POINT('Ctrl Pts',(0.415825531454692,-1.95092900145483,
22.5495891862112));
#16279=CARTESIAN_POINT('Ctrl Pts',(0.421840281774882,-1.94963849655661,
22.5499833736897));
#16280=CARTESIAN_POINT('Ctrl Pts',(0.425215279774653,-1.94890519442826,
22.5502041772537));
#16281=CARTESIAN_POINT('Ctrl Pts',(0.435541167469643,-1.94663353888735,
22.5508786055035));
#16282=CARTESIAN_POINT('Ctrl Pts',(0.44248583561854,-1.9450667166557,22.5513306286604));
#16283=CARTESIAN_POINT('Ctrl Pts',(0.497300725493365,-1.93239087664798,
22.5548871962136));
#16284=CARTESIAN_POINT('Ctrl Pts',(0.544758553400688,-1.9195524363302,22.5578983500583));
#16285=CARTESIAN_POINT('Ctrl Pts',(0.762528660113038,-1.85191150700659,
22.5716023927544));
#16286=CARTESIAN_POINT('Ctrl Pts',(0.925453263414701,-1.77611166426968,
22.581599861375));
#16287=CARTESIAN_POINT('Ctrl Pts',(1.11632211931106,-1.65382427314641,22.5951108083804));
#16288=CARTESIAN_POINT('Ctrl Pts',(1.1556059033512,-1.62661743942888,22.5979956596301));
#16289=CARTESIAN_POINT('Ctrl Pts',(1.21709308396422,-1.58068089018479,22.6027126656628));
#16290=CARTESIAN_POINT('Ctrl Pts',(1.23993104127373,-1.5628302943425,22.6045119884421));
#16291=CARTESIAN_POINT('Ctrl Pts',(1.2687859998665,-1.53924601365169,22.6068510977748));
#16292=CARTESIAN_POINT('Ctrl Pts',(1.27516809100609,-1.53396301791901,22.6073727035432));
#16293=CARTESIAN_POINT('Ctrl Pts',(1.28564224884653,-1.52518213608453,22.6082358857634));
#16294=CARTESIAN_POINT('Ctrl Pts',(1.28975343932334,-1.52170713512081,22.6085765265738));
#16295=CARTESIAN_POINT('Ctrl Pts',(1.29752835917773,-1.5150812092403,22.6092242536879));
#16296=CARTESIAN_POINT('Ctrl Pts',(1.30119480910814,-1.5119335241797,22.6095312051768));
#16297=CARTESIAN_POINT('Ctrl Pts',(1.30949530691094,-1.50475490576425,22.6102295536084));
#16298=CARTESIAN_POINT('Ctrl Pts',(1.31412223074216,-1.50071584469483,22.6106212862797));
#16299=CARTESIAN_POINT('Ctrl Pts',(1.3260205553458,-1.49023201457492,22.6116350508912));
#16300=CARTESIAN_POINT('Ctrl Pts',(1.33326358602594,-1.48375542967492,22.612258410958));
#16301=CARTESIAN_POINT('Ctrl Pts',(1.35187761188666,-1.46686476298206,22.6138767940778));
#16302=CARTESIAN_POINT('Ctrl Pts',(1.36317551915813,-1.45637144718114,22.6148751541644));
#16303=CARTESIAN_POINT('Ctrl Pts',(1.49057246350765,-1.33526598134491,22.6263200324392));
#16304=CARTESIAN_POINT('Ctrl Pts',(1.59302573901624,-1.21119372229919,22.6373921507008));
#16305=CARTESIAN_POINT('Ctrl Pts',(1.72228372922423,-1.00948098766119,22.6541076937224));
#16306=CARTESIAN_POINT('Ctrl Pts',(1.76104324387832,-0.940234594272093,
22.6596386027489));
#16307=CARTESIAN_POINT('Ctrl Pts',(1.80925582585188,-0.840599037396781,
22.6671696654947));
#16308=CARTESIAN_POINT('Ctrl Pts',(1.8222635334276,-0.812015536752611,22.6692831825295));
#16309=CARTESIAN_POINT('Ctrl Pts',(1.84165860881691,-0.766580160989994,
22.6725568652198));
#16310=CARTESIAN_POINT('Ctrl Pts',(1.84850140832012,-0.749929446026353,
22.6737388031703));
#16311=CARTESIAN_POINT('Ctrl Pts',(1.8569394428166,-0.72857945417306,22.6752297170721));
#16312=CARTESIAN_POINT('Ctrl Pts',(1.85874357280237,-0.723964396346133,
22.6755505422672));
#16313=CARTESIAN_POINT('Ctrl Pts',(1.86160996844704,-0.716550659800417,
22.6760635394373));
#16314=CARTESIAN_POINT('Ctrl Pts',(1.8626831493131,-0.713756266688654,22.6762563573176));
#16315=CARTESIAN_POINT('Ctrl Pts',(1.86471862599565,-0.708420350863957,
22.6766234977335));
#16316=CARTESIAN_POINT('Ctrl Pts',(1.86568200652061,-0.705879308576643,
22.6767978817389));
#16317=CARTESIAN_POINT('Ctrl Pts',(1.86789254083851,-0.700012595232482,
22.677199463264));
#16318=CARTESIAN_POINT('Ctrl Pts',(1.86913600683422,-0.696685557505772,
22.677426438475));
#16319=CARTESIAN_POINT('Ctrl Pts',(1.87245111052919,-0.687742850226298,
22.678034520194));
#16320=CARTESIAN_POINT('Ctrl Pts',(1.87450638966861,-0.682121093825888,
22.6784146699298));
#16321=CARTESIAN_POINT('Ctrl Pts',(1.88937661409514,-0.640872127323986,
22.6811890930592));
#16322=CARTESIAN_POINT('Ctrl Pts',(1.90120120440005,-0.604892969929968,
22.6835279541159));
#16323=CARTESIAN_POINT('Ctrl Pts',(1.9361116318199,-0.487501113056454,22.690965121051));
#16324=CARTESIAN_POINT('Ctrl Pts',(1.95504633017762,-0.404946698496029,
22.6959007483728));
#16325=CARTESIAN_POINT('Ctrl Pts',(1.98491678741861,-0.221999158367863,
22.7066647979654));
#16326=CARTESIAN_POINT('Ctrl Pts',(1.99359468472123,-0.121480026991771,
22.7124727196927));
#16327=CARTESIAN_POINT('Ctrl Pts',(1.99517545653653,0.0305468418019273,
22.7215078341762));
#16328=CARTESIAN_POINT('Ctrl Pts',(1.99373045347125,0.0818320573321208,
22.7245971045408));
#16329=CARTESIAN_POINT('Ctrl Pts',(1.98826916154383,0.163557734931406,22.7296244118648));
#16330=CARTESIAN_POINT('Ctrl Pts',(1.98552399057693,0.194061111342069,22.7315240064004));
#16331=CARTESIAN_POINT('Ctrl Pts',(1.98109816598418,0.233138167037473,22.7339920070998));
#16332=CARTESIAN_POINT('Ctrl Pts',(1.98006185089138,0.241781742423838,22.7345400801569));
#16333=CARTESIAN_POINT('Ctrl Pts',(1.97829918228246,0.255711509741991,22.7354269470858));
#16334=CARTESIAN_POINT('Ctrl Pts',(1.97760813189825,0.261002119879242,22.7357646250052));
#16335=CARTESIAN_POINT('Ctrl Pts',(1.97624940024058,0.271089139639613,22.7364100684452));
#16336=CARTESIAN_POINT('Ctrl Pts',(1.97558546153878,0.275886021861949,22.7367177135068));
#16337=CARTESIAN_POINT('Ctrl Pts',(1.97402761923951,0.286847204205327,22.7374223351988));
#16338=CARTESIAN_POINT('Ctrl Pts',(1.97312230030656,0.293009806421168,22.7378196704677));
#16339=CARTESIAN_POINT('Ctrl Pts',(1.97025015172648,0.311943707031555,22.7390441330497));
#16340=CARTESIAN_POINT('Ctrl Pts',(1.96818810705046,0.324700013760337,22.7398742664013));
#16341=CARTESIAN_POINT('Ctrl Pts',(1.9473228653218,0.446267415820006,22.7478362360987));
#16342=CARTESIAN_POINT('Ctrl Pts',(1.91964232292156,0.553341513907452,22.7552548186305));
#16343=CARTESIAN_POINT('Ctrl Pts',(1.82651577628048,0.820055639187041,22.7747219809042));
#16344=CARTESIAN_POINT('Ctrl Pts',(1.74898915740276,0.974519898479016,22.7870015472129));
#16345=CARTESIAN_POINT('Ctrl Pts',(1.64226378352394,1.13240353731302,22.7996368929803));
#16346=CARTESIAN_POINT('Ctrl Pts',(1.63171701388448,1.14754858402196,22.8008490518177));
#16347=CARTESIAN_POINT('Ctrl Pts',(1.61804810445454,1.16660742205184,22.8023723836902));
#16348=CARTESIAN_POINT('Ctrl Pts',(1.61511978651685,1.17065820034293,22.8026960324628));
#16349=CARTESIAN_POINT('Ctrl Pts',(1.61040777531065,1.17712504765559,22.8032124690612));
#16350=CARTESIAN_POINT('Ctrl Pts',(1.60863382234227,1.1795481365798,22.8034059179874));
#16351=CARTESIAN_POINT('Ctrl Pts',(1.60524577815102,1.18415409649484,22.8037735149481));
#16352=CARTESIAN_POINT('Ctrl Pts',(1.60363272266733,1.18633765150904,22.8039477275079));
#16353=CARTESIAN_POINT('Ctrl Pts',(1.59991026973095,1.19135518293681,22.8043479318962));
#16354=CARTESIAN_POINT('Ctrl Pts',(1.59779779913364,1.19418685165022,22.8045737064086));
#16355=CARTESIAN_POINT('Ctrl Pts',(1.59212493318368,1.20174906429766,22.8051764789548));
#16356=CARTESIAN_POINT('Ctrl Pts',(1.58855094706958,1.2064694389381,22.8055525461816));
#16357=CARTESIAN_POINT('Ctrl Pts',(1.56278310013225,1.2401895365013,22.8082382091873));
#16358=CARTESIAN_POINT('Ctrl Pts',(1.53981593869398,1.26859307402303,22.8104962928574));
#16359=CARTESIAN_POINT('Ctrl Pts',(1.4667283614622,1.35406879227771,22.8173348484934));
#16360=CARTESIAN_POINT('Ctrl Pts',(1.41411676423863,1.40892513374242,22.8217871962587));
#16361=CARTESIAN_POINT('Ctrl Pts',(1.28219245229713,1.53162336391116,22.8322689832983));
#16362=CARTESIAN_POINT('Ctrl Pts',(1.20044215311522,1.59650415665228,22.8382584351856));
#16363=CARTESIAN_POINT('Ctrl Pts',(1.06777988036323,1.68581673644667,22.8477295656777));
#16364=CARTESIAN_POINT('Ctrl Pts',(1.02028094304673,1.71498046362059,22.8510749061639));
#16365=CARTESIAN_POINT('Ctrl Pts',(0.943235443344064,1.75795086202701,22.8564810489308));
#16366=CARTESIAN_POINT('Ctrl Pts',(0.914463069262987,1.7730881084232,22.8584955028114));
#16367=CARTESIAN_POINT('Ctrl Pts',(0.877370059248215,1.7914598356594,22.8610925049177));
#16368=CARTESIAN_POINT('Ctrl Pts',(0.869379031980131,1.79535140245078,22.8616519737826));
#16369=CARTESIAN_POINT('Ctrl Pts',(0.856513180651841,1.80151093198391,22.8625528384647));
#16370=CARTESIAN_POINT('Ctrl Pts',(0.85165466865916,1.80381284814027,22.8628930529684));
#16371=CARTESIAN_POINT('Ctrl Pts',(0.842410455150029,1.80814699391779,22.8635404428854));
#16372=CARTESIAN_POINT('Ctrl Pts',(0.838026549818965,1.81018298182334,22.8638474855249));
#16373=CARTESIAN_POINT('Ctrl Pts',(0.828044612911843,1.81477479364279,22.8645466948078));
#16374=CARTESIAN_POINT('Ctrl Pts',(0.822442087992473,1.81732067701587,22.8649392003359));
#16375=CARTESIAN_POINT('Ctrl Pts',(0.805385364236191,1.82497651701979,22.8661344171093));
#16376=CARTESIAN_POINT('Ctrl Pts',(0.793894843269383,1.83000432744978,22.8669399296299));
#16377=CARTESIAN_POINT('Ctrl Pts',(0.637986272532171,1.89647920221075,22.8778757303823));
#16378=CARTESIAN_POINT('Ctrl Pts',(0.48688591149088,1.94076831641874,22.8886133361283));
#16379=CARTESIAN_POINT('Ctrl Pts',(0.242528399290034,1.98203857291557,22.9058881910641));
#16380=CARTESIAN_POINT('Ctrl Pts',(0.151928392206219,1.9910338931163,22.9122583810231));
#16381=CARTESIAN_POINT('Ctrl Pts',(0.0267241362351118,1.99486621983656,
22.9208052199254));
#16382=CARTESIAN_POINT('Ctrl Pts',(-0.00760323781957737,1.99503080134012,
22.9231213435121));
#16383=CARTESIAN_POINT('Ctrl Pts',(-0.0610970543308081,1.99390637768921,
22.9266719372443));
#16384=CARTESIAN_POINT('Ctrl Pts',(-0.0802684116077697,1.99322666607084,
22.9279326279261));
#16385=CARTESIAN_POINT('Ctrl Pts',(-0.104487052154384,1.99201799135356,
22.9295078450429));
#16386=CARTESIAN_POINT('Ctrl Pts',(-0.109545358246763,1.99174622826215,
22.9298358853588));
#16387=CARTESIAN_POINT('Ctrl Pts',(-0.117615683156636,1.99128180377935,
22.9303576702476));
#16388=CARTESIAN_POINT('Ctrl Pts',(-0.120628352459527,1.99110157246374,
22.9305520998308));
#16389=CARTESIAN_POINT('Ctrl Pts',(-0.126346212928537,1.99074647944261,
22.9309204286286));
#16390=CARTESIAN_POINT('Ctrl Pts',(-0.129051423148523,1.99057294294943,
22.9310943970733));
#16391=CARTESIAN_POINT('Ctrl Pts',(-0.135253185204583,1.99016241047088,
22.9314925620557));
#16392=CARTESIAN_POINT('Ctrl Pts',(-0.138749468457328,1.98992171444525,
22.9317165487041));
#16393=CARTESIAN_POINT('Ctrl Pts',(-0.149801137813084,1.98913161119218,
22.9324230942243));
#16394=CARTESIAN_POINT('Ctrl Pts',(-0.15735415065229,1.98854837085257,22.9329037924214));
#16395=CARTESIAN_POINT('Ctrl Pts',(-0.28648262272367,1.97783679620507,22.9410875448193));
#16396=CARTESIAN_POINT('Ctrl Pts',(-0.406901180141803,1.95661746999596,
22.9482056002925));
#16397=CARTESIAN_POINT('Ctrl Pts',(-0.621530690257861,1.89810757757316,
22.9611217636335));
#16398=CARTESIAN_POINT('Ctrl Pts',(-0.716285028780494,1.86441609797625,
22.9669126470896));
#16399=CARTESIAN_POINT('Ctrl Pts',(-0.854614684721749,1.80312235940427,
22.9759071334529));
#16400=CARTESIAN_POINT('Ctrl Pts',(-0.900325374427479,1.78073864722669,
22.9789727220304));
#16401=CARTESIAN_POINT('Ctrl Pts',(-0.97194032319833,1.74220738601696,22.9839648429509));
#16402=CARTESIAN_POINT('Ctrl Pts',(-0.998417588995791,1.7271701505935,22.9858536225567));
#16403=CARTESIAN_POINT('Ctrl Pts',(-1.03199352782441,1.70707129254735,22.9883094515749));
#16404=CARTESIAN_POINT('Ctrl Pts',(-1.03941844569094,1.70256052174982,22.9888564171801));
#16405=CARTESIAN_POINT('Ctrl Pts',(-1.0513520291994,1.69520349792219,22.9897419240131));
#16406=CARTESIAN_POINT('Ctrl Pts',(-1.05587921942695,1.69238738524937,22.9900793555606));
#16407=CARTESIAN_POINT('Ctrl Pts',(-1.06449755453409,1.68697835768705,22.9907246157254));
#16408=CARTESIAN_POINT('Ctrl Pts',(-1.06859065758722,1.68438862165204,22.9910323250967));
#16409=CARTESIAN_POINT('Ctrl Pts',(-1.07793219279699,1.6784304104782,22.99173750054));
#16410=CARTESIAN_POINT('Ctrl Pts',(-1.08317432106507,1.67505219136933,22.9921353272643));
#16411=CARTESIAN_POINT('Ctrl Pts',(-1.09926195288677,1.66457763535729,22.993362788102));
#16412=CARTESIAN_POINT('Ctrl Pts',(-1.11005403220569,1.65740024665056,22.9941954496608));
#16413=CARTESIAN_POINT('Ctrl Pts',(-1.21483124195331,1.58623462481342,23.0023717791739));
#16414=CARTESIAN_POINT('Ctrl Pts',(-1.30323624114396,1.51443798564161,23.0100203358722));
#16415=CARTESIAN_POINT('Ctrl Pts',(-1.50116996399817,1.32346489153158,23.0289967490486));
#16416=CARTESIAN_POINT('Ctrl Pts',(-1.60327700833823,1.19773717721527,23.0404789963379));
#16417=CARTESIAN_POINT('Ctrl Pts',(-1.70234724473211,1.04002864368377,23.05291554291));
#16418=CARTESIAN_POINT('Ctrl Pts',(-1.71517869549642,1.01872857297808,23.0545566636392));
#16419=CARTESIAN_POINT('Ctrl Pts',(-1.73036589387726,0.992417171983663,
23.056532158617));
#16420=CARTESIAN_POINT('Ctrl Pts',(-1.73310276251856,0.987629883228585,
23.0568895340401));
#16421=CARTESIAN_POINT('Ctrl Pts',(-1.7373558430498,0.980118337971587,23.0574469854864));
#16422=CARTESIAN_POINT('Ctrl Pts',(-1.73888555378862,0.977401817555047,
23.0576479149568));
#16423=CARTESIAN_POINT('Ctrl Pts',(-1.7417248953565,0.972331838970681,23.0580216553195));
#16424=CARTESIAN_POINT('Ctrl Pts',(-1.74303611474329,0.969979339477833,
23.0581945655442));
#16425=CARTESIAN_POINT('Ctrl Pts',(-1.7459928653227,0.96464918521885,23.0585851951958));
#16426=CARTESIAN_POINT('Ctrl Pts',(-1.74763554162708,0.961669979963943,
23.0588027304219));
#16427=CARTESIAN_POINT('Ctrl Pts',(-1.75246197112126,0.95286341941922,23.0594434493249));
#16428=CARTESIAN_POINT('Ctrl Pts',(-1.755624296569,0.947024280885827,23.0598652876223));
#16429=CARTESIAN_POINT('Ctrl Pts',(-1.77737433577252,0.906380114963131,
23.0627816430493));
#16430=CARTESIAN_POINT('Ctrl Pts',(-1.79495642220029,0.8710432771751,23.0652162207104));
#16431=CARTESIAN_POINT('Ctrl Pts',(-1.8399621045117,0.773430284616103,23.0717332378804));
#16432=CARTESIAN_POINT('Ctrl Pts',(-1.86526779382775,0.710234016399131,
23.0757294286686));
#16433=CARTESIAN_POINT('Ctrl Pts',(-1.91109823134709,0.576311706650971,
23.083974474948));
#16434=CARTESIAN_POINT('Ctrl Pts',(-1.9310371488245,0.505496973663527,23.0882121008464));
#16435=CARTESIAN_POINT('Ctrl Pts',(-1.97224762056614,0.320508096779724,
23.0992750624989));
#16436=CARTESIAN_POINT('Ctrl Pts',(-1.98754377539282,0.205304950558999,
23.1061703190404));
#16437=CARTESIAN_POINT('Ctrl Pts',(-1.9933461117447,0.0760207468025642,
23.1142438290231));
#16438=CARTESIAN_POINT('Ctrl Pts',(-1.99381268178783,0.0626007273850999,
23.1150856383549));
#16439=CARTESIAN_POINT('Ctrl Pts',(-1.99429969261233,0.0428523872649563,
23.1163303205717));
#16440=CARTESIAN_POINT('Ctrl Pts',(-1.99442557610496,0.0365268521593845,
23.1167298923532));
#16441=CARTESIAN_POINT('Ctrl Pts',(-1.99459487876957,0.025345795898488,
23.1174377951233));
#16442=CARTESIAN_POINT('Ctrl Pts',(-1.9946506658732,0.0204904912615598,
23.1177457363784));
#16443=CARTESIAN_POINT('Ctrl Pts',(-1.99473016566779,0.0103480754011308,
23.1183901519715));
#16444=CARTESIAN_POINT('Ctrl Pts',(-1.99475058642723,0.00506098315732062,
23.1187267270038));
#16445=CARTESIAN_POINT('Ctrl Pts',(-1.99474902517757,-0.0087138660979068,
23.1196053566625));
#16446=CARTESIAN_POINT('Ctrl Pts',(-1.9946938891948,-0.0172014425346067,
23.1201484450481));
#16447=CARTESIAN_POINT('Ctrl Pts',(-1.99421732812472,-0.0542043318696857,
23.1225237571064));
#16448=CARTESIAN_POINT('Ctrl Pts',(-1.99323860203648,-0.0827078989382515,
23.1243733150328));
#16449=CARTESIAN_POINT('Ctrl Pts',(-1.98905590780223,-0.157635912292106,
23.1292903308347));
#16450=CARTESIAN_POINT('Ctrl Pts',(-1.98483814030236,-0.203983992940521,
23.1323879126468));
#16451=CARTESIAN_POINT('Ctrl Pts',(-1.95455248711019,-0.443592193144321,
23.1486909148887));
#16452=CARTESIAN_POINT('Ctrl Pts',(-1.90187522353625,-0.632379154602995,
23.1626549211699));
#16453=CARTESIAN_POINT('Ctrl Pts',(-1.80804089939705,-0.843392388790838,
23.1782463106551));
#16454=CARTESIAN_POINT('Ctrl Pts',(-1.79253034456599,-0.875875549766268,
23.1806414509516));
#16455=CARTESIAN_POINT('Ctrl Pts',(-1.77346524620833,-0.913172124085858,
23.1833709687034));
#16456=CARTESIAN_POINT('Ctrl Pts',(-1.77075903035547,-0.918408823045166,
23.1837537300751));
#16457=CARTESIAN_POINT('Ctrl Pts',(-1.76639735237753,-0.926757995672966,
23.1843631245572));
#16458=CARTESIAN_POINT('Ctrl Pts',(-1.76475680942004,-0.929878160354736,
23.1845906671854));
#16459=CARTESIAN_POINT('Ctrl Pts',(-1.76183874938753,-0.935392509872981,
23.1849924437385));
#16460=CARTESIAN_POINT('Ctrl Pts',(-1.76056460846337,-0.937788454904466,
23.1851668895022));
#16461=CARTESIAN_POINT('Ctrl Pts',(-1.75786827307977,-0.942833887326651,
23.1855339738396));
#16462=CARTESIAN_POINT('Ctrl Pts',(-1.75644497947497,-0.945482754450112,
23.1857265406866));
#16463=CARTESIAN_POINT('Ctrl Pts',(-1.75263144473794,-0.952541727892574,
23.1862393298405));
#16464=CARTESIAN_POINT('Ctrl Pts',(-1.75023052963959,-0.956946089857879,
23.1865588787993));
#16465=CARTESIAN_POINT('Ctrl Pts',(-1.73882750533259,-0.977677906821048,
23.1880613664042));
#16466=CARTESIAN_POINT('Ctrl Pts',(-1.72961302219979,-0.993888342299916,
23.1892312934512));
#16467=CARTESIAN_POINT('Ctrl Pts',(-1.63309970154953,-1.15826934146475,
23.2010695161742));
#16468=CARTESIAN_POINT('Ctrl Pts',(-1.52720194505438,-1.29471050508555,
23.2107312579881));
#16469=CARTESIAN_POINT('Ctrl Pts',(-1.32679705967998,-1.49358808513795,
23.2272465626159));
#16470=CARTESIAN_POINT('Ctrl Pts',(-1.24219966557471,-1.56465031829176,
23.2338246066446));
#16471=CARTESIAN_POINT('Ctrl Pts',(-1.14162357909098,-1.63581481464676,
23.2415152945552));
#16472=CARTESIAN_POINT('Ctrl Pts',(-1.13100420169006,-1.64317497163366,
23.2423256127113));
#16473=CARTESIAN_POINT('Ctrl Pts',(-1.11516086298745,-1.65392944428732,
23.2435323777622));
#16474=CARTESIAN_POINT('Ctrl Pts',(-1.10999115150386,-1.65740339060022,
23.243925808805));
#16475=CARTESIAN_POINT('Ctrl Pts',(-1.10077329374681,-1.66353514211645,
23.2446267567087));
#16476=CARTESIAN_POINT('Ctrl Pts',(-1.09673156150811,-1.66620253708753,
23.2449339099134));
#16477=CARTESIAN_POINT('Ctrl Pts',(-1.08821621177744,-1.67177794836034,
23.2455806604972));
#16478=CARTESIAN_POINT('Ctrl Pts',(-1.08374056529833,-1.67468278142873,
23.2459203736799));
#16479=CARTESIAN_POINT('Ctrl Pts',(-1.07193161152075,-1.68227999406973,
23.2468161655731));
#16480=CARTESIAN_POINT('Ctrl Pts',(-1.06457920834362,-1.68694234145723,
23.2473733540514));
#16481=CARTESIAN_POINT('Ctrl Pts',(-1.03122238256557,-1.70778984284034,
23.2498990087871));
#16482=CARTESIAN_POINT('Ctrl Pts',(-1.00487897809935,-1.7234221234075,23.251887635923));
#16483=CARTESIAN_POINT('Ctrl Pts',(-0.933475600799488,-1.76359942893007,
23.257265357599));
#16484=CARTESIAN_POINT('Ctrl Pts',(-0.887813513219818,-1.78702155907183,
23.2606920268837));
#16485=CARTESIAN_POINT('Ctrl Pts',(-0.74989968001803,-1.85117264763509,
23.2710012891206));
#16486=CARTESIAN_POINT('Ctrl Pts',(-0.655412613570665,-1.88669570874792,
23.2780208097599));
#16487=CARTESIAN_POINT('Ctrl Pts',(-0.476956152970249,-1.93875815817386,
23.2909906949848));
#16488=CARTESIAN_POINT('Ctrl Pts',(-0.393810231563768,-1.95734149815231,
23.2969216868984));
#16489=CARTESIAN_POINT('Ctrl Pts',(-0.272841538709948,-1.97635502766549,
23.3051984700274));
#16490=CARTESIAN_POINT('Ctrl Pts',(-0.23579768814716,-1.9811162493413,23.3076857610451));
#16491=CARTESIAN_POINT('Ctrl Pts',(-0.192708361052063,-1.98542856268389,
23.3105080609151));
#16492=CARTESIAN_POINT('Ctrl Pts',(-0.186774775760275,-1.98599553757468,
23.3108951482672));
#16493=CARTESIAN_POINT('Ctrl Pts',(-0.177308789349377,-1.98685724672708,
23.3115101031235));
#16494=CARTESIAN_POINT('Ctrl Pts',(-0.173778047380773,-1.98716917155475,
23.311738906018));
#16495=CARTESIAN_POINT('Ctrl Pts',(-0.167539926545156,-1.98770352783902,
23.3121421252462));
#16496=CARTESIAN_POINT('Ctrl Pts',(-0.164832902839687,-1.98792984183838,
23.3123167585887));
#16497=CARTESIAN_POINT('Ctrl Pts',(-0.159138252878659,-1.98839421675648,
23.3126833982275));
#16498=CARTESIAN_POINT('Ctrl Pts',(-0.156150557010321,-1.98863107402954,
23.3128753360066));
#16499=CARTESIAN_POINT('Ctrl Pts',(-0.148205419613642,-1.98924292951431,
23.3133846650563));
#16500=CARTESIAN_POINT('Ctrl Pts',(-0.143247050664874,-1.98960613257581,
23.3137013988908));
#16501=CARTESIAN_POINT('Ctrl Pts',(-0.120158958304453,-1.99121058944073,
23.3151712093473));
#16502=CARTESIAN_POINT('Ctrl Pts',(-0.102013460011142,-1.9922226525018,
23.3163119516667));
#16503=CARTESIAN_POINT('Ctrl Pts',(0.0721482535332635,-1.99955059285529,
23.3271443796006));
#16504=CARTESIAN_POINT('Ctrl Pts',(0.228407247983973,-1.98777586765281,
23.3359982637772));
#16505=CARTESIAN_POINT('Ctrl Pts',(0.505905225920262,-1.93367475198033,
23.3524575742911));
#16506=CARTESIAN_POINT('Ctrl Pts',(0.627495153678901,-1.89770416836332,
23.3599421174552));
#16507=CARTESIAN_POINT('Ctrl Pts',(0.756922254093729,-1.84560710890173,
23.3686500867499));
#16508=CARTESIAN_POINT('Ctrl Pts',(0.768945875507025,-1.84063008965246,
23.3694661371741));
#16509=CARTESIAN_POINT('Ctrl Pts',(0.786667708233827,-1.83309042301939,
23.3706798129451));
#16510=CARTESIAN_POINT('Ctrl Pts',(0.792404126349157,-1.83061800527753,
23.3710743714424));
#16511=CARTESIAN_POINT('Ctrl Pts',(0.802568961300915,-1.82618019315275,
23.3717765897554));
#16512=CARTESIAN_POINT('Ctrl Pts',(0.80700202865933,-1.82422552349433,23.3720838811373));
#16513=CARTESIAN_POINT('Ctrl Pts',(0.816293693860386,-1.82008805784805,
23.3727301711858));
#16514=CARTESIAN_POINT('Ctrl Pts',(0.821150751457561,-1.81790191578938,
23.3730692827983));
#16515=CARTESIAN_POINT('Ctrl Pts',(0.833885484590942,-1.81210861439441,
23.3739617862645));
#16516=CARTESIAN_POINT('Ctrl Pts',(0.84174844855115,-1.8084695676751,23.3745162731614));
#16517=CARTESIAN_POINT('Ctrl Pts',(0.8769238999694,-1.79191096902896,23.3770123905391));
#16518=CARTESIAN_POINT('Ctrl Pts',(0.903963212586597,-1.77842368151106,
23.3789736084757));
#16519=CARTESIAN_POINT('Ctrl Pts',(0.975216696786217,-1.74083740676136,
23.3842594739241));
#16520=CARTESIAN_POINT('Ctrl Pts',(1.01883999213167,-1.71567095796115,23.3876201356824));
#16521=CARTESIAN_POINT('Ctrl Pts',(1.14616281086576,-1.63564866321966,23.397804624408));
#16522=CARTESIAN_POINT('Ctrl Pts',(1.22673212697761,-1.57612204790798,23.4047656862329));
#16523=CARTESIAN_POINT('Ctrl Pts',(1.39582846739347,-1.43034182055913,23.4203430100627));
#16524=CARTESIAN_POINT('Ctrl Pts',(1.48152101030504,-1.34138651921141,23.428939245322));
#16525=CARTESIAN_POINT('Ctrl Pts',(1.56317762342597,-1.23917729437307,23.4374802745958));
#16526=CARTESIAN_POINT('Ctrl Pts',(1.56786016952027,-1.23324739713201,23.4379713729433));
#16527=CARTESIAN_POINT('Ctrl Pts',(1.57466290298419,-1.22453115928623,23.4386865991766));
#16528=CARTESIAN_POINT('Ctrl Pts',(1.57680955813855,-1.22176570418388,23.43891255525));
#16529=CARTESIAN_POINT('Ctrl Pts',(1.58060518530478,-1.21684927422991,23.4393125243509));
#16530=CARTESIAN_POINT('Ctrl Pts',(1.58225706528265,-1.21470057533529,23.4394867427081));
#16531=CARTESIAN_POINT('Ctrl Pts',(1.58574039398235,-1.21015043947522,23.4398544279491));
#16532=CARTESIAN_POINT('Ctrl Pts',(1.58757076486305,-1.20774821470317,23.4400478189554));
#16533=CARTESIAN_POINT('Ctrl Pts',(1.59246206786622,-1.20129841286687,23.4405651429938));
#16534=CARTESIAN_POINT('Ctrl Pts',(1.59551304754545,-1.19724326301008,23.4408883815903));
#16535=CARTESIAN_POINT('Ctrl Pts',(1.61008246577444,-1.17772400221129,23.4424348631599));
#16536=CARTESIAN_POINT('Ctrl Pts',(1.62139222879797,-1.16210441840951,23.4436441520524));
#16537=CARTESIAN_POINT('Ctrl Pts',(1.65234309306941,-1.11802739496867,23.4469861887131));
#16538=CARTESIAN_POINT('Ctrl Pts',(1.6714742034511,-1.08921863447767,23.4490903080501));
#16539=CARTESIAN_POINT('Ctrl Pts',(1.73855742906047,-0.982267292718258,
23.4566699342053));
#16540=CARTESIAN_POINT('Ctrl Pts',(1.78185919567237,-0.901338475025759,
23.4619702574825));
#16541=CARTESIAN_POINT('Ctrl Pts',(1.88329833705338,-0.675632609041538,
23.4763218962617));
#16542=CARTESIAN_POINT('Ctrl Pts',(1.9302826131601,-0.526585044463319,23.4853972505017));
#16543=CARTESIAN_POINT('Ctrl Pts',(1.96180649197478,-0.361249142563708,
23.4959077948642));
#16544=CARTESIAN_POINT('Ctrl Pts',(1.96404452639658,-0.348876398957765,
23.4966965630493));
#16545=CARTESIAN_POINT('Ctrl Pts',(1.96720450914525,-0.330411755365373,
23.4978773128872));
#16546=CARTESIAN_POINT('Ctrl Pts',(1.96821547587624,-0.324335240180608,
23.4982664667296));
#16547=CARTESIAN_POINT('Ctrl Pts',(1.9699695713428,-0.313481772045245,23.4989626242555));
#16548=CARTESIAN_POINT('Ctrl Pts',(1.97072351440209,-0.308706596187221,
23.4992692823731));
#16549=CARTESIAN_POINT('Ctrl Pts',(1.97227870373655,-0.298618726618705,
23.4999179216718));
#16550=CARTESIAN_POINT('Ctrl Pts',(1.97307585794811,-0.293305449916991,
23.5002600298725));
#16551=CARTESIAN_POINT('Ctrl Pts',(1.97513249206851,-0.279209461670281,
23.5011689128497));
#16552=CARTESIAN_POINT('Ctrl Pts',(1.97635484519537,-0.270421534579042,
23.5017368567759));
#16553=CARTESIAN_POINT('Ctrl Pts',(1.9817603742648,-0.229563441443843,23.5043837528508));
#16554=CARTESIAN_POINT('Ctrl Pts',(1.98522162512093,-0.197404279792403,
23.5064853128086));
#16555=CARTESIAN_POINT('Ctrl Pts',(1.99248029282498,-0.110046304635909,
23.5122471284698));
#16556=CARTESIAN_POINT('Ctrl Pts',(1.99476539572911,-0.0547538784678133,
23.515951896427));
#16557=CARTESIAN_POINT('Ctrl Pts',(1.99472083995126,0.10451325394847,23.526781267626));
#16558=CARTESIAN_POINT('Ctrl Pts',(1.9865654187481,0.208299913540758,23.5340406579857));
#16559=CARTESIAN_POINT('Ctrl Pts',(1.95915198494756,0.381997034783298,23.5463031836596));
#16560=CARTESIAN_POINT('Ctrl Pts',(1.94410889756941,0.452371616561821,23.5513002630426));
#16561=CARTESIAN_POINT('Ctrl Pts',(1.92459300799034,0.52438207763953,23.5563582050747));
#16562=CARTESIAN_POINT('Ctrl Pts',(1.92388355714886,0.526979001876972,23.5565405317299));
#16563=CARTESIAN_POINT('Ctrl Pts',(1.91293780788876,0.566728884556873,23.5593300370431));
#16564=CARTESIAN_POINT('Ctrl Pts',(1.90163135373923,0.603582109440011,23.5618992216618));
#16565=CARTESIAN_POINT('Ctrl Pts',(1.88714598905568,0.646336688542688,23.5648416176739));
#16566=CARTESIAN_POINT('Ctrl Pts',(1.88499768322268,0.652575540593402,23.5652700112501));
#16567=CARTESIAN_POINT('Ctrl Pts',(1.88169783714548,0.662006287213307,23.5659159868007));
#16568=CARTESIAN_POINT('Ctrl Pts',(1.88056907120851,0.665206015803639,23.5661348795406));
#16569=CARTESIAN_POINT('Ctrl Pts',(1.8785299182394,0.670939757755498,23.5665266041083));
#16570=CARTESIAN_POINT('Ctrl Pts',(1.87762256378575,0.673474810599133,23.566699613101));
#16571=CARTESIAN_POINT('Ctrl Pts',(1.87565131502325,0.678947322787018,23.5670726941056));
#16572=CARTESIAN_POINT('Ctrl Pts',(1.87458565584975,0.681884111765686,23.5672726588038));
#16573=CARTESIAN_POINT('Ctrl Pts',(1.87160975254923,0.690025531034069,23.5678263509243));
#16574=CARTESIAN_POINT('Ctrl Pts',(1.86968468490016,0.695224769503947,23.5681792049505));
#16575=CARTESIAN_POINT('Ctrl Pts',(1.8588546071197,0.724104388849254,23.5701353838328));
#16576=CARTESIAN_POINT('Ctrl Pts',(1.84952091343033,0.747623001823085,23.5717142674897));
#16577=CARTESIAN_POINT('Ctrl Pts',(1.77672407169122,0.921338327501038,23.5833155069715));
#16578=CARTESIAN_POINT('Ctrl Pts',(1.69549862677927,1.06344329104048,23.5925040380343));
#16579=CARTESIAN_POINT('Ctrl Pts',(1.53109117556448,1.28344508501932,23.6085625433659));
#16580=CARTESIAN_POINT('Ctrl Pts',(1.4569463657648,1.36703089007972,23.6152105917116));
#16581=CARTESIAN_POINT('Ctrl Pts',(1.36684771682189,1.45290131481923,23.6229796625555));
#16582=CARTESIAN_POINT('Ctrl Pts',(1.35739682748506,1.46173484317861,23.6237909587903));
#16583=CARTESIAN_POINT('Ctrl Pts',(1.34326708730211,1.47468638280055,23.6249989032714));
#16584=CARTESIAN_POINT('Ctrl Pts',(1.33865365091826,1.47887551771544,23.6253925269934));
#16585=CARTESIAN_POINT('Ctrl Pts',(1.33042007070808,1.48628175407773,23.6260936917885));
#16586=CARTESIAN_POINT('Ctrl Pts',(1.32680768147181,1.48950743293105,23.6264008683893));
#16587=CARTESIAN_POINT('Ctrl Pts',(1.31919197301362,1.49625818407874,23.6270475392056));
#16588=CARTESIAN_POINT('Ctrl Pts',(1.31518619492876,1.49978041287506,23.6273871487336));
#16589=CARTESIAN_POINT('Ctrl Pts',(1.30461071510917,1.50900434553152,23.6282823740344));
#16590=CARTESIAN_POINT('Ctrl Pts',(1.29801781657593,1.5146791662547,23.6288390970325));
#16591=CARTESIAN_POINT('Ctrl Pts',(1.26852141581792,1.539734112662,23.6313239912969));
#16592=CARTESIAN_POINT('Ctrl Pts',(1.24522053660386,1.55863830704041,23.6332714379365));
#16593=CARTESIAN_POINT('Ctrl Pts',(1.18191530166107,1.60767261629807,23.6385249713219));
#16594=CARTESIAN_POINT('Ctrl Pts',(1.14118987123898,1.63683230458749,23.6418667609568));
#16595=CARTESIAN_POINT('Ctrl Pts',(0.940859549598415,1.7691576096526,23.6581228254526));
#16596=CARTESIAN_POINT('Ctrl Pts',(0.768181820920613,1.85068050346722,23.6717211793796));
#16597=CARTESIAN_POINT('Ctrl Pts',(0.552643863484696,1.91699617388569,23.6869401403451));
#16598=CARTESIAN_POINT('Ctrl Pts',(0.518414199006579,1.92653488787829,23.6893038023525));
#16599=CARTESIAN_POINT('Ctrl Pts',(0.478249402392898,1.93657934166554,23.6920015694262));
#16600=CARTESIAN_POINT('Ctrl Pts',(0.472546934248044,1.93797869814918,23.6923828249911));
#16601=CARTESIAN_POINT('Ctrl Pts',(0.463417611951749,1.94017629571473,23.692990282724));
#16602=CARTESIAN_POINT('Ctrl Pts',(0.45999473453063,1.9409906713302,23.6932173854796));
#16603=CARTESIAN_POINT('Ctrl Pts',(0.453929010551228,1.94241689000338,23.6936186599172));
#16604=CARTESIAN_POINT('Ctrl Pts',(0.451287051159835,1.94303240297234,23.6937930416336));
#16605=CARTESIAN_POINT('Ctrl Pts',(0.445710364076144,1.94431964897152,23.6941602878834));
#16606=CARTESIAN_POINT('Ctrl Pts',(0.442775376528311,1.94499012651898,23.6943530795521));
#16607=CARTESIAN_POINT('Ctrl Pts',(0.435029191163544,1.94674124639669,23.6948606453425));
#16608=CARTESIAN_POINT('Ctrl Pts',(0.430215446881831,1.9478107064346,23.6951747824341));
#16609=CARTESIAN_POINT('Ctrl Pts',(0.408050723907701,1.95264882282056,23.6966155324378));
#16610=CARTESIAN_POINT('Ctrl Pts',(0.390653213139125,1.95620370573333,23.6977304015264));
#16611=CARTESIAN_POINT('Ctrl Pts',(0.204940835335811,1.99157434516518,23.7094837883902));
#16612=CARTESIAN_POINT('Ctrl Pts',(0.0332189798035813,2.00182024001185,
23.7191134295983));
#16613=CARTESIAN_POINT('Ctrl Pts',(-0.249371251815618,1.98226314295159,
23.735673871603));
#16614=CARTESIAN_POINT('Ctrl Pts',(-0.360157589699307,1.96515504596192,
23.7423425028749));
#16615=CARTESIAN_POINT('Ctrl Pts',(-0.481494251299651,1.9358094723581,23.7501346318597));
#16616=CARTESIAN_POINT('Ctrl Pts',(-0.494042288972022,1.93264513851989,
23.7509462056751));
#16617=CARTESIAN_POINT('Ctrl Pts',(-0.512586591501544,1.92777628177231,
23.7521544848603));
#16618=CARTESIAN_POINT('Ctrl Pts',(-0.518607257418771,1.92616534011788,
23.7525481632421));
#16619=CARTESIAN_POINT('Ctrl Pts',(-0.529292821961587,1.92325248647641,
23.7532493895822));
#16620=CARTESIAN_POINT('Ctrl Pts',(-0.533960735595123,1.92196174527034,
23.7535565728365));
#16621=CARTESIAN_POINT('Ctrl Pts',(-0.543759390674064,1.91921383261398,
23.7542032211045));
#16622=CARTESIAN_POINT('Ctrl Pts',(-0.548889073906283,1.91775305862833,
23.7545428012916));
#16623=CARTESIAN_POINT('Ctrl Pts',(-0.562367470627117,1.91385632305801,
23.7554378662082));
#16624=CARTESIAN_POINT('Ctrl Pts',(-0.570706147551424,1.91138632581234,
23.7559944574439));
#16625=CARTESIAN_POINT('Ctrl Pts',(-0.604992364418687,1.90098605029883,
23.7582949190547));
#16626=CARTESIAN_POINT('Ctrl Pts',(-0.630791909139028,1.89258161542398,
23.7600542336474));
#16627=CARTESIAN_POINT('Ctrl Pts',(-0.698689076826157,1.8689209807639,23.7647621105274));
#16628=CARTESIAN_POINT('Ctrl Pts',(-0.740456204801879,1.85276986005703,
23.7677390252861));
#16629=CARTESIAN_POINT('Ctrl Pts',(-0.909454284734698,1.78079188784509,
23.7801191361801));
#16630=CARTESIAN_POINT('Ctrl Pts',(-1.03121915171044,1.71315659905379,23.789871457052));
#16631=CARTESIAN_POINT('Ctrl Pts',(-1.22072439977651,1.58032328031969,23.8059602169694));
#16632=CARTESIAN_POINT('Ctrl Pts',(-1.29271876487694,1.52199618006782,23.8123206104895));
#16633=CARTESIAN_POINT('Ctrl Pts',(-1.36615420523471,1.45351709097308,23.8188795583615));
#16634=CARTESIAN_POINT('Ctrl Pts',(-1.3718666376865,1.44812678298547,23.8193902384723));
#16635=CARTESIAN_POINT('Ctrl Pts',(-1.38011944227563,1.4402466928626,23.820128510716));
#16636=CARTESIAN_POINT('Ctrl Pts',(-1.38268513775431,1.43778371863211,23.820358099703));
#16637=CARTESIAN_POINT('Ctrl Pts',(-1.38720015276246,1.43342620580564,23.8207622217604));
#16638=CARTESIAN_POINT('Ctrl Pts',(-1.38915220347169,1.43153452884168,23.8209369750641));
#16639=CARTESIAN_POINT('Ctrl Pts',(-1.39324406521857,1.42755297040368,23.8213033512786));
#16640=CARTESIAN_POINT('Ctrl Pts',(-1.39538303964321,1.42546226942006,23.8214949076363));
#16641=CARTESIAN_POINT('Ctrl Pts',(-1.39973270937868,1.42119159301034,23.8218845401698));
#16642=CARTESIAN_POINT('Ctrl Pts',(-1.40194303478421,1.41901125058355,23.8220825868988));
#16643=CARTESIAN_POINT('Ctrl Pts',(-1.41135220183156,1.40968627479287,23.8229259225855));
#16644=CARTESIAN_POINT('Ctrl Pts',(-1.41850175010443,1.40249179187023,23.8235674014619));
#16645=CARTESIAN_POINT('Ctrl Pts',(-1.47692329544274,1.34279929116321,23.8288179677158));
#16646=CARTESIAN_POINT('Ctrl Pts',(-1.5253237470081,1.28755676184601,23.8332251170261));
#16647=CARTESIAN_POINT('Ctrl Pts',(-1.60653713303421,1.18383649492422,23.8409893840692));
#16648=CARTESIAN_POINT('Ctrl Pts',(-1.6404691108211,1.13635025668703,23.8443725172661));
#16649=CARTESIAN_POINT('Ctrl Pts',(-1.75326816242585,0.962887809147457,
23.8563728741762));
#16650=CARTESIAN_POINT('Ctrl Pts',(-1.82008480420641,0.82969052032929,23.864993293892));
#16651=CARTESIAN_POINT('Ctrl Pts',(-1.87616565224984,0.677652026728188,
23.8750178796965));
#16652=CARTESIAN_POINT('Ctrl Pts',(-1.88070891294721,0.664938940771866,
23.8758570534069));
#16653=CARTESIAN_POINT('Ctrl Pts',(-1.88906313910096,0.640791131455061,
23.8774533668785));
#16654=CARTESIAN_POINT('Ctrl Pts',(-1.89290020856103,0.629366036516225,
23.8782096185501));
#16655=CARTESIAN_POINT('Ctrl Pts',(-1.89853473711962,0.612071145671082,
23.8793561668438));
#16656=CARTESIAN_POINT('Ctrl Pts',(-1.90040906792504,0.606226532405844,
23.8797439313981));
#16657=CARTESIAN_POINT('Ctrl Pts',(-1.90371064622489,0.595765628862508,
23.8804385434803));
#16658=CARTESIAN_POINT('Ctrl Pts',(-1.90514815752673,0.591152608285838,
23.8807450513088));
#16659=CARTESIAN_POINT('Ctrl Pts',(-1.90815241219042,0.581387080402761,
23.8813943551046));
#16660=CARTESIAN_POINT('Ctrl Pts',(-1.90971507567197,0.576233367847167,
23.8817372818706));
#16661=CARTESIAN_POINT('Ctrl Pts',(-1.91381323816139,0.5625177217628,23.8826506400654));
#16662=CARTESIAN_POINT('Ctrl Pts',(-1.91631212581144,0.553945060475702,
23.8832222612265));
#16663=CARTESIAN_POINT('Ctrl Pts',(-1.92164618138673,0.535177986340756,
23.8844753789138));
#16664=CARTESIAN_POINT('Ctrl Pts',(-1.92445794802636,0.524977259124959,
23.885157618341));
#16665=CARTESIAN_POINT('Ctrl Pts',(-1.93258636608511,0.49454530847942,23.8871964645244));
#16666=CARTESIAN_POINT('Ctrl Pts',(-1.93766594980546,0.474252819067026,
23.8885606169804));
#16667=CARTESIAN_POINT('Ctrl Pts',(-1.97733335685798,0.30449394592668,23.9000136371151));
#16668=CARTESIAN_POINT('Ctrl Pts',(-1.9948831837466,0.151605765928437,23.9106520774232));
#16669=CARTESIAN_POINT('Ctrl Pts',(-1.99474923905662,-0.00174234986216392,
23.9213503181716));
#16670=CARTESIAN_POINT('',(-1.99474926718243,0.0010867435194402,25.5194715405958));
#16671=CARTESIAN_POINT('Ctrl Pts',(-1.99474923809175,-0.00174345415664474,
23.921350395212));
#16672=CARTESIAN_POINT('Ctrl Pts',(-1.99465279067116,-0.112092451863815,
23.9290488277685));
#16673=CARTESIAN_POINT('Ctrl Pts',(-1.98539976672746,-0.222258981767481,
23.9367300039541));
#16674=CARTESIAN_POINT('Ctrl Pts',(-1.9655027770055,-0.340465031149384,
23.9446282277757));
#16675=CARTESIAN_POINT('Ctrl Pts',(-1.96386091420468,-0.349811265962468,
23.9452502755261));
#16676=CARTESIAN_POINT('Ctrl Pts',(-1.96129918682364,-0.363806979434425,
23.9461777490928));
#16677=CARTESIAN_POINT('Ctrl Pts',(-1.96042937329275,-0.368465319865975,
23.94648577956));
#16678=CARTESIAN_POINT('Ctrl Pts',(-1.95895292373932,-0.376219291464799,
23.9469973399604));
#16679=CARTESIAN_POINT('Ctrl Pts',(-1.95835553605177,-0.379316632175001,
23.9472013731833));
#16680=CARTESIAN_POINT('Ctrl Pts',(-1.95717076530788,-0.385382033945181,
23.9476002971232));
#16681=CARTESIAN_POINT('Ctrl Pts',(-1.95658397186845,-0.388350200194083,
23.9477952203578));
#16682=CARTESIAN_POINT('Ctrl Pts',(-1.95545899848093,-0.393973357184122,
23.9481639272714));
#16683=CARTESIAN_POINT('Ctrl Pts',(-1.95492217013066,-0.396628553850687,
23.9483377825302));
#16684=CARTESIAN_POINT('Ctrl Pts',(-1.95368117794911,-0.402702872206078,
23.9487349645909));
#16685=CARTESIAN_POINT('Ctrl Pts',(-1.95297344754239,-0.406121240522431,
23.9489580850993));
#16686=CARTESIAN_POINT('Ctrl Pts',(-1.95107046975322,-0.415192690172853,
23.9495491769418));
#16687=CARTESIAN_POINT('Ctrl Pts',(-1.94985961674241,-0.420842517918806,
23.9499162733754));
#16688=CARTESIAN_POINT('Ctrl Pts',(-1.94142015396722,-0.459402516522879,
23.9524150602883));
#16689=CARTESIAN_POINT('Ctrl Pts',(-1.93338273436137,-0.492132517417653,
23.954502973977));
#16690=CARTESIAN_POINT('Ctrl Pts',(-1.90440374169407,-0.598434083893761,
23.9612223348132));
#16691=CARTESIAN_POINT('Ctrl Pts',(-1.88005922411456,-0.671011385436395,
23.9657133471563));
#16692=CARTESIAN_POINT('Ctrl Pts',(-1.83716998721847,-0.778035824832143,
23.9724255051228));
#16693=CARTESIAN_POINT('Ctrl Pts',(-1.8216874782631,-0.813626497658147,
23.9746729601069));
#16694=CARTESIAN_POINT('Ctrl Pts',(-1.79086914167354,-0.879173470817844,
23.9788748868046));
#16695=CARTESIAN_POINT('Ctrl Pts',(-1.77579462330578,-0.909236868255141,
23.9808277094315));
#16696=CARTESIAN_POINT('Ctrl Pts',(-1.71652760379852,-1.02033233302828,
23.9881802475092));
#16697=CARTESIAN_POINT('Ctrl Pts',(-1.66749369487277,-1.09863874415188,
23.9936466243389));
#16698=CARTESIAN_POINT('Ctrl Pts',(-1.5952864039728,-1.19792255513778,24.001181778613));
#16699=CARTESIAN_POINT('Ctrl Pts',(-1.57679117181271,-1.22216471970837,
24.0030729722191));
#16700=CARTESIAN_POINT('Ctrl Pts',(-1.55227739557933,-1.25281250263351,
24.0055356771755));
#16701=CARTESIAN_POINT('Ctrl Pts',(-1.54676148439092,-1.25961628524112,
24.0060870758325));
#16702=CARTESIAN_POINT('Ctrl Pts',(-1.5378061436593,-1.27051502241697,24.0069780273091));
#16703=CARTESIAN_POINT('Ctrl Pts',(-1.53439470184874,-1.27463291017202,
24.0073164452571));
#16704=CARTESIAN_POINT('Ctrl Pts',(-1.52786418681096,-1.28245156367787,
24.0079624455536));
#16705=CARTESIAN_POINT('Ctrl Pts',(-1.5247481174861,-1.28615479786205,24.0082699038189));
#16706=CARTESIAN_POINT('Ctrl Pts',(-1.51760552899487,-1.29458083506208,
24.0089728930618));
#16707=CARTESIAN_POINT('Ctrl Pts',(-1.51357039935403,-1.29929624216576,
24.0093687767347));
#16708=CARTESIAN_POINT('Ctrl Pts',(-1.50114117973247,-1.31368441565182,
24.0105844077761));
#16709=CARTESIAN_POINT('Ctrl Pts',(-1.49267601609012,-1.32329508564254,
24.0114070985766));
#16710=CARTESIAN_POINT('Ctrl Pts',(-1.38615133566813,-1.44191193243975,
24.0216969295528));
#16711=CARTESIAN_POINT('Ctrl Pts',(-1.27647576917412,-1.53984363938957,
24.0316879210935));
#16712=CARTESIAN_POINT('Ctrl Pts',(-1.0702558457911,-1.68669602331309,24.0493104153485));
#16713=CARTESIAN_POINT('Ctrl Pts',(-0.978603550161111,-1.74147288182424,
24.0568001916866));
#16714=CARTESIAN_POINT('Ctrl Pts',(-0.855730961011988,-1.80213140402328,
24.0661142930362));
#16715=CARTESIAN_POINT('Ctrl Pts',(-0.828145634363181,-1.8149733047239,
24.0681603329142));
#16716=CARTESIAN_POINT('Ctrl Pts',(-0.784218998465963,-1.83421247526352,
24.0713365951796));
#16717=CARTESIAN_POINT('Ctrl Pts',(-0.768069486342853,-1.84103344833148,
24.0724872693959));
#16718=CARTESIAN_POINT('Ctrl Pts',(-0.747291076407721,-1.84948848021564,
24.0739441232411));
#16719=CARTESIAN_POINT('Ctrl Pts',(-0.742743809329414,-1.8513193204498,
24.0742615129731));
#16720=CARTESIAN_POINT('Ctrl Pts',(-0.735399127518461,-1.85424505102597,
24.0747717891419));
#16721=CARTESIAN_POINT('Ctrl Pts',(-0.732605943601032,-1.85535040294364,
24.0749652969065));
#16722=CARTESIAN_POINT('Ctrl Pts',(-0.727283928081611,-1.8574426018349,
24.0753329370241));
#16723=CARTESIAN_POINT('Ctrl Pts',(-0.724755610275348,-1.85843058428661,
24.0755071341862));
#16724=CARTESIAN_POINT('Ctrl Pts',(-0.718933757633465,-1.86069188286548,
24.0759072128252));
#16725=CARTESIAN_POINT('Ctrl Pts',(-0.715638855198403,-1.86196161620634,
24.0761328774428));
#16726=CARTESIAN_POINT('Ctrl Pts',(-0.706815859720396,-1.86533479211552,
24.0767351648404));
#16727=CARTESIAN_POINT('Ctrl Pts',(-0.701281701269774,-1.86742242778882,
24.0771108591689));
#16728=CARTESIAN_POINT('Ctrl Pts',(-0.66162711299586,-1.8821800789354,24.0797885291145));
#16729=CARTESIAN_POINT('Ctrl Pts',(-0.627172277782475,-1.89393970981801,
24.0820393367));
#16730=CARTESIAN_POINT('Ctrl Pts',(-0.551681195802812,-1.91741882002782,
24.0868472279642));
#16731=CARTESIAN_POINT('Ctrl Pts',(-0.510551773686136,-1.92877794768979,
24.0893892755834));
#16732=CARTESIAN_POINT('Ctrl Pts',(-0.323099646129521,-1.97413126349641,
24.100755001292));
#16733=CARTESIAN_POINT('Ctrl Pts',(-0.173591687040931,-1.99285105981596,
24.1092601102918));
#16734=CARTESIAN_POINT('Ctrl Pts',(0.0240842515977598,-1.99516971525552,
24.1210459103544));
#16735=CARTESIAN_POINT('Ctrl Pts',(0.0715662878921597,-1.99403109702275,
24.1239139078616));
#16736=CARTESIAN_POINT('Ctrl Pts',(0.147359413969956,-1.98950299507709,
24.128580815825));
#16737=CARTESIAN_POINT('Ctrl Pts',(0.175718014996744,-1.98719903766466,
24.1303468470648));
#16738=CARTESIAN_POINT('Ctrl Pts',(0.212757002036039,-1.98339083978368,
24.1326832479322));
#16739=CARTESIAN_POINT('Ctrl Pts',(0.221491287196444,-1.9824344556556,24.1332363726432));
#16740=CARTESIAN_POINT('Ctrl Pts',(0.235536690430103,-1.9808025371232,24.1341294442246));
#16741=CARTESIAN_POINT('Ctrl Pts',(0.240851971477427,-1.9801632636064,24.1344682463535));
#16742=CARTESIAN_POINT('Ctrl Pts',(0.250966031543559,-1.97890551165015,
24.1351145394054));
#16743=CARTESIAN_POINT('Ctrl Pts',(0.255765266877857,-1.97829095448804,
24.1354219043741));
#16744=CARTESIAN_POINT('Ctrl Pts',(0.26670389895806,-1.97684975863752,24.1361240639416));
#16745=CARTESIAN_POINT('Ctrl Pts',(0.272841752749752,-1.97601197224867,
24.1365192082104));
#16746=CARTESIAN_POINT('Ctrl Pts',(0.288768295710323,-1.97376245909409,
24.1375475675274));
#16747=CARTESIAN_POINT('Ctrl Pts',(0.298550471832266,-1.97230651356485,
24.1381821751678));
#16748=CARTESIAN_POINT('Ctrl Pts',(0.360902967211727,-1.96255168495387,
24.1422466868669));
#16749=CARTESIAN_POINT('Ctrl Pts',(0.41312975383929,-1.95222513536441,24.1457404505359));
#16750=CARTESIAN_POINT('Ctrl Pts',(0.493921979091102,-1.93286333653532,
24.1512909246542));
#16751=CARTESIAN_POINT('Ctrl Pts',(0.522805370618792,-1.92525167296347,
24.1533047261749));
#16752=CARTESIAN_POINT('Ctrl Pts',(0.700896802238948,-1.87401602107133,
24.1659001550139));
#16753=CARTESIAN_POINT('Ctrl Pts',(0.844732785471984,-1.8137285152229,24.1769147240754));
#16754=CARTESIAN_POINT('Ctrl Pts',(1.01717125465571,-1.71645026982445,24.1905156988104));
#16755=CARTESIAN_POINT('Ctrl Pts',(1.05356330410089,-1.69435644420534,24.193406871667));
#16756=CARTESIAN_POINT('Ctrl Pts',(1.10785586492808,-1.65896884516567,24.1977225723866));
#16757=CARTESIAN_POINT('Ctrl Pts',(1.12628537179292,-1.64651256017508,24.199187926505));
#16758=CARTESIAN_POINT('Ctrl Pts',(1.14884918654194,-1.63070575536196,24.2009787457159));
#16759=CARTESIAN_POINT('Ctrl Pts',(1.15318266446678,-1.6276441435174,24.201322528226));
#16760=CARTESIAN_POINT('Ctrl Pts',(1.1600250501193,-1.62276893866617,24.2018650386116));
#16761=CARTESIAN_POINT('Ctrl Pts',(1.16254200175584,-1.62096676081837,24.2020645330235));
#16762=CARTESIAN_POINT('Ctrl Pts',(1.16724314087684,-1.61758408776861,24.202437006543));
#16763=CARTESIAN_POINT('Ctrl Pts',(1.16942829507573,-1.61600504136666,24.202610078474));
#16764=CARTESIAN_POINT('Ctrl Pts',(1.17438936357263,-1.61240471845241,24.2030028866066));
#16765=CARTESIAN_POINT('Ctrl Pts',(1.17716325780369,-1.6103807060039,24.2032224300741));
#16766=CARTESIAN_POINT('Ctrl Pts',(1.18540549262256,-1.604333963078,24.2038745545989));
#16767=CARTESIAN_POINT('Ctrl Pts',(1.19085860858676,-1.60029041882337,24.2043057178331));
#16768=CARTESIAN_POINT('Ctrl Pts',(1.23057322461868,-1.57052618273185,24.2074446060734));
#16769=CARTESIAN_POINT('Ctrl Pts',(1.26402178832222,-1.54373330140024,24.2100815212263));
#16770=CARTESIAN_POINT('Ctrl Pts',(1.31132018422234,-1.50327740400627,24.2138430072335));
#16771=CARTESIAN_POINT('Ctrl Pts',(1.32587203846001,-1.49045863996984,24.2150049986557));
#16772=CARTESIAN_POINT('Ctrl Pts',(1.4197816107232,-1.40526952655246,24.2225525144359));
#16773=CARTESIAN_POINT('Ctrl Pts',(1.49337437433657,-1.32679978512355,24.2287070769935));
#16774=CARTESIAN_POINT('Ctrl Pts',(1.63924810156653,-1.14365761095221,24.2423338040877));
#16775=CARTESIAN_POINT('Ctrl Pts',(1.70856460972787,-1.03724984490412,24.2498235495663));
#16776=CARTESIAN_POINT('Ctrl Pts',(1.77368214543783,-0.912834937453798,
24.2585810730765));
#16777=CARTESIAN_POINT('Ctrl Pts',(1.77992145239572,-0.900608452332835,
24.2594413874956));
#16778=CARTESIAN_POINT('Ctrl Pts',(1.78887675680459,-0.882603116836053,
24.260708296405));
#16779=CARTESIAN_POINT('Ctrl Pts',(1.79169207574805,-0.876873888907671,
24.2611114163569));
#16780=CARTESIAN_POINT('Ctrl Pts',(1.79660387799518,-0.866755861908511,
24.2618233746603));
#16781=CARTESIAN_POINT('Ctrl Pts',(1.79871191132452,-0.862372702462842,
24.2621318081385));
#16782=CARTESIAN_POINT('Ctrl Pts',(1.80279016010193,-0.853812934315414,
24.2627341815745));
#16783=CARTESIAN_POINT('Ctrl Pts',(1.80476194522063,-0.849637104096287,
24.2630280646748));
#16784=CARTESIAN_POINT('Ctrl Pts',(1.81001545410144,-0.838410461586305,
24.263818236068));
#16785=CARTESIAN_POINT('Ctrl Pts',(1.81327044726143,-0.831347297122637,
24.2643154432615));
#16786=CARTESIAN_POINT('Ctrl Pts',(1.825031216009,-0.805429371343678,24.2661403235196));
#16787=CARTESIAN_POINT('Ctrl Pts',(1.83328464078335,-0.786462194827535,
24.267476597395));
#16788=CARTESIAN_POINT('Ctrl Pts',(1.90551667062883,-0.613147517489005,
24.2796984130807));
#16789=CARTESIAN_POINT('Ctrl Pts',(1.95014818225195,-0.451489706270898,
24.2912644850565));
#16790=CARTESIAN_POINT('Ctrl Pts',(1.98391298754606,-0.218595361575162,
24.3076817646254));
#16791=CARTESIAN_POINT('Ctrl Pts',(1.99023569928573,-0.150523786525468,
24.3124396476893));
#16792=CARTESIAN_POINT('Ctrl Pts',(1.99447905525916,-0.0477118212640706,
24.319462270324));
#16793=CARTESIAN_POINT('Ctrl Pts',(1.99500651553182,-0.0131309361932714,
24.3217962472275));
#16794=CARTESIAN_POINT('Ctrl Pts',(1.99442734688521,0.040730414786778,24.3253710777205));
#16795=CARTESIAN_POINT('Ctrl Pts',(1.99394040476064,0.0600094924994351,
24.3266385612098));
#16796=CARTESIAN_POINT('Ctrl Pts',(1.99297224901735,0.084350043741496,24.3282210238128));
#16797=CARTESIAN_POINT('Ctrl Pts',(1.99275120751043,0.0894200289155129,
24.3285496652554));
#16798=CARTESIAN_POINT('Ctrl Pts',(1.99236775925638,0.0975058729650793,
24.3290721821101));
#16799=CARTESIAN_POINT('Ctrl Pts',(1.99221784929738,0.100522259355966,24.3292667458315));
#16800=CARTESIAN_POINT('Ctrl Pts',(1.99192040963798,0.106244951995511,24.3296351767487));
#16801=CARTESIAN_POINT('Ctrl Pts',(1.9917742166748,0.108951264478881,24.3298091138144));
#16802=CARTESIAN_POINT('Ctrl Pts',(1.99142654850298,0.115152593399556,24.3302070089047));
#16803=CARTESIAN_POINT('Ctrl Pts',(1.99122138840926,0.118647379439393,24.3304307580262));
#16804=CARTESIAN_POINT('Ctrl Pts',(1.99054439881678,0.129682854629902,24.3311358046469));
#16805=CARTESIAN_POINT('Ctrl Pts',(1.99003892020851,0.137221524846043,24.331615252671));
#16806=CARTESIAN_POINT('Ctrl Pts',(1.98052531225459,0.267973035464976,24.3398956453475));
#16807=CARTESIAN_POINT('Ctrl Pts',(1.96013097686202,0.390111179758361,24.347096542537));
#16808=CARTESIAN_POINT('Ctrl Pts',(1.90303792717769,0.606180446493574,24.360069550165));
#16809=CARTESIAN_POINT('Ctrl Pts',(1.87029669565566,0.700711897142247,24.3658330992057));
#16810=CARTESIAN_POINT('Ctrl Pts',(1.80056189805657,0.861816562679126,24.376274683477));
#16811=CARTESIAN_POINT('Ctrl Pts',(1.76658773575693,0.929471168230145,24.3808661325634));
#16812=CARTESIAN_POINT('Ctrl Pts',(1.72321374659392,1.00483328680699,24.3863041298895));
#16813=CARTESIAN_POINT('Ctrl Pts',(1.71748724564385,1.01459011593004,24.3870145854276));
#16814=CARTESIAN_POINT('Ctrl Pts',(1.70864694147781,1.02936292832067,24.3881003338285));
#16815=CARTESIAN_POINT('Ctrl Pts',(1.70559328749342,1.03441478395331,24.3884734335319));
#16816=CARTESIAN_POINT('Ctrl Pts',(1.7002510890917,1.04316475666656,24.3891228329462));
#16817=CARTESIAN_POINT('Ctrl Pts',(1.69797277958277,1.04686910108838,24.3893987555987));
#16818=CARTESIAN_POINT('Ctrl Pts',(1.69320296228229,1.05456789930382,24.3899743035228));
#16819=CARTESIAN_POINT('Ctrl Pts',(1.69070939342061,1.05856103843683,24.3902740036549));
#16820=CARTESIAN_POINT('Ctrl Pts',(1.68381607659257,1.06951333341939,24.3910992895908));
#16821=CARTESIAN_POINT('Ctrl Pts',(1.67938738019203,1.07645407428068,24.3916259462001));
#16822=CARTESIAN_POINT('Ctrl Pts',(1.66381088131199,1.10053577774974,24.393466153971));
#16823=CARTESIAN_POINT('Ctrl Pts',(1.65244290318465,1.11753212339374,24.3947879021905));
#16824=CARTESIAN_POINT('Ctrl Pts',(1.553307943506,1.26092895789727,24.4061409948184));
#16825=CARTESIAN_POINT('Ctrl Pts',(1.45146380432375,1.37693216016352,24.4167397099128));
#16826=CARTESIAN_POINT('Ctrl Pts',(1.24286395492987,1.56541568042858,24.4363525405638));
#16827=CARTESIAN_POINT('Ctrl Pts',(1.14043242965982,1.64154139354727,24.4452620599943));
#16828=CARTESIAN_POINT('Ctrl Pts',(1.02307466799342,1.71243719233642,24.4542467322188));
#16829=CARTESIAN_POINT('Ctrl Pts',(1.01467939891546,1.71742500296605,24.4548830692597));
#16830=CARTESIAN_POINT('Ctrl Pts',(1.00285613105903,1.72433250019094,24.4557699538541));
#16831=CARTESIAN_POINT('Ctrl Pts',(0.999458745204333,1.72630391533398,24.4560237311901));
#16832=CARTESIAN_POINT('Ctrl Pts',(0.993654395430378,1.72964915095251,24.4564554579586));
#16833=CARTESIAN_POINT('Ctrl Pts',(0.991250361729803,1.731028007763,24.4566337318285));
#16834=CARTESIAN_POINT('Ctrl Pts',(0.986644425630587,1.73365704537647,24.4569742512903));
#16835=CARTESIAN_POINT('Ctrl Pts',(0.984443014531997,1.73490804509254,24.4571365510909));
#16836=CARTESIAN_POINT('Ctrl Pts',(0.979224826230272,1.73786026398153,24.4575202097655));
#16837=CARTESIAN_POINT('Ctrl Pts',(0.976205976155617,1.73955783174615,24.4577413337628));
#16838=CARTESIAN_POINT('Ctrl Pts',(0.967182128225263,1.74460125745333,24.4583998774732));
#16839=CARTESIAN_POINT('Ctrl Pts',(0.961164163686093,1.74792398873556,24.4588358510935));
#16840=CARTESIAN_POINT('Ctrl Pts',(0.850580883783602,1.80823712305644,24.4667907576366));
#16841=CARTESIAN_POINT('Ctrl Pts',(0.741118302338165,1.85579153776437,24.4737522235301));
#16842=CARTESIAN_POINT('Ctrl Pts',(0.531813067990394,1.92522292595316,24.4865610883943));
#16843=CARTESIAN_POINT('Ctrl Pts',(0.433282923212879,1.9497623728666,24.4924027281299));
#16844=CARTESIAN_POINT('Ctrl Pts',(0.28194835801721,1.97541069586179,24.5015184778251));
#16845=CARTESIAN_POINT('Ctrl Pts',(0.230259840528209,1.98210041858869,24.5046548890355));
#16846=CARTESIAN_POINT('Ctrl Pts',(0.147520336951575,1.98952878325001,24.5097521605438));
#16847=CARTESIAN_POINT('Ctrl Pts',(0.116610259064667,1.99157950179583,24.5116731847748));
#16848=CARTESIAN_POINT('Ctrl Pts',(0.0769338970957597,1.99328501037302,
24.5141652903314));
#16849=CARTESIAN_POINT('Ctrl Pts',(0.0681993019638421,1.99360297160564,
24.5147155398574));
#16850=CARTESIAN_POINT('Ctrl Pts',(0.0541220424738574,1.99402279784403,
24.5156050799119));
#16851=CARTESIAN_POINT('Ctrl Pts',(0.0487804996123187,1.99416061934702,
24.5159432421207));
#16852=CARTESIAN_POINT('Ctrl Pts',(0.038598871393781,1.9943823913274,24.516589048915));
#16853=CARTESIAN_POINT('Ctrl Pts',(0.0337589009995935,1.99447018820393,
24.5168965706667));
#16854=CARTESIAN_POINT('Ctrl Pts',(0.0227053724201449,1.99463045250019,
24.5176001188872));
#16855=CARTESIAN_POINT('Ctrl Pts',(0.0164917229766111,1.99469150437021,
24.5179965000875));
#16856=CARTESIAN_POINT('Ctrl Pts',(-0.00256827801079911,1.99478971230896,
24.519215154022));
#16857=CARTESIAN_POINT('Ctrl Pts',(-0.0154145857663771,1.99473180405164,
24.5200403915418));
#16858=CARTESIAN_POINT('Ctrl Pts',(-0.172184840180993,1.99251065078239,
24.5301601197068));
#16859=CARTESIAN_POINT('Ctrl Pts',(-0.315436724216096,1.9749000268383,24.5399580096762));
#16860=CARTESIAN_POINT('Ctrl Pts',(-0.552149893694806,1.91937728125612,
24.5568744293126));
#16861=CARTESIAN_POINT('Ctrl Pts',(-0.646955330323089,1.88953126734442,
24.5638452416923));
#16862=CARTESIAN_POINT('Ctrl Pts',(-0.773692497982777,1.83897003895562,
24.5731792577456));
#16863=CARTESIAN_POINT('Ctrl Pts',(-0.807848050673968,1.82422388238281,
24.5756952989373));
#16864=CARTESIAN_POINT('Ctrl Pts',(-0.859979598503877,1.79996522289418,
24.5795158526611));
#16865=CARTESIAN_POINT('Ctrl Pts',(-0.878254925247854,1.79111922520407,
24.5808513263986));
#16866=CARTESIAN_POINT('Ctrl Pts',(-0.901006199927359,1.77967470578203,
24.5825060938361));
#16867=CARTESIAN_POINT('Ctrl Pts',(-0.90561056873868,1.77733613307732,24.5828405780685));
#16868=CARTESIAN_POINT('Ctrl Pts',(-0.912910953474712,1.77359251104837,
24.5833702075762));
#16869=CARTESIAN_POINT('Ctrl Pts',(-0.915612888767559,1.77219915428476,
24.5835660735578));
#16870=CARTESIAN_POINT('Ctrl Pts',(-0.920713568435187,1.76955401390615,
24.583935519528));
#16871=CARTESIAN_POINT('Ctrl Pts',(-0.923112921844298,1.76830354205627,
24.58410917555));
#16872=CARTESIAN_POINT('Ctrl Pts',(-0.928579767823083,1.76544022489674,
24.5845045565699));
#16873=CARTESIAN_POINT('Ctrl Pts',(-0.931645601753395,1.76382426734391,
24.5847260818944));
#16874=CARTESIAN_POINT('Ctrl Pts',(-0.939736413563216,1.75953273459614,
24.5853101883261));
#16875=CARTESIAN_POINT('Ctrl Pts',(-0.944754220846486,1.75684360008956,
24.5856719271693));
#16876=CARTESIAN_POINT('Ctrl Pts',(-0.977996552490043,1.73884481977141,
24.5880654306901));
#16877=CARTESIAN_POINT('Ctrl Pts',(-1.00586130043403,1.72287605264944,24.5900574896322));
#16878=CARTESIAN_POINT('Ctrl Pts',(-1.0423339995788,1.70078752285367,24.5926622664386));
#16879=CARTESIAN_POINT('Ctrl Pts',(-1.05129465642398,1.69526337715488,24.593301990847));
#16880=CARTESIAN_POINT('Ctrl Pts',(-1.21488619405234,1.5926150738254,24.6049850767716));
#16881=CARTESIAN_POINT('Ctrl Pts',(-1.35551269500975,1.47477784745069,24.6151685484025));
#16882=CARTESIAN_POINT('Ctrl Pts',(-1.51202133911129,1.30206118178868,24.6290295725916));
#16883=CARTESIAN_POINT('Ctrl Pts',(-1.54445941879055,1.26341456983849,24.6320695834745));
#16884=CARTESIAN_POINT('Ctrl Pts',(-1.59395474535689,1.1996879522464,24.6370236714478));
#16885=CARTESIAN_POINT('Ctrl Pts',(-1.6119662035686,1.17537556457359,24.6389007328936));
#16886=CARTESIAN_POINT('Ctrl Pts',(-1.63441740665788,1.14358316017397,24.6413433685512));
#16887=CARTESIAN_POINT('Ctrl Pts',(-1.63937145886673,1.13646993776835,24.6418891272794));
#16888=CARTESIAN_POINT('Ctrl Pts',(-1.64729497814889,1.12493341924129,24.6427731519681));
#16889=CARTESIAN_POINT('Ctrl Pts',(-1.65029340039267,1.1205300685312,24.6431103150676));
#16890=CARTESIAN_POINT('Ctrl Pts',(-1.6559848401882,1.11209947501826,24.6437553767652));
#16891=CARTESIAN_POINT('Ctrl Pts',(-1.65868089947099,1.10807432346332,24.6440631574425));
#16892=CARTESIAN_POINT('Ctrl Pts',(-1.66481855852499,1.09883835337637,24.6447689422366));
#16893=CARTESIAN_POINT('Ctrl Pts',(-1.66825039208598,1.09362113526534,24.6451673092199));
#16894=CARTESIAN_POINT('Ctrl Pts',(-1.67875280985181,1.07749044666894,24.6463980708924));
#16895=CARTESIAN_POINT('Ctrl Pts',(-1.68574110689991,1.06652405806988,24.6472335166841));
#16896=CARTESIAN_POINT('Ctrl Pts',(-1.75653363288302,0.952998665625529,
24.6558704774647));
#16897=CARTESIAN_POINT('Ctrl Pts',(-1.81099275340321,0.844933407534047,
24.6640182995758));
#16898=CARTESIAN_POINT('Ctrl Pts',(-1.89669653932677,0.627892676070149,
24.6801576601004));
#16899=CARTESIAN_POINT('Ctrl Pts',(-1.92910970265941,0.519848325567508,
24.6880896858351));
#16900=CARTESIAN_POINT('Ctrl Pts',(-1.96124544112281,0.366700833071344,
24.6988497710607));
#16901=CARTESIAN_POINT('Ctrl Pts',(-1.96883819819459,0.323465416687952,
24.7018336885393));
#16902=CARTESIAN_POINT('Ctrl Pts',(-1.97819467383585,0.25747168457394,24.7062746383364));
#16903=CARTESIAN_POINT('Ctrl Pts',(-1.98100445365406,0.234877203149722,
24.7077750160446));
#16904=CARTESIAN_POINT('Ctrl Pts',(-1.98399751677331,0.206906196102912,
24.7096036396167));
#16905=CARTESIAN_POINT('Ctrl Pts',(-1.98454659819748,0.201571629320054,
24.709951100188));
#16906=CARTESIAN_POINT('Ctrl Pts',(-1.98537756954806,0.193165681766397,
24.7104965111316));
#16907=CARTESIAN_POINT('Ctrl Pts',(-1.98567385577742,0.190095799732308,
24.7106952563148));
#16908=CARTESIAN_POINT('Ctrl Pts',(-1.98621595263948,0.184339440572999,
24.7110670830157));
#16909=CARTESIAN_POINT('Ctrl Pts',(-1.9864634306143,0.18165318278547,24.7112402539311));
#16910=CARTESIAN_POINT('Ctrl Pts',(-1.98701509888672,0.175529114314983,
24.7116342663681));
#16911=CARTESIAN_POINT('Ctrl Pts',(-1.98731581663326,0.172091018284429,
24.7118549104847));
#16912=CARTESIAN_POINT('Ctrl Pts',(-1.98820843694681,0.161571264060495,
24.7125283718489));
#16913=CARTESIAN_POINT('Ctrl Pts',(-1.98877142928303,0.154487112236704,
24.7129795942538));
#16914=CARTESIAN_POINT('Ctrl Pts',(-1.99290202203708,0.0987410107736622,
24.7165133331227));
#16915=CARTESIAN_POINT('Ctrl Pts',(-1.99472128911868,0.0499613971369182,
24.7195037966203));
#16916=CARTESIAN_POINT('Ctrl Pts',(-1.99480080932865,-0.0868098885426201,
24.7277257662376));
#16917=CARTESIAN_POINT('Ctrl Pts',(-1.98903262344727,-0.174692803194069,
24.7328230142401));
#16918=CARTESIAN_POINT('Ctrl Pts',(-1.95803198486501,-0.408752169165059,
24.74651622615));
#16919=CARTESIAN_POINT('Ctrl Pts',(-1.92229262429381,-0.552948044952065,
24.7551123909539));
#16920=CARTESIAN_POINT('Ctrl Pts',(-1.86641816742885,-0.704045295008075,
24.7650778956838));
#16921=CARTESIAN_POINT('Ctrl Pts',(-1.86179041892914,-0.71619339342671,
24.7658857943512));
#16922=CARTESIAN_POINT('Ctrl Pts',(-1.85247219293728,-0.739953483439173,
24.767479631554));
#16923=CARTESIAN_POINT('Ctrl Pts',(-1.84779044288463,-0.751568261066158,
24.7682652530824));
#16924=CARTESIAN_POINT('Ctrl Pts',(-1.84064690531058,-0.76882010561023,
24.7694421996398));
#16925=CARTESIAN_POINT('Ctrl Pts',(-1.83826784203443,-0.774491268114423,
24.7698307238299));
#16926=CARTESIAN_POINT('Ctrl Pts',(-1.8339723382099,-0.784599506098843,
24.770526180263));
#16927=CARTESIAN_POINT('Ctrl Pts',(-1.83206591720916,-0.789040807953773,
24.7708327695994));
#16928=CARTESIAN_POINT('Ctrl Pts',(-1.82800393169236,-0.798409742002944,
24.771481706832));
#16929=CARTESIAN_POINT('Ctrl Pts',(-1.8258445440323,-0.803335664900426,
24.7718241834518));
#16930=CARTESIAN_POINT('Ctrl Pts',(-1.82005982986606,-0.816387748305625,
24.7727350805117));
#16931=CARTESIAN_POINT('Ctrl Pts',(-1.81640003862968,-0.824498414361877,
24.7733046793466));
#16932=CARTESIAN_POINT('Ctrl Pts',(-1.79907367186601,-0.862221042952241,
24.7759707674385));
#16933=CARTESIAN_POINT('Ctrl Pts',(-1.78473713218674,-0.891518010709639,
24.7780902656372));
#16934=CARTESIAN_POINT('Ctrl Pts',(-1.74386291663732,-0.97010430071404,
24.7839139396217));
#16935=CARTESIAN_POINT('Ctrl Pts',(-1.71596003467865,-1.01864636614899,
24.7876638079324));
#16936=CARTESIAN_POINT('Ctrl Pts',(-1.63023492685055,-1.15424147042592,
24.7985770710958));
#16937=CARTESIAN_POINT('Ctrl Pts',(-1.56756881966963,-1.23800810630327,
24.8058748004737));
#16938=CARTESIAN_POINT('Ctrl Pts',(-1.44754524723948,-1.37463955385313,
24.8185549930584));
#16939=CARTESIAN_POINT('Ctrl Pts',(-1.39310497077041,-1.42978368481388,
24.823930585147));
#16940=CARTESIAN_POINT('Ctrl Pts',(-1.30989680635394,-1.50479061653673,
24.831484744924));
#16941=CARTESIAN_POINT('Ctrl Pts',(-1.28359995612032,-1.5272838483881,24.8337851872403));
#16942=CARTESIAN_POINT('Ctrl Pts',(-1.25220610460746,-1.55275283303931,
24.8364190931154));
#16943=CARTESIAN_POINT('Ctrl Pts',(-1.24766668556361,-1.55640268976449,
24.8367972744302));
#16944=CARTESIAN_POINT('Ctrl Pts',(-1.24037045001631,-1.56221669154071,
24.8374007760712));
#16945=CARTESIAN_POINT('Ctrl Pts',(-1.23762384665511,-1.56439351163755,
24.837626978875));
#16946=CARTESIAN_POINT('Ctrl Pts',(-1.23274260626034,-1.56824123702767,
24.8380272283957));
#16947=CARTESIAN_POINT('Ctrl Pts',(-1.23061028531054,-1.56991504128184,
24.8382014814548));
#16948=CARTESIAN_POINT('Ctrl Pts',(-1.2260967647778,-1.57344316522101,24.8385690701382));
#16949=CARTESIAN_POINT('Ctrl Pts',(-1.22371477355211,-1.57529642419013,
24.838762330539));
#16950=CARTESIAN_POINT('Ctrl Pts',(-1.21732365050612,-1.58024566137745,
24.8392789357539));
#16951=CARTESIAN_POINT('Ctrl Pts',(-1.21330688337693,-1.58333181250433,
24.8396015894927));
#16952=CARTESIAN_POINT('Ctrl Pts',(-1.1940248446609,-1.59803006813968,24.8411410069655));
#16953=CARTESIAN_POINT('Ctrl Pts',(-1.17860374706491,-1.60943738668073,
24.8423439703263));
#16954=CARTESIAN_POINT('Ctrl Pts',(-1.13514035863695,-1.64062838231273,
24.8456640249635));
#16955=CARTESIAN_POINT('Ctrl Pts',(-1.10674751427758,-1.65991425981153,
24.8477529422688));
#16956=CARTESIAN_POINT('Ctrl Pts',(-1.00136579363134,-1.72758808519944,
24.85527428219));
#16957=CARTESIAN_POINT('Ctrl Pts',(-0.921587320028886,-1.77143250008126,
24.8605335887246));
#16958=CARTESIAN_POINT('Ctrl Pts',(-0.696700288990083,-1.87570529516955,
24.8749099665122));
#16959=CARTESIAN_POINT('Ctrl Pts',(-0.547038822559078,-1.92468201091436,
24.8840483904333));
#16960=CARTESIAN_POINT('Ctrl Pts',(-0.38089898564765,-1.9580860104944,24.8946311564645));
#16961=CARTESIAN_POINT('Ctrl Pts',(-0.368580340605556,-1.9604421396274,
24.8954179634974));
#16962=CARTESIAN_POINT('Ctrl Pts',(-0.35018566129031,-1.9637809027981,24.8965963430807));
#16963=CARTESIAN_POINT('Ctrl Pts',(-0.344125808957736,-1.96485186662963,
24.8969851046454));
#16964=CARTESIAN_POINT('Ctrl Pts',(-0.333297445260089,-1.96671394448956,
24.897680825257));
#16965=CARTESIAN_POINT('Ctrl Pts',(-0.328530810786781,-1.96751580226344,
24.8979874403947));
#16966=CARTESIAN_POINT('Ctrl Pts',(-0.318456321448877,-1.96917293261258,
24.8986362646849));
#16967=CARTESIAN_POINT('Ctrl Pts',(-0.313147837028925,-1.97002408575012,
24.898978601917));
#16968=CARTESIAN_POINT('Ctrl Pts',(-0.299054022946336,-1.97222545842726,
24.8998887369477));
#16969=CARTESIAN_POINT('Ctrl Pts',(-0.290263076973265,-1.97353842359669,
24.90045770964));
#16970=CARTESIAN_POINT('Ctrl Pts',(-0.249278590371073,-1.97937987150333,
24.9031165190084));
#16971=CARTESIAN_POINT('Ctrl Pts',(-0.216987773772212,-1.98317941448709,
24.9052292120486));
#16972=CARTESIAN_POINT('Ctrl Pts',(-0.129135933739827,-1.99134541417093,
24.9110293912699));
#16973=CARTESIAN_POINT('Ctrl Pts',(-0.073464799946427,-1.99417517199349,
24.914762119613));
#16974=CARTESIAN_POINT('Ctrl Pts',(0.086511349446103,-1.99559893616663,
24.9256435069905));
#16975=CARTESIAN_POINT('Ctrl Pts',(0.190680115523286,-1.98835037163982,
24.932926675516));
#16976=CARTESIAN_POINT('Ctrl Pts',(0.369272373697638,-1.96175649805191,
24.9455168792244));
#16977=CARTESIAN_POINT('Ctrl Pts',(0.44404751974304,-1.94619475763947,24.9508169181002));
#16978=CARTESIAN_POINT('Ctrl Pts',(0.55263844868642,-1.91700895452849,24.9584093896121));
#16979=CARTESIAN_POINT('Ctrl Pts',(0.587267110705992,-1.90668569281275,
24.960813952761));
#16980=CARTESIAN_POINT('Ctrl Pts',(0.627206283165518,-1.89358777632888,
24.9635529691945));
#16981=CARTESIAN_POINT('Ctrl Pts',(0.632805678472392,-1.89172391318637,
24.963936178456));
#16982=CARTESIAN_POINT('Ctrl Pts',(0.641738426139534,-1.88870638151676,
24.9645461488819));
#16983=CARTESIAN_POINT('Ctrl Pts',(0.645077079576406,-1.88756869147619,
24.9647738222278));
#16984=CARTESIAN_POINT('Ctrl Pts',(0.650979276237851,-1.88553995179913,
24.9651757481395));
#16985=CARTESIAN_POINT('Ctrl Pts',(0.653544038195908,-1.88465251927691,
24.9653502130806));
#16986=CARTESIAN_POINT('Ctrl Pts',(0.658945727421706,-1.88277112963622,
24.9657172499799));
#16987=CARTESIAN_POINT('Ctrl Pts',(0.661782214298192,-1.88177599607677,
24.9659097505482));
#16988=CARTESIAN_POINT('Ctrl Pts',(0.669341590003951,-1.87910471055398,
24.9664221751043));
#16989=CARTESIAN_POINT('Ctrl Pts',(0.67406046870462,-1.87741715214741,24.9667414274281));
#16990=CARTESIAN_POINT('Ctrl Pts',(0.69625759808999,-1.86938456844525,24.9682404361089));
#16991=CARTESIAN_POINT('Ctrl Pts',(0.713653637166449,-1.86281288756075,
24.9694072538952));
#16992=CARTESIAN_POINT('Ctrl Pts',(0.890985755314345,-1.79297341069414,
24.9812443533709));
#16993=CARTESIAN_POINT('Ctrl Pts',(1.04221640274193,-1.70950660411171,24.9909072358625));
#16994=CARTESIAN_POINT('Ctrl Pts',(1.26981173988946,-1.54233023613869,25.0074257501017));
#16995=CARTESIAN_POINT('Ctrl Pts',(1.35316004384931,-1.46974729997954,25.014005993112));
#16996=CARTESIAN_POINT('Ctrl Pts',(1.43908206178811,-1.38138963969378,25.0216991421134));
#16997=CARTESIAN_POINT('Ctrl Pts',(1.44799969571827,-1.37203913424563,25.0225094916385));
#16998=CARTESIAN_POINT('Ctrl Pts',(1.46108043357888,-1.35805387406573,25.0237162945179));
#16999=CARTESIAN_POINT('Ctrl Pts',(1.46531380302344,-1.35348506289926,25.0241097317422));
#17000=CARTESIAN_POINT('Ctrl Pts',(1.47280035437641,-1.34532900420376,25.0248106866029));
#17001=CARTESIAN_POINT('Ctrl Pts',(1.47606201653617,-1.34174958023644,25.0251178405568));
#17002=CARTESIAN_POINT('Ctrl Pts',(1.48288995625797,-1.33420141256047,25.0257645885746));
#17003=CARTESIAN_POINT('Ctrl Pts',(1.48645340394456,-1.33023017130069,25.0261042984264));
#17004=CARTESIAN_POINT('Ctrl Pts',(1.4957890802489,-1.31974178595706,25.0270000721123));
#17005=CARTESIAN_POINT('Ctrl Pts',(1.50153460164272,-1.31320112331544,25.0275572456325));
#17006=CARTESIAN_POINT('Ctrl Pts',(1.52729902619214,-1.28348092787749,25.030082735839));
#17007=CARTESIAN_POINT('Ctrl Pts',(1.54682436238642,-1.25988087772748,25.0320712101852));
#17008=CARTESIAN_POINT('Ctrl Pts',(1.59757961749283,-1.19557453135403,25.03744841836));
#17009=CARTESIAN_POINT('Ctrl Pts',(1.62779379377285,-1.15409952051872,25.0408747181047));
#17010=CARTESIAN_POINT('Ctrl Pts',(1.7125433396656,-1.02780550294126,25.0511832837765));
#17011=CARTESIAN_POINT('Ctrl Pts',(1.76228246845434,-0.939971293937737,
25.0582024793581));
#17012=CARTESIAN_POINT('Ctrl Pts',(1.84140073235156,-0.771700978370523,
25.0711756313807));
#17013=CARTESIAN_POINT('Ctrl Pts',(1.87266489551997,-0.692392317305198,
25.0771102018213));
#17014=CARTESIAN_POINT('Ctrl Pts',(1.91019762187873,-0.575816023739283,
25.0853877873001));
#17015=CARTESIAN_POINT('Ctrl Pts',(1.92063229033387,-0.539991754106582,
25.0878726528258));
#17016=CARTESIAN_POINT('Ctrl Pts',(1.93156203286626,-0.49812767712736,25.0906925137743));
#17017=CARTESIAN_POINT('Ctrl Pts',(1.93304145916679,-0.492355348155817,
25.0910794888549));
#17018=CARTESIAN_POINT('Ctrl Pts',(1.93535949081565,-0.483139486498522,
25.0916942994721));
#17019=CARTESIAN_POINT('Ctrl Pts',(1.93621480950124,-0.479700254376378,
25.0919230697235));
#17020=CARTESIAN_POINT('Ctrl Pts',(1.93770951607528,-0.473620916431468,
25.0923262515093));
#17021=CARTESIAN_POINT('Ctrl Pts',(1.93835268222469,-0.470981762748864,
25.0925008799186));
#17022=CARTESIAN_POINT('Ctrl Pts',(1.93969419203956,-0.465427746969418,
25.0928675307246));
#17023=CARTESIAN_POINT('Ctrl Pts',(1.94039135598954,-0.462512629203602,
25.0930594845218));
#17024=CARTESIAN_POINT('Ctrl Pts',(1.94222767790006,-0.454757009309252,
25.0935689016688));
#17025=CARTESIAN_POINT('Ctrl Pts',(1.94335531988057,-0.44991376094942,25.0938857071792));
#17026=CARTESIAN_POINT('Ctrl Pts',(1.94852203638172,-0.427340721807538,
25.0953563403367));
#17027=CARTESIAN_POINT('Ctrl Pts',(1.95233682679962,-0.409559751454695,
25.0964978168665));
#17028=CARTESIAN_POINT('Ctrl Pts',(1.98661881322881,-0.238389054834851,
25.1073458660057));
#17029=CARTESIAN_POINT('Ctrl Pts',(1.99919564234486,-0.0819470161938231,
25.1162121936474));
#17030=CARTESIAN_POINT('Ctrl Pts',(1.98865459414495,0.200564536396305,25.1326716628265));
#17031=CARTESIAN_POINT('Ctrl Pts',(1.97197607481659,0.326001148856512,25.1401419867168));
#17032=CARTESIAN_POINT('Ctrl Pts',(1.94062866068086,0.461689626740882,25.1488339543987));
#17033=CARTESIAN_POINT('Ctrl Pts',(1.93757545531006,0.474339806781253,25.1496500308768));
#17034=CARTESIAN_POINT('Ctrl Pts',(1.93287381458685,0.493016632630669,25.1508637380492));
#17035=CARTESIAN_POINT('Ctrl Pts',(1.93132044786469,0.499067038967568,25.1512583016611));
#17036=CARTESIAN_POINT('Ctrl Pts',(1.92851187615533,0.509796997967594,25.1519605257441));
#17037=CARTESIAN_POINT('Ctrl Pts',(1.92726798780158,0.514479482706144,25.1522678177598));
#17038=CARTESIAN_POINT('Ctrl Pts',(1.92462081592243,0.524300150133571,25.152914105753));
#17039=CARTESIAN_POINT('Ctrl Pts',(1.92321398841665,0.529437329967593,25.1532532146637));
#17040=CARTESIAN_POINT('Ctrl Pts',(1.91946474980384,0.54291592606885,25.1541457033592));
#17041=CARTESIAN_POINT('Ctrl Pts',(1.91708855835524,0.551247751935289,25.1547001781214));
#17042=CARTESIAN_POINT('Ctrl Pts',(1.90618314158928,0.58856279687398,25.1571961636292));
#17043=CARTESIAN_POINT('Ctrl Pts',(1.89705077685446,0.617364170174376,25.1591572592904));
#17044=CARTESIAN_POINT('Ctrl Pts',(1.87096583212223,0.693576895376227,25.1644427161337));
#17045=CARTESIAN_POINT('Ctrl Pts',(1.85286732378634,0.740570063176308,25.1678030847046));
#17046=CARTESIAN_POINT('Ctrl Pts',(1.79355256349569,0.878751531526024,25.1779870175077));
#17047=CARTESIAN_POINT('Ctrl Pts',(1.74723694013402,0.967571604557962,25.1849478177556));
#17048=CARTESIAN_POINT('Ctrl Pts',(1.62942935987013,1.15722823864101,25.2005255827653));
#17049=CARTESIAN_POINT('Ctrl Pts',(1.55482702089374,1.25568213924491,25.2091225372248));
#17050=CARTESIAN_POINT('Ctrl Pts',(1.46650390259364,1.35220226100939,25.2176642117622));
#17051=CARTESIAN_POINT('Ctrl Pts',(1.46137142972671,1.35774747276934,25.2181553176304));
#17052=CARTESIAN_POINT('Ctrl Pts',(1.45381492270092,1.36581916401153,25.2188705527326));
#17053=CARTESIAN_POINT('Ctrl Pts',(1.45141562518083,1.36836855477227,25.2190965102177));
#17054=CARTESIAN_POINT('Ctrl Pts',(1.44714695153783,1.37288040581725,25.2194964809223));
#17055=CARTESIAN_POINT('Ctrl Pts',(1.44528027469255,1.37484538620069,25.2196706994773));
#17056=CARTESIAN_POINT('Ctrl Pts',(1.44132508237051,1.37899191082734,25.2200383841626));
#17057=CARTESIAN_POINT('Ctrl Pts',(1.43923562158321,1.38117251241863,25.220231774419));
#17058=CARTESIAN_POINT('Ctrl Pts',(1.4336220092909,1.38700441538083,25.2207490943302));
#17059=CARTESIAN_POINT('Ctrl Pts',(1.43008883407581,1.39064705868255,25.2210723295686));
#17060=CARTESIAN_POINT('Ctrl Pts',(1.4130643138257,1.4080655503945,25.22261877048));
#17061=CARTESIAN_POINT('Ctrl Pts',(1.39938704075417,1.4216593566299,25.2238280229595));
#17062=CARTESIAN_POINT('Ctrl Pts',(1.36064190698567,1.45906697956981,25.2271699329368));
#17063=CARTESIAN_POINT('Ctrl Pts',(1.33514796046321,1.48243147124427,25.229273964634));
#17064=CARTESIAN_POINT('Ctrl Pts',(1.23989624063009,1.56527522918585,25.2368529452548));
#17065=CARTESIAN_POINT('Ctrl Pts',(1.16666583658701,1.62059320225945,25.242152745272));
#17066=CARTESIAN_POINT('Ctrl Pts',(0.959419053620506,1.75579277432634,25.2565040421057));
#17067=CARTESIAN_POINT('Ctrl Pts',(0.819453601606901,1.82531633140499,25.2655795428492));
#17068=CARTESIAN_POINT('Ctrl Pts',(0.660994947086356,1.88209230981788,25.2760905708652));
#17069=CARTESIAN_POINT('Ctrl Pts',(0.649113895048487,1.8862229249087,25.2768796545449));
#17070=CARTESIAN_POINT('Ctrl Pts',(0.631356503317253,1.89220889096321,25.2780607856478));
#17071=CARTESIAN_POINT('Ctrl Pts',(0.625509189245483,1.89414988163734,25.2784500025495));
#17072=CARTESIAN_POINT('Ctrl Pts',(0.615057740853982,1.89756552191504,25.2791462303498));
#17073=CARTESIAN_POINT('Ctrl Pts',(0.61045704111994,1.89905058774584,25.2794528954159));
#17074=CARTESIAN_POINT('Ctrl Pts',(0.601167635079508,1.90201188222467,25.280072489065));
#17075=CARTESIAN_POINT('Ctrl Pts',(0.596478781267086,1.90348753302351,25.2803854341549));
#17076=CARTESIAN_POINT('Ctrl Pts',(0.583983428860944,1.90736930040159,25.281219969518));
#17077=CARTESIAN_POINT('Ctrl Pts',(0.576167587145081,1.90974480010562,25.2817425584719));
#17078=CARTESIAN_POINT('Ctrl Pts',(0.559092958117396,1.91482000149295,25.2828855785421));
#17079=CARTESIAN_POINT('Ctrl Pts',(0.549828778280709,1.91750068658948,25.283506616645));
#17080=CARTESIAN_POINT('Ctrl Pts',(0.522834370146129,1.92510008418684,25.2853189058666));
#17081=CARTESIAN_POINT('Ctrl Pts',(0.505055456178126,1.92984068288694,25.2865158620665));
#17082=CARTESIAN_POINT('Ctrl Pts',(0.443639074286026,1.94531004451985,25.2906630637096));
#17083=CARTESIAN_POINT('Ctrl Pts',(0.399708790363694,1.95480923933301,25.2936512515341));
#17084=CARTESIAN_POINT('Ctrl Pts',(0.173303818173071,1.99581485446975,25.3091609518814));
#17085=CARTESIAN_POINT('Ctrl Pts',(-0.0125627512863938,2.00328165767449,
25.3223660965633));
#17086=CARTESIAN_POINT('Ctrl Pts',(-0.205872429791445,1.9841188672704,25.3355976124627));
#17087=CARTESIAN_POINT('Ctrl Pts',(-0.214963567943442,1.98315450890887,
25.3362184251348));
#17088=CARTESIAN_POINT('Ctrl Pts',(-0.262654926561549,1.9777637622472,25.3394665218398));
#17089=CARTESIAN_POINT('Ctrl Pts',(-0.30112949358743,1.97227245371955,25.3420572794784));
#17090=CARTESIAN_POINT('Ctrl Pts',(-0.345940196942792,1.96453472753261,
25.3450214157219));
#17091=CARTESIAN_POINT('Ctrl Pts',(-0.352452816560508,1.96337676736608,
25.3454508835194));
#17092=CARTESIAN_POINT('Ctrl Pts',(-0.362300709367983,1.96157520748857,
25.3460981561912));
#17093=CARTESIAN_POINT('Ctrl Pts',(-0.365640216612522,1.96095546381316,
25.3463172795906));
#17094=CARTESIAN_POINT('Ctrl Pts',(-0.371624495345527,1.95982908647198,
25.3467092529198));
#17095=CARTESIAN_POINT('Ctrl Pts',(-0.374269827063037,1.95932562647602,
25.3468822809883));
#17096=CARTESIAN_POINT('Ctrl Pts',(-0.379979511768562,1.95822697287139,
25.3472552182032));
#17097=CARTESIAN_POINT('Ctrl Pts',(-0.383043478596804,1.95762994472311,
25.3474550207829));
#17098=CARTESIAN_POINT('Ctrl Pts',(-0.391533831439984,1.9559548636944,25.348007809767));
#17099=CARTESIAN_POINT('Ctrl Pts',(-0.396957205147604,1.95486141427164,
25.3483599274359));
#17100=CARTESIAN_POINT('Ctrl Pts',(-0.426986673208195,1.94867681194214,
25.3503045000139));
#17101=CARTESIAN_POINT('Ctrl Pts',(-0.451500743017651,1.94314337053519,
25.3518728537722));
#17102=CARTESIAN_POINT('Ctrl Pts',(-0.633543265873735,1.89842042511688,
25.3634212358615));
#17103=CARTESIAN_POINT('Ctrl Pts',(-0.78588523078916,1.8405911992282,25.37257287806));
#17104=CARTESIAN_POINT('Ctrl Pts',(-1.02905128753731,1.71252104917088,25.3886372441771));
#17105=CARTESIAN_POINT('Ctrl Pts',(-1.12393032684882,1.65180208095046,25.3953364334316));
#17106=CARTESIAN_POINT('Ctrl Pts',(-1.22345443788887,1.57554888302259,25.4031624465996));
#17107=CARTESIAN_POINT('Ctrl Pts',(-1.23365026270109,1.56757840669953,25.4039740613711));
#17108=CARTESIAN_POINT('Ctrl Pts',(-1.24864032139483,1.55562326922265,25.4051823899399));
#17109=CARTESIAN_POINT('Ctrl Pts',(-1.25349473546096,1.55171432767096,25.4055760763858));
#17110=CARTESIAN_POINT('Ctrl Pts',(-1.26208861649509,1.54472759488179,25.4062773118063));
#17111=CARTESIAN_POINT('Ctrl Pts',(-1.26583536050546,1.54165880067281,25.4065844960429));
#17112=CARTESIAN_POINT('Ctrl Pts',(-1.26961518176168,1.53853984545137,25.4068958847872));
#17113=CARTESIAN_POINT('Ctrl Pts',(-1.26965949729428,1.53850327485241,25.4068995357919));
#17114=CARTESIAN_POINT('Ctrl Pts',(-1.26974649857748,1.53843147228389,25.406906703938));
#17115=CARTESIAN_POINT('Ctrl Pts',(-1.26978918487027,1.5383962400987,25.4069102211091));
#17116=CARTESIAN_POINT('Ctrl Pts',(-1.26987300193491,1.53832705375073,25.4069171276624));
#17117=CARTESIAN_POINT('Ctrl Pts',(-1.26991413294785,1.53829309960223,25.4069205170507));
#17118=CARTESIAN_POINT('Ctrl Pts',(-1.26999490917778,1.53822641240021,25.4069271737433));
#17119=CARTESIAN_POINT('Ctrl Pts',(-1.27003455464942,1.53819367933285,25.4069304410558));
#17120=CARTESIAN_POINT('Ctrl Pts',(-1.27011242570285,1.5381293804595,25.4069368589908));
#17121=CARTESIAN_POINT('Ctrl Pts',(-1.27015065153884,1.53809781462458,25.4069400096225));
#17122=CARTESIAN_POINT('Ctrl Pts',(-1.27022574561321,1.53803579931277,25.4069461992954));
#17123=CARTESIAN_POINT('Ctrl Pts',(-1.27026261412418,1.53800534977765,25.4069492383482));
#17124=CARTESIAN_POINT('Ctrl Pts',(-1.27033505244023,1.53794551892126,25.4069552096858));
#17125=CARTESIAN_POINT('Ctrl Pts',(-1.27037062255348,1.53791613749949,25.406958141986));
#17126=CARTESIAN_POINT('Ctrl Pts',(-1.27044051988546,1.53785839722504,25.4069639043897));
#17127=CARTESIAN_POINT('Ctrl Pts',(-1.27047484740529,1.53783003826589,25.4069667345089));
#17128=CARTESIAN_POINT('Ctrl Pts',(-1.27054231236415,1.53777429970718,25.4069722968775));
#17129=CARTESIAN_POINT('Ctrl Pts',(-1.2705754501318,1.5377469199676,25.4069750291455));
#17130=CARTESIAN_POINT('Ctrl Pts',(-1.27064058564112,1.53769309888039,25.4069803999137));
#17131=CARTESIAN_POINT('Ctrl Pts',(-1.27067258373281,1.53766665736514,25.4069830384348));
#17132=CARTESIAN_POINT('Ctrl Pts',(-1.27073548737102,1.53761467385142,25.4069882256012));
#17133=CARTESIAN_POINT('Ctrl Pts',(-1.27076639328057,1.53758913166551,25.4069907742691));
#17134=CARTESIAN_POINT('Ctrl Pts',(-1.27082715756168,1.53753890994798,25.4069957854189));
#17135=CARTESIAN_POINT('Ctrl Pts',(-1.27085701633089,1.53751423019196,25.4069982479268));
#17136=CARTESIAN_POINT('Ctrl Pts',(-1.27091572911641,1.53746569827937,25.4070030902652));
#17137=CARTESIAN_POINT('Ctrl Pts',(-1.27094458352759,1.53744184589302,25.4070054701221));
#17138=CARTESIAN_POINT('Ctrl Pts',(-1.27100132818265,1.53739493545644,25.4070101504871));
#17139=CARTESIAN_POINT('Ctrl Pts',(-1.2710292188541,1.53737187714237,25.4070124510248));
#17140=CARTESIAN_POINT('Ctrl Pts',(-1.27108407463135,1.53732652320266,25.4070169759185));
#17141=CARTESIAN_POINT('Ctrl Pts',(-1.27111104017678,1.53730422729675,25.4070192003053));
#17142=CARTESIAN_POINT('Ctrl Pts',(-1.27116408238187,1.53726036809214,25.407023575907));
#17143=CARTESIAN_POINT('Ctrl Pts',(-1.27119015950882,1.53723880448432,25.4070257271554));
#17144=CARTESIAN_POINT('Ctrl Pts',(-1.27124145980536,1.53719638122225,25.4070299593467));
#17145=CARTESIAN_POINT('Ctrl Pts',(-1.27126668345654,1.53717552124154,25.4070320403248));
#17146=CARTESIAN_POINT('Ctrl Pts',(-1.27131630996516,1.53713447802036,25.4070361346978));
#17147=CARTESIAN_POINT('Ctrl Pts',(-1.27134071336545,1.53711429439768,25.4070381481332));
#17148=CARTESIAN_POINT('Ctrl Pts',(-1.27138873104009,1.53707457789883,25.4070421100208));
#17149=CARTESIAN_POINT('Ctrl Pts',(-1.27141234585355,1.53705504463884,25.4070440585135));
#17150=CARTESIAN_POINT('Ctrl Pts',(-1.27145881654325,1.53701660407873,25.4070478929946));
#17151=CARTESIAN_POINT('Ctrl Pts',(-1.27148167295819,1.5369976963908,25.4070497790238));
#17152=CARTESIAN_POINT('Ctrl Pts',(-1.27574962478244,1.53346692543189,25.4074019654472));
#17153=CARTESIAN_POINT('Ctrl Pts',(-1.27998011785712,1.52993751944739,25.4077529796671));
#17154=CARTESIAN_POINT('Ctrl Pts',(-1.29153622893392,1.52021503434459,25.4087171319949));
#17155=CARTESIAN_POINT('Ctrl Pts',(-1.29883180586143,1.51398663007387,25.4093317165086));
#17156=CARTESIAN_POINT('Ctrl Pts',(-1.31495396252914,1.50002047177767,25.4107031879422));
#17157=CARTESIAN_POINT('Ctrl Pts',(-1.32375768372676,1.49225699003033,25.4114611310597));
#17158=CARTESIAN_POINT('Ctrl Pts',(-1.35045093437283,1.46829568855202,25.4137873300332));
#17159=CARTESIAN_POINT('Ctrl Pts',(-1.36811493896041,1.45185102016609,25.4153658545363));
#17160=CARTESIAN_POINT('Ctrl Pts',(-1.43309189406048,1.38912049028472,25.4213231071439));
#17161=CARTESIAN_POINT('Ctrl Pts',(-1.47838608368565,1.34081361978432,25.4257857602523));
#17162=CARTESIAN_POINT('Ctrl Pts',(-1.6464999015215,1.14262431408354,25.4435933239477));
#17163=CARTESIAN_POINT('Ctrl Pts',(-1.74961403818921,0.977445694349946,
25.4575012252794));
#17164=CARTESIAN_POINT('Ctrl Pts',(-1.83205831167327,0.789132852286655,
25.4710191590031));
#17165=CARTESIAN_POINT('Ctrl Pts',(-1.83671947784287,0.77822226403292,25.4717942380369));
#17166=CARTESIAN_POINT('Ctrl Pts',(-1.84297012791455,0.763222055011605,
25.4728481053546));
#17167=CARTESIAN_POINT('Ctrl Pts',(-1.8446437626905,0.759168088964304,25.4731317577943));
#17168=CARTESIAN_POINT('Ctrl Pts',(-1.84728113973141,0.752719480200086,
25.4735810729072));
#17169=CARTESIAN_POINT('Ctrl Pts',(-1.84825361549842,0.750328460118517,
25.4737472591281));
#17170=CARTESIAN_POINT('Ctrl Pts',(-1.85024719710819,0.745399460660219,
25.474088989483));
#17171=CARTESIAN_POINT('Ctrl Pts',(-1.85126772157716,0.742861272030986,
25.4742644952618));
#17172=CARTESIAN_POINT('Ctrl Pts',(-1.85366729200975,0.736857547005966,
25.4746785387774));
#17173=CARTESIAN_POINT('Ctrl Pts',(-1.85504185417118,0.733390205736809,
25.4749168057301));
#17174=CARTESIAN_POINT('Ctrl Pts',(-1.85955157316575,0.721920614458185,
25.4757022055144));
#17175=CARTESIAN_POINT('Ctrl Pts',(-1.86264479308468,0.713901819598324,
25.4762468735828));
#17176=CARTESIAN_POINT('Ctrl Pts',(-1.90319204420191,0.606730267578278,
25.4834706295395));
#17177=CARTESIAN_POINT('Ctrl Pts',(-1.93274312340243,0.504749843138312,
25.4897143119683));
#17178=CARTESIAN_POINT('Ctrl Pts',(-1.98104299422856,0.269322839103342,
25.5037084226064));
#17179=CARTESIAN_POINT('Ctrl Pts',(-1.99467637956076,0.135379192454375,
25.5113976063033));
#17180=CARTESIAN_POINT('Ctrl Pts',(-1.99474970266067,0.00108914423437002,
25.5194706385773));
#17181=CARTESIAN_POINT('',(-1.99774652581851,-0.000397439823534614,27.121064794965));
#17182=CARTESIAN_POINT('Ctrl Pts',(-1.99474970399463,0.00108669836046226,
25.5194707856144));
#17183=CARTESIAN_POINT('Ctrl Pts',(-1.99477864875537,-0.0520444694238004,
25.5226648409668));
#17184=CARTESIAN_POINT('Ctrl Pts',(-1.99268484369696,-0.105152553496392,
25.525910525209));
#17185=CARTESIAN_POINT('Ctrl Pts',(-1.98770903672266,-0.167730301252841,
25.5298244945845));
#17186=CARTESIAN_POINT('Ctrl Pts',(-1.98687443595081,-0.177343280728575,
25.5304282250247));
#17187=CARTESIAN_POINT('Ctrl Pts',(-1.98539402199652,-0.193069746082949,
25.5314201301886));
#17188=CARTESIAN_POINT('Ctrl Pts',(-1.98478962838246,-0.199187045601989,
25.5318070107077));
#17189=CARTESIAN_POINT('Ctrl Pts',(-1.98366966429628,-0.210011056358707,
25.5324934584308));
#17190=CARTESIAN_POINT('Ctrl Pts',(-1.98316559096884,-0.214718930257409,
25.5327926632004));
#17191=CARTESIAN_POINT('Ctrl Pts',(-1.98213581040468,-0.224023657046903,
25.5333852948594));
#17192=CARTESIAN_POINT('Ctrl Pts',(-1.98161086148757,-0.228620565236366,
25.5336786961248));
#17193=CARTESIAN_POINT('Ctrl Pts',(-1.98053342780961,-0.237772919096294,
25.5342640997872));
#17194=CARTESIAN_POINT('Ctrl Pts',(-1.97998120732606,-0.242328367680629,
25.5345560921402));
#17195=CARTESIAN_POINT('Ctrl Pts',(-1.9784694140785,-0.254449403544559,
25.5353346810353));
#17196=CARTESIAN_POINT('Ctrl Pts',(-1.97748217253519,-0.262011404404,25.5358221481648));
#17197=CARTESIAN_POINT('Ctrl Pts',(-1.97378249076125,-0.289137236450202,
25.5375770682697));
#17198=CARTESIAN_POINT('Ctrl Pts',(-1.97082295538693,-0.308665667319003,
25.5388522942848));
#17199=CARTESIAN_POINT('Ctrl Pts',(-1.96679912246105,-0.332792672738863,
25.5404430042626));
#17200=CARTESIAN_POINT('Ctrl Pts',(-1.96600777458543,-0.337436187717719,
25.5407498529842));
#17201=CARTESIAN_POINT('Ctrl Pts',(-1.96432787954298,-0.347087030740639,
25.5413890535205));
#17202=CARTESIAN_POINT('Ctrl Pts',(-1.96343661677771,-0.352093845963292,
25.5417214878768));
#17203=CARTESIAN_POINT('Ctrl Pts',(-1.96024240326387,-0.369648529909305,
25.5428899482147));
#17204=CARTESIAN_POINT('Ctrl Pts',(-1.95783827062313,-0.3821774574721,25.5437290834988));
#17205=CARTESIAN_POINT('Ctrl Pts',(-1.94949663589628,-0.423503150266057,
25.5465142362819));
#17206=CARTESIAN_POINT('Ctrl Pts',(-1.94304284970025,-0.452190660058426,
25.5484756149738));
#17207=CARTESIAN_POINT('Ctrl Pts',(-1.89123154692902,-0.660843664870152,
25.5629451046473));
#17208=CARTESIAN_POINT('Ctrl Pts',(-1.82159886484378,-0.833805591687323,
25.5761740976607));
#17209=CARTESIAN_POINT('Ctrl Pts',(-1.71211966430217,-1.02412448254609,
25.5911507781912));
#17210=CARTESIAN_POINT('Ctrl Pts',(-1.69440540703044,-1.05317391897498,
25.5934458506026));
#17211=CARTESIAN_POINT('Ctrl Pts',(-1.66561893046525,-1.09777250078535,
25.5969678330164));
#17212=CARTESIAN_POINT('Ctrl Pts',(-1.65505260113188,-1.11363900725513,
25.5982204844435));
#17213=CARTESIAN_POINT('Ctrl Pts',(-1.64139828641327,-1.13351875876011,
25.5997871213441));
#17214=CARTESIAN_POINT('Ctrl Pts',(-1.63852071950873,-1.13767436650348,
25.600114446007));
#17215=CARTESIAN_POINT('Ctrl Pts',(-1.63390119445739,-1.14429172110258,
25.6006353594349));
#17216=CARTESIAN_POINT('Ctrl Pts',(-1.6321694199426,-1.14676049859343,25.6008296292908));
#17217=CARTESIAN_POINT('Ctrl Pts',(-1.62886992297318,-1.15144156965472,
25.6011978371068));
#17218=CARTESIAN_POINT('Ctrl Pts',(-1.62730330778364,-1.15365456652143,
25.6013718435343));
#17219=CARTESIAN_POINT('Ctrl Pts',(-1.62369884132374,-1.1587242762833,25.601770332676));
#17220=CARTESIAN_POINT('Ctrl Pts',(-1.62165796287589,-1.16157880820284,
25.6019946043177));
#17221=CARTESIAN_POINT('Ctrl Pts',(-1.61620062536082,-1.16916945028297,
25.6025907533652));
#17222=CARTESIAN_POINT('Ctrl Pts',(-1.6127708513584,-1.17389601240402,25.602961731871));
#17223=CARTESIAN_POINT('Ctrl Pts',(-1.58870393238541,-1.20675799676233,
25.6055398962061));
#17224=CARTESIAN_POINT('Ctrl Pts',(-1.56735093539493,-1.23436479702641,
25.6077000987887));
#17225=CARTESIAN_POINT('Ctrl Pts',(-1.54073273981344,-1.26697354625184,
25.6102639542189));
#17226=CARTESIAN_POINT('Ctrl Pts',(-1.53615220418561,-1.27252337916334,
25.6107007487528));
#17227=CARTESIAN_POINT('Ctrl Pts',(-1.42433724646804,-1.40651617035846,
25.621260595513));
#17228=CARTESIAN_POINT('Ctrl Pts',(-1.30138765723827,-1.52099482943121,
25.6306497529312));
#17229=CARTESIAN_POINT('Ctrl Pts',(-1.11622624933578,-1.65431692984031,
25.6441128832599));
#17230=CARTESIAN_POINT('Ctrl Pts',(-1.06528135306669,-1.68757229534346,
25.6477512160482));
#17231=CARTESIAN_POINT('Ctrl Pts',(-0.993286704744341,-1.73000792544056,
25.6528638217586));
#17232=CARTESIAN_POINT('Ctrl Pts',(-0.973477406028795,-1.74123162623372,
25.6542675030687));
#17233=CARTESIAN_POINT('Ctrl Pts',(-0.943597971386984,-1.75749168672217,
25.6563826589878));
#17234=CARTESIAN_POINT('Ctrl Pts',(-0.933669843593652,-1.76278608331482,
25.6570851238751));
#17235=CARTESIAN_POINT('Ctrl Pts',(-0.915465337038046,-1.77229711055161,
25.6583728577642));
#17236=CARTESIAN_POINT('Ctrl Pts',(-0.907203235712548,-1.77654049090059,
25.6589571731339));
#17237=CARTESIAN_POINT('Ctrl Pts',(-0.894064416504118,-1.78317297751809,
25.6598863182768));
#17238=CARTESIAN_POINT('Ctrl Pts',(-0.889206989527557,-1.78560017289269,
25.6602298098434));
#17239=CARTESIAN_POINT('Ctrl Pts',(-0.884316295315165,-1.78801908631444,
25.6605756548241));
#17240=CARTESIAN_POINT('Ctrl Pts',(-0.884292839033272,-1.7880306871022,
25.6605773135329));
#17241=CARTESIAN_POINT('Ctrl Pts',(-0.884245628714148,-1.78805403478252,
25.6605806520062));
#17242=CARTESIAN_POINT('Ctrl Pts',(-0.884221874858119,-1.78806578157084,
25.660582331758));
#17243=CARTESIAN_POINT('Ctrl Pts',(-0.884174065173737,-1.78808942329354,
25.6605857126155));
#17244=CARTESIAN_POINT('Ctrl Pts',(-0.884150009408023,-1.78810131818191,
25.6605874137168));
#17245=CARTESIAN_POINT('Ctrl Pts',(-0.884101591323205,-1.78812525832456,
25.6605908375974));
#17246=CARTESIAN_POINT('Ctrl Pts',(-0.884077229137599,-1.78813730349739,
25.6605925603672));
#17247=CARTESIAN_POINT('Ctrl Pts',(-0.884028193735618,-1.78816154637605,
25.6605960279014));
#17248=CARTESIAN_POINT('Ctrl Pts',(-0.884003520605003,-1.78817374402361,
25.6605977726597));
#17249=CARTESIAN_POINT('Ctrl Pts',(-0.88395385868617,-1.78819829409122,
25.6606012844981));
#17250=CARTESIAN_POINT('Ctrl Pts',(-0.883928869990882,-1.78821064644901,
25.6606030515717));
#17251=CARTESIAN_POINT('Ctrl Pts',(-0.883878572263243,-1.78823550820099,
25.6606066083714));
#17252=CARTESIAN_POINT('Ctrl Pts',(-0.883853263324179,-1.78824801753229,
25.660608398091));
#17253=CARTESIAN_POINT('Ctrl Pts',(-0.883802320262145,-1.78827319557633,
25.6606120005256));
#17254=CARTESIAN_POINT('Ctrl Pts',(-0.883776686272227,-1.78828586420606,
25.6606138132312));
#17255=CARTESIAN_POINT('Ctrl Pts',(-0.883725088377709,-1.78831136313296,
25.6606174619724));
#17256=CARTESIAN_POINT('Ctrl Pts',(-0.883699124529804,-1.78832419338439,
25.660619298004));
#17257=CARTESIAN_POINT('Ctrl Pts',(-0.883646861939137,-1.78835001796223,
25.6606229937493));
#17258=CARTESIAN_POINT('Ctrl Pts',(-0.883620563290989,-1.78836301222368,
25.6606248534563));
#17259=CARTESIAN_POINT('Ctrl Pts',(-0.883567626114362,-1.78838916722994,
25.6606285969051));
#17260=CARTESIAN_POINT('Ctrl Pts',(-0.883540987661871,-1.78840232791848,
25.6606304806415));
#17261=CARTESIAN_POINT('Ctrl Pts',(-0.883487365828111,-1.78842881821666,
25.6606342725059));
#17262=CARTESIAN_POINT('Ctrl Pts',(-0.88346038249933,-1.7884421477811,25.6606361806303));
#17263=CARTESIAN_POINT('Ctrl Pts',(-0.883406064966736,-1.78846897871039,
25.6606400216913));
#17264=CARTESIAN_POINT('Ctrl Pts',(-0.883378730823474,-1.7884824800254,
25.6606419546236));
#17265=CARTESIAN_POINT('Ctrl Pts',(-0.883325223270455,-1.78850890780177,
25.6606457384071));
#17266=CARTESIAN_POINT('Ctrl Pts',(-0.88329904764392,-1.78852183542261,
25.6606475894151));
#17267=CARTESIAN_POINT('Ctrl Pts',(-0.883245212885875,-1.78854842186774,
25.6606513963371));
#17268=CARTESIAN_POINT('Ctrl Pts',(-0.883217554049297,-1.78856208046313,
25.6606533522303));
#17269=CARTESIAN_POINT('Ctrl Pts',(-0.883160667422736,-1.78859017079928,
25.6606573749653));
#17270=CARTESIAN_POINT('Ctrl Pts',(-0.883131439891513,-1.78860460231923,
25.6606594417887));
#17271=CARTESIAN_POINT('Ctrl Pts',(-0.883071325402392,-1.78863428289252,
25.6606636927822));
#17272=CARTESIAN_POINT('Ctrl Pts',(-0.883040438667561,-1.78864953173175,
25.6606658769363));
#17273=CARTESIAN_POINT('Ctrl Pts',(-0.882976910296061,-1.78868089376194,
25.6606703693426));
#17274=CARTESIAN_POINT('Ctrl Pts',(-0.882944268887404,-1.7886970067242,
25.6606726775786));
#17275=CARTESIAN_POINT('Ctrl Pts',(-0.878574451415106,-1.79085395554171,
25.6609816890757));
#17276=CARTESIAN_POINT('Ctrl Pts',(-0.874229536845616,-1.79297899401761,
25.661288941372));
#17277=CARTESIAN_POINT('Ctrl Pts',(-0.864314891262726,-1.79778350549814,
25.6619900851228));
#17278=CARTESIAN_POINT('Ctrl Pts',(-0.858740370195685,-1.80045292609238,
25.662384322539));
#17279=CARTESIAN_POINT('Ctrl Pts',(-0.84169392356628,-1.80851862755688,
25.6635899812172));
#17280=CARTESIAN_POINT('Ctrl Pts',(-0.83018305748607,-1.81383140504161,
25.6644042760221));
#17281=CARTESIAN_POINT('Ctrl Pts',(-0.732337026640794,-1.8578651983485,
25.6713284603613));
#17282=CARTESIAN_POINT('Ctrl Pts',(-0.64341138965896,-1.89050194453488,
25.677646094022));
#17283=CARTESIAN_POINT('Ctrl Pts',(-0.434635845709935,-1.95068449279221,
25.6925172173992));
#17284=CARTESIAN_POINT('Ctrl Pts',(-0.313874224238932,-1.97371678918793,
25.7011550429326));
#17285=CARTESIAN_POINT('Ctrl Pts',(-0.136089932802466,-1.99088844185003,
25.7135235544777));
#17286=CARTESIAN_POINT('Ctrl Pts',(-0.0801992898656494,-1.99392233875122,
25.7173588056173));
#17287=CARTESIAN_POINT('Ctrl Pts',(0.00252348216109496,-1.9949281144154,
25.722893859219));
#17288=CARTESIAN_POINT('Ctrl Pts',(0.029303629749624,-1.99471452137963,
25.724663729083));
#17289=CARTESIAN_POINT('Ctrl Pts',(0.0617114573816073,-1.99380316899235,
25.726772499811));
#17290=CARTESIAN_POINT('Ctrl Pts',(0.0673493722532456,-1.99362068723922,
25.7271381459563));
#17291=CARTESIAN_POINT('Ctrl Pts',(0.0761297242379217,-1.99329920497823,
25.727705627592));
#17292=CARTESIAN_POINT('Ctrl Pts',(0.0792726789278182,-1.99317668514128,
25.7279083667849));
#17293=CARTESIAN_POINT('Ctrl Pts',(0.08510363008286,-1.99293556689998,25.7282837526516));
#17294=CARTESIAN_POINT('Ctrl Pts',(0.0877916507410601,-1.99281896515401,
25.7284565067773));
#17295=CARTESIAN_POINT('Ctrl Pts',(0.0938407044030223,-1.99254430460726,
25.7288446087131));
#17296=CARTESIAN_POINT('Ctrl Pts',(0.0972015680904663,-1.99238318081486,
25.7290597823846));
#17297=CARTESIAN_POINT('Ctrl Pts',(0.105794302577378,-1.99194944072073,
25.7296087874463));
#17298=CARTESIAN_POINT('Ctrl Pts',(0.1110255767775,-1.99166471365752,25.7299419510193));
#17299=CARTESIAN_POINT('Ctrl Pts',(0.141092151570577,-1.98990942432509,
25.7318509463703));
#17300=CARTESIAN_POINT('Ctrl Pts',(0.165900660110943,-1.9879948745994,25.7334031411506));
#17301=CARTESIAN_POINT('Ctrl Pts',(0.39466952605564,-1.96602741558078,25.7475577469129));
#17302=CARTESIAN_POINT('Ctrl Pts',(0.594457564142217,-1.91511710448562,
25.7588649070505));
#17303=CARTESIAN_POINT('Ctrl Pts',(0.827221246453771,-1.81577633732689,
25.7739450648069));
#17304=CARTESIAN_POINT('Ctrl Pts',(0.870737583357324,-1.79531452617533,
25.7768474743026));
#17305=CARTESIAN_POINT('Ctrl Pts',(0.930632560316081,-1.764461194807,25.7809877021675));
#17306=CARTESIAN_POINT('Ctrl Pts',(0.947665253100583,-1.75537198304105,
25.7821820494005));
#17307=CARTESIAN_POINT('Ctrl Pts',(0.973302588009724,-1.74120915659556,
25.7840071263342));
#17308=CARTESIAN_POINT('Ctrl Pts',(0.982005774331486,-1.73631561310041,
25.784631551375));
#17309=CARTESIAN_POINT('Ctrl Pts',(0.997990221366245,-1.72716941172006,
25.7857875905996));
#17310=CARTESIAN_POINT('Ctrl Pts',(1.00528199285063,-1.72293550954634,25.7863185268859));
#17311=CARTESIAN_POINT('Ctrl Pts',(1.01705416968354,-1.71599992682536,25.787181606723));
#17312=CARTESIAN_POINT('Ctrl Pts',(1.02155122629428,-1.71332659587749,25.7875127190309));
#17313=CARTESIAN_POINT('Ctrl Pts',(1.03018977175762,-1.70814520422992,25.7881515089942));
#17314=CARTESIAN_POINT('Ctrl Pts',(1.03433275265107,-1.70563969251474,25.7884590918867));
#17315=CARTESIAN_POINT('Ctrl Pts',(1.04377832705844,-1.69988031094873,25.7891631743345));
#17316=CARTESIAN_POINT('Ctrl Pts',(1.0490748815663,-1.69661668004448,25.7895600305664));
#17317=CARTESIAN_POINT('Ctrl Pts',(1.0652931086993,-1.68651835176321,25.7907815746728));
#17318=CARTESIAN_POINT('Ctrl Pts',(1.07616373038996,-1.67960268239853,25.7916092478226));
#17319=CARTESIAN_POINT('Ctrl Pts',(1.17691520531392,-1.61412700138943,25.7993651544078));
#17320=CARTESIAN_POINT('Ctrl Pts',(1.26198662125724,-1.54852131668962,25.8065632728672));
#17321=CARTESIAN_POINT('Ctrl Pts',(1.43220889047856,-1.39386904468949,25.822391630411));
#17322=CARTESIAN_POINT('Ctrl Pts',(1.51523941591109,-1.30312734898599,25.8310487804382));
#17323=CARTESIAN_POINT('Ctrl Pts',(1.61745508094546,-1.16834154709674,25.84270063217));
#17324=CARTESIAN_POINT('Ctrl Pts',(1.64421010318575,-1.13037899443386,25.8458633273837));
#17325=CARTESIAN_POINT('Ctrl Pts',(1.68256145873976,-1.07171547255883,25.8505375077663));
#17326=CARTESIAN_POINT('Ctrl Pts',(1.69515278252784,-1.05168639965404,25.8520975212853));
#17327=CARTESIAN_POINT('Ctrl Pts',(1.71019257122284,-1.02679034037971,25.8539885365143));
#17328=CARTESIAN_POINT('Ctrl Pts',(1.71298070295101,-1.02213215718674,25.8543403180291));
#17329=CARTESIAN_POINT('Ctrl Pts',(1.71733039127652,-1.01479726636076,25.85489097836));
#17330=CARTESIAN_POINT('Ctrl Pts',(1.71890476065637,-1.012128247175,25.8550906773256));
#17331=CARTESIAN_POINT('Ctrl Pts',(1.72183703087128,-1.0071306110716,25.8554633292266));
#17332=CARTESIAN_POINT('Ctrl Pts',(1.72319641603441,-1.00480293616457,25.8556363759171));
#17333=CARTESIAN_POINT('Ctrl Pts',(1.72627443342344,-0.999507829862,25.8560288634599));
#17334=CARTESIAN_POINT('Ctrl Pts',(1.72799013065602,-0.996538724903854,
25.8562481128267));
#17335=CARTESIAN_POINT('Ctrl Pts',(1.73306863173539,-0.987697559558204,
25.8568985610925));
#17336=CARTESIAN_POINT('Ctrl Pts',(1.73640926436061,-0.981812722097654,
25.8573283529338));
#17337=CARTESIAN_POINT('Ctrl Pts',(1.76042407689899,-0.93900241183533,25.8604329558507));
#17338=CARTESIAN_POINT('Ctrl Pts',(1.77995024042742,-0.901441188220266,
25.8630386940851));
#17339=CARTESIAN_POINT('Ctrl Pts',(1.83288686438338,-0.791171291581292,
25.8704346156787));
#17340=CARTESIAN_POINT('Ctrl Pts',(1.86313925828265,-0.717035772964954,
25.8750999933681));
#17341=CARTESIAN_POINT('Ctrl Pts',(1.92122907527788,-0.545934711010538,
25.8855921925858));
#17342=CARTESIAN_POINT('Ctrl Pts',(1.94633272388889,-0.44827856855005,25.8913968898663));
#17343=CARTESIAN_POINT('Ctrl Pts',(1.97291971163532,-0.298727448959983,
25.9004243087824));
#17344=CARTESIAN_POINT('Ctrl Pts',(1.97993798019173,-0.247982396716648,
25.9035090895083));
#17345=CARTESIAN_POINT('Ctrl Pts',(1.98801726507701,-0.166585385870296,
25.9085297281418));
#17346=CARTESIAN_POINT('Ctrl Pts',(1.9903379835977,-0.136080451487063,25.9104272749125));
#17347=CARTESIAN_POINT('Ctrl Pts',(1.99241668309104,-0.0968454992855836,
25.9128929712981));
#17348=CARTESIAN_POINT('Ctrl Pts',(1.99282020784631,-0.0881527374766316,
25.9134408351324));
#17349=CARTESIAN_POINT('Ctrl Pts',(1.99337933952493,-0.0741271314738322,
25.9143274451045));
#17350=CARTESIAN_POINT('Ctrl Pts',(1.99357045687673,-0.068795751551865,
25.914665076476));
#17351=CARTESIAN_POINT('Ctrl Pts',(1.99389425951927,-0.0586233501982341,
25.915310485207));
#17352=CARTESIAN_POINT('Ctrl Pts',(1.9940307067648,-0.0537824797845978,
25.9156181423365));
#17353=CARTESIAN_POINT('Ctrl Pts',(1.99430238156014,-0.0427128653186683,
25.9163228682519));
#17354=CARTESIAN_POINT('Ctrl Pts',(1.99442605794871,-0.0364839126123607,
25.9167202960553));
#17355=CARTESIAN_POINT('Ctrl Pts',(1.99471664821841,-0.017326845509537,
25.9179453228491));
#17356=CARTESIAN_POINT('Ctrl Pts',(1.99478704939554,-0.00439780997735998,
25.9187759319005));
#17357=CARTESIAN_POINT('Ctrl Pts',(1.99426185797431,0.118406896693262,25.9267031633904));
#17358=CARTESIAN_POINT('Ctrl Pts',(1.98471466589682,0.228037020273399,25.9340835522411));
#17359=CARTESIAN_POINT('Ctrl Pts',(1.96453818861248,0.345996943436812,25.9423284372156));
#17360=CARTESIAN_POINT('Ctrl Pts',(1.96280940949652,0.355673161983693,25.9430068938583));
#17361=CARTESIAN_POINT('Ctrl Pts',(1.9401839880797,0.477119293833564,25.9515478353791));
#17362=CARTESIAN_POINT('Ctrl Pts',(1.9098397745849,0.58691415201389,25.9595589842457));
#17363=CARTESIAN_POINT('Ctrl Pts',(1.85503359399821,0.734716242874107,25.9703987642592));
#17364=CARTESIAN_POINT('Ctrl Pts',(1.83840174070168,0.775394853529512,25.9733862077173));
#17365=CARTESIAN_POINT('Ctrl Pts',(1.81112455695698,0.836286126899067,25.9778317768523));
#17366=CARTESIAN_POINT('Ctrl Pts',(1.80145418941835,0.856918642892758,25.9793333478071));
#17367=CARTESIAN_POINT('Ctrl Pts',(1.78907260376595,0.882199270848949,25.9811632221525));
#17368=CARTESIAN_POINT('Ctrl Pts',(1.78669381593469,0.887007071420386,25.9815107709976));
#17369=CARTESIAN_POINT('Ctrl Pts',(1.78291666128578,0.89456428222356,25.9820562892128));
#17370=CARTESIAN_POINT('Ctrl Pts',(1.78153128347637,0.897320100316879,25.9822550539083));
#17371=CARTESIAN_POINT('Ctrl Pts',(1.778922287721,0.9024801016507,25.9826268973211));
#17372=CARTESIAN_POINT('Ctrl Pts',(1.77770019892014,0.904884988547796,25.9828000655256));
#17373=CARTESIAN_POINT('Ctrl Pts',(1.77490369323756,0.910360560287811,25.9831940459864));
#17374=CARTESIAN_POINT('Ctrl Pts',(1.77332618787937,0.913429637036049,25.9834146609613));
#17375=CARTESIAN_POINT('Ctrl Pts',(1.76847676335533,0.922804403181734,25.9840879456939));
#17376=CARTESIAN_POINT('Ctrl Pts',(1.76517907215287,0.929096806555903,25.9845390218287));
#17377=CARTESIAN_POINT('Ctrl Pts',(1.73899800009601,0.978410966779382,25.9880686154783));
#17378=CARTESIAN_POINT('Ctrl Pts',(1.71457658295664,1.02060281694847,25.9910553215393));
#17379=CARTESIAN_POINT('Ctrl Pts',(1.68054852643241,1.07471614644264,25.9948982501646));
#17380=CARTESIAN_POINT('Ctrl Pts',(1.67231846800554,1.08747832402456,25.9958054947261));
#17381=CARTESIAN_POINT('Ctrl Pts',(1.63288112388631,1.14712634662467,26.0000561249536));
#17382=CARTESIAN_POINT('Ctrl Pts',(1.59984178874383,1.19277256806037,26.0033399375662));
#17383=CARTESIAN_POINT('Ctrl Pts',(1.50212077393058,1.31640214040468,26.0124927508386));
#17384=CARTESIAN_POINT('Ctrl Pts',(1.43337099195527,1.39094498415361,26.0183274019524));
#17385=CARTESIAN_POINT('Ctrl Pts',(1.32125231619151,1.49533174266239,26.0274264166253));
#17386=CARTESIAN_POINT('Ctrl Pts',(1.28187717936533,1.52922038162306,26.0305530306983));
#17387=CARTESIAN_POINT('Ctrl Pts',(1.21703578395128,1.58076134278926,26.035635770227));
#17388=CARTESIAN_POINT('Ctrl Pts',(1.19240225858182,1.59942465043815,26.0375523515315));
#17389=CARTESIAN_POINT('Ctrl Pts',(1.16026458267995,1.62261823278915,26.0400394609623));
#17390=CARTESIAN_POINT('Ctrl Pts',(1.15314959502155,1.62768235193344,26.0405892611953));
#17391=CARTESIAN_POINT('Ctrl Pts',(1.14162946884152,1.63576839819618,26.041478249417));
#17392=CARTESIAN_POINT('Ctrl Pts',(1.13724499083379,1.63881967482166,26.0418163116435));
#17393=CARTESIAN_POINT('Ctrl Pts',(1.12886364557716,1.64460264776726,26.0424620430906));
#17394=CARTESIAN_POINT('Ctrl Pts',(1.12486898045824,1.64733748074666,26.0427695899667));
#17395=CARTESIAN_POINT('Ctrl Pts',(1.11572171645459,1.65355110750593,26.0434733581944));
#17396=CARTESIAN_POINT('Ctrl Pts',(1.11056275012345,1.65702039525595,26.0438699350786));
#17397=CARTESIAN_POINT('Ctrl Pts',(1.09468126240914,1.66759285302972,26.0450897791169));
#17398=CARTESIAN_POINT('Ctrl Pts',(1.08390635783943,1.67461636929122,26.0459160194851));
#17399=CARTESIAN_POINT('Ctrl Pts',(0.952689205382368,1.75835204048236,26.0559631584849));
#17400=CARTESIAN_POINT('Ctrl Pts',(0.82443882223363,1.82200541545647,26.0656788882564));
#17401=CARTESIAN_POINT('Ctrl Pts',(0.596849724799946,1.90598189114176,26.0825533825283));
#17402=CARTESIAN_POINT('Ctrl Pts',(0.500713760629589,1.93346404181297,26.0895671071567));
#17403=CARTESIAN_POINT('Ctrl Pts',(0.366140608924806,1.96121877204345,26.0989693445146));
#17404=CARTESIAN_POINT('Ctrl Pts',(0.329149317566016,1.96776500465066,26.1015106883999));
#17405=CARTESIAN_POINT('Ctrl Pts',(0.271772924509367,1.97625525746801,26.1053651905389));
#17406=CARTESIAN_POINT('Ctrl Pts',(0.251507089699256,1.97893648955981,26.1067099342092));
#17407=CARTESIAN_POINT('Ctrl Pts',(0.226061599615823,1.98190577631284,26.1083745302139));
#17408=CARTESIAN_POINT('Ctrl Pts',(0.220918144399159,1.98248569425699,26.108709787391));
#17409=CARTESIAN_POINT('Ctrl Pts',(0.21274761949423,1.98337471765808,26.1092403575557));
#17410=CARTESIAN_POINT('Ctrl Pts',(0.209722044188232,1.98369692360802,26.1094363955803));
#17411=CARTESIAN_POINT('Ctrl Pts',(0.204005154906916,1.9842925129566,26.1098059787241));
#17412=CARTESIAN_POINT('Ctrl Pts',(0.201314055002673,1.98456734114928,26.109979600685));
#17413=CARTESIAN_POINT('Ctrl Pts',(0.195178431731702,1.98518133218912,26.1103746633527));
#17414=CARTESIAN_POINT('Ctrl Pts',(0.191733584684177,1.98551700441769,26.110595905561));
#17415=CARTESIAN_POINT('Ctrl Pts',(0.182635416155084,1.98637964762467,26.1111787749106));
#17416=CARTESIAN_POINT('Ctrl Pts',(0.176980637970635,1.98689145536221,26.1115395655058));
#17417=CARTESIAN_POINT('Ctrl Pts',(0.139604520138677,1.99011349467939,26.113914948589));
#17418=CARTESIAN_POINT('Ctrl Pts',(0.107822258080884,1.99208829679993,26.1158905150858));
#17419=CARTESIAN_POINT('Ctrl Pts',(-0.122430932623135,2.00086780924987,
26.1299705230797));
#17420=CARTESIAN_POINT('Ctrl Pts',(-0.320901624951784,1.97876321495778,
26.1409631319081));
#17421=CARTESIAN_POINT('Ctrl Pts',(-0.558400312333835,1.91557767715059,
26.1556192864236));
#17422=CARTESIAN_POINT('Ctrl Pts',(-0.603498923023268,1.90185102235544,
26.1584666489346));
#17423=CARTESIAN_POINT('Ctrl Pts',(-0.666069549896328,1.88035668408686,
26.1625336791399));
#17424=CARTESIAN_POINT('Ctrl Pts',(-0.683982295194189,1.87391517593918,
26.1637116263799));
#17425=CARTESIAN_POINT('Ctrl Pts',(-0.715204798918712,1.86218010435634,
26.1657904182511));
#17426=CARTESIAN_POINT('Ctrl Pts',(-0.728555009176556,1.85699763787855,
26.1666875815025));
#17427=CARTESIAN_POINT('Ctrl Pts',(-0.747876741195922,1.84925664043125,
26.167998631637));
#17428=CARTESIAN_POINT('Ctrl Pts',(-0.753893601325338,1.84681189579846,
26.1684086857675));
#17429=CARTESIAN_POINT('Ctrl Pts',(-0.764410984831291,1.84247855604525,
26.169128638015));
#17430=CARTESIAN_POINT('Ctrl Pts',(-0.768916739464059,1.8406027355994,26.1694381014841));
#17431=CARTESIAN_POINT('Ctrl Pts',(-0.777641267934519,1.83693294301787,
26.1700393354339));
#17432=CARTESIAN_POINT('Ctrl Pts',(-0.781860834535907,1.83514092471938,
26.1703310379046));
#17433=CARTESIAN_POINT('Ctrl Pts',(-0.793061823184645,1.83033830509514,
26.1711078404132));
#17434=CARTESIAN_POINT('Ctrl Pts',(-0.800032221187363,1.82730233100656,
26.1715938036627));
#17435=CARTESIAN_POINT('Ctrl Pts',(-0.824909929847585,1.81629715331854,
26.173337519136));
#17436=CARTESIAN_POINT('Ctrl Pts',(-0.842716443699149,1.80810417051011,
26.1746029143048));
#17437=CARTESIAN_POINT('Ctrl Pts',(-0.95314596916628,1.75530867440647,26.1825618115649));
#17438=CARTESIAN_POINT('Ctrl Pts',(-1.04231188331705,1.70387083882086,26.1894943428646));
#17439=CARTESIAN_POINT('Ctrl Pts',(-1.26080109961505,1.55424111626821,26.2077592632226));
#17440=CARTESIAN_POINT('Ctrl Pts',(-1.38283847185585,1.44673541264575,26.2192909718127));
#17441=CARTESIAN_POINT('Ctrl Pts',(-1.50717392643413,1.30693600594174,26.2317864893768));
#17442=CARTESIAN_POINT('Ctrl Pts',(-1.52346710663281,1.28790647476713,26.2334400607132));
#17443=CARTESIAN_POINT('Ctrl Pts',(-1.54291335661809,1.26430869817792,26.2354284872711));
#17444=CARTESIAN_POINT('Ctrl Pts',(-1.54641060120708,1.26002871576761,26.2357866940909));
#17445=CARTESIAN_POINT('Ctrl Pts',(-1.5518543993518,1.25330970731822,26.2363451543882));
#17446=CARTESIAN_POINT('Ctrl Pts',(-1.55381306204281,1.25088059693913,26.2365462663092));
#17447=CARTESIAN_POINT('Ctrl Pts',(-1.55745146445279,1.24634656111072,26.2369201702297));
#17448=CARTESIAN_POINT('Ctrl Pts',(-1.55913262412154,1.24424285212039,26.2370930623844));
#17449=CARTESIAN_POINT('Ctrl Pts',(-1.56292557622647,1.23947680614966,26.2374834264998));
#17450=CARTESIAN_POINT('Ctrl Pts',(-1.56503482321811,1.23681248066952,26.2377007153082));
#17451=CARTESIAN_POINT('Ctrl Pts',(-1.571234413546,1.22894012633011,26.2383400411756));
#17452=CARTESIAN_POINT('Ctrl Pts',(-1.57530569270704,1.22371703997052,26.2387607415737));
#17453=CARTESIAN_POINT('Ctrl Pts',(-1.60317302015194,1.18759620235874,26.2416470540721));
#17454=CARTESIAN_POINT('Ctrl Pts',(-1.62608639224044,1.15602422432862,26.2440541342699));
#17455=CARTESIAN_POINT('Ctrl Pts',(-1.74443309118259,0.982467638912514,
26.2567960451355));
#17456=CARTESIAN_POINT('Ctrl Pts',(-1.822233538656,0.829316865170294,26.2663805023754));
#17457=CARTESIAN_POINT('Ctrl Pts',(-1.89967946163673,0.6114421817386,26.2800308128428));
#17458=CARTESIAN_POINT('Ctrl Pts',(-1.91724614571517,0.553904242374328,
26.2836302757754));
#17459=CARTESIAN_POINT('Ctrl Pts',(-1.94071476147354,0.46241941585726,26.2894095603495));
#17460=CARTESIAN_POINT('Ctrl Pts',(-1.94838317109513,0.428961884230149,
26.2915343620131));
#17461=CARTESIAN_POINT('Ctrl Pts',(-1.95697879364363,0.386449925805058,
26.2942548760653));
#17462=CARTESIAN_POINT('Ctrl Pts',(-1.95871273972537,0.377563164004095,
26.29482469995));
#17463=CARTESIAN_POINT('Ctrl Pts',(-1.96138656100846,0.363345047903939,
26.2957382855517));
#17464=CARTESIAN_POINT('Ctrl Pts',(-1.9623653533818,0.358021067041667,26.2960808052573));
#17465=CARTESIAN_POINT('Ctrl Pts',(-1.9641758859554,0.3479424515438,26.2967300502989));
#17466=CARTESIAN_POINT('Ctrl Pts',(-1.96501206449619,0.343188645305611,
26.2970366319125));
#17467=CARTESIAN_POINT('Ctrl Pts',(-1.96686437449493,0.332429232462508,
26.297731339858));
#17468=CARTESIAN_POINT('Ctrl Pts',(-1.96787026552719,0.326421933924422,
26.2981197885187));
#17469=CARTESIAN_POINT('Ctrl Pts',(-1.97038262530088,0.310984047049956,
26.2991195593547));
#17470=CARTESIAN_POINT('Ctrl Pts',(-1.97184889681389,0.301547161270824,
26.2997321491823));
#17471=CARTESIAN_POINT('Ctrl Pts',(-1.98023994509146,0.24486246526018,26.3034208341351));
#17472=CARTESIAN_POINT('Ctrl Pts',(-1.98553353090647,0.197392540164988,
26.3065480367885));
#17473=CARTESIAN_POINT('Ctrl Pts',(-1.99012763534971,0.136382250053488,
26.3106197701565));
#17474=CARTESIAN_POINT('Ctrl Pts',(-1.99100117429133,0.122973304434868,
26.3115178568455));
#17475=CARTESIAN_POINT('Ctrl Pts',(-1.99377655691672,0.0725169374495927,
26.314909136307));
#17476=CARTESIAN_POINT('Ctrl Pts',(-1.99478023382093,0.0354292575438041,
26.3174261235079));
#17477=CARTESIAN_POINT('Ctrl Pts',(-1.99460412678541,-0.17578471832943,
26.3318843840123));
#17478=CARTESIAN_POINT('Ctrl Pts',(-1.97166284332363,-0.349123068784183,
26.3443142834677));
#17479=CARTESIAN_POINT('Ctrl Pts',(-1.918691056218,-0.546408367989368,26.3580335800415));
#17480=CARTESIAN_POINT('Ctrl Pts',(-1.91020842683993,-0.575362045656703,
26.3600333459574));
#17481=CARTESIAN_POINT('Ctrl Pts',(-1.89938054039609,-0.60943605859832,
26.3623615716245));
#17482=CARTESIAN_POINT('Ctrl Pts',(-1.89766696246977,-0.614751045636675,
26.3627240019386));
#17483=CARTESIAN_POINT('Ctrl Pts',(-1.89485235788306,-0.623357158307403,
26.3633095824338));
#17484=CARTESIAN_POINT('Ctrl Pts',(-1.89376503799945,-0.626652683938401,
26.3635335144055));
#17485=CARTESIAN_POINT('Ctrl Pts',(-1.89181658524206,-0.632506804685954,
26.3639307425749));
#17486=CARTESIAN_POINT('Ctrl Pts',(-1.89095885507573,-0.635066499592859,
26.36410423715));
#17487=CARTESIAN_POINT('Ctrl Pts',(-1.88911394872385,-0.640535313916996,
26.3644744943596));
#17488=CARTESIAN_POINT('Ctrl Pts',(-1.88812525126198,-0.643443886828484,
26.3646711651092));
#17489=CARTESIAN_POINT('Ctrl Pts',(-1.8854099220658,-0.651371754444841,
26.3652065773537));
#17490=CARTESIAN_POINT('Ctrl Pts',(-1.88366995363748,-0.65638650506382,
26.3655445376205));
#17491=CARTESIAN_POINT('Ctrl Pts',(-1.87459671124977,-0.682203214941757,
26.3672810178602));
#17492=CARTESIAN_POINT('Ctrl Pts',(-1.86693845244365,-0.70289043921845,
26.3686611066377));
#17493=CARTESIAN_POINT('Ctrl Pts',(-1.84374070659885,-0.76249833401675,
26.3726162181632));
#17494=CARTESIAN_POINT('Ctrl Pts',(-1.82731534158822,-0.801063436021313,
26.3751482999223));
#17495=CARTESIAN_POINT('Ctrl Pts',(-1.75471198944255,-0.957649823863518,
26.3854292521458));
#17496=CARTESIAN_POINT('Ctrl Pts',(-1.68821691862545,-1.07053009148921,
26.3928596036727));
#17497=CARTESIAN_POINT('Ctrl Pts',(-1.54882912941497,-1.26147932492719,
26.4067117767347));
#17498=CARTESIAN_POINT('Ctrl Pts',(-1.47982477256909,-1.34175843473198,
26.4130296890303));
#17499=CARTESIAN_POINT('Ctrl Pts',(-1.39566419424561,-1.42524184998158,
26.4204298009215));
#17500=CARTESIAN_POINT('Ctrl Pts',(-1.38644886770617,-1.43420793434731,
26.4212361936577));
#17501=CARTESIAN_POINT('Ctrl Pts',(-1.37265067476396,-1.44737566920481,
26.4224382240405));
#17502=CARTESIAN_POINT('Ctrl Pts',(-1.36813367926805,-1.45164611285514,
26.4228308805203));
#17503=CARTESIAN_POINT('Ctrl Pts',(-1.36006353019259,-1.45920464367752,
26.4235309574526));
#17504=CARTESIAN_POINT('Ctrl Pts',(-1.35651821282052,-1.46250105500789,
26.4238380175285));
#17505=CARTESIAN_POINT('Ctrl Pts',(-1.34903539215994,-1.46940791216685,
26.4244850932653));
#17506=CARTESIAN_POINT('Ctrl Pts',(-1.34509531973702,-1.47301550621327,
26.4248252267161));
#17507=CARTESIAN_POINT('Ctrl Pts',(-1.33467456585134,-1.48248024304729,
26.4257233157824));
#17508=CARTESIAN_POINT('Ctrl Pts',(-1.32816987583134,-1.48831066806087,
26.4262823914972));
#17509=CARTESIAN_POINT('Ctrl Pts',(-1.29846490397567,-1.51458665235052,
26.4288288937035));
#17510=CARTESIAN_POINT('Ctrl Pts',(-1.27483047793644,-1.53453279805448,
26.4308368911397));
#17511=CARTESIAN_POINT('Ctrl Pts',(-1.21024745778367,-1.58651535148252,
26.4362798463231));
#17512=CARTESIAN_POINT('Ctrl Pts',(-1.16849646028572,-1.6175120113899,26.4397535099787));
#17513=CARTESIAN_POINT('Ctrl Pts',(-1.04191462758986,-1.70402837929633,
26.4501511971157));
#17514=CARTESIAN_POINT('Ctrl Pts',(-0.954013597706767,-1.75475170945212,
26.4572118767671));
#17515=CARTESIAN_POINT('Ctrl Pts',(-0.855502264728771,-1.80200062440219,
26.46483432746));
#17516=CARTESIAN_POINT('Ctrl Pts',(-0.848335881024695,-1.8053854459854,
26.4653871833649));
#17517=CARTESIAN_POINT('Ctrl Pts',(-0.774193153054797,-1.83986555427451,
26.471089046765));
#17518=CARTESIAN_POINT('Ctrl Pts',(-0.705554993997839,-1.8672637295543,
26.4762195795999));
#17519=CARTESIAN_POINT('Ctrl Pts',(-0.598624248243548,-1.90320631581014,
26.4838547097468));
#17520=CARTESIAN_POINT('Ctrl Pts',(-0.561337915077519,-1.91453532581896,
26.4864526390203));
#17521=CARTESIAN_POINT('Ctrl Pts',(-0.517352955306116,-1.92650390802183,
26.4894240026949));
#17522=CARTESIAN_POINT('Ctrl Pts',(-0.510956410642753,-1.92821029387603,
26.489853829232));
#17523=CARTESIAN_POINT('Ctrl Pts',(-0.5012641960562,-1.93074423795946,26.4905015350181));
#17524=CARTESIAN_POINT('Ctrl Pts',(-0.49797479084882,-1.93159525127854,
26.4907207353879));
#17525=CARTESIAN_POINT('Ctrl Pts',(-0.492074417172123,-1.93310568313844,
26.4911127918006));
#17526=CARTESIAN_POINT('Ctrl Pts',(-0.489464284526345,-1.93376822000055,
26.4912858263069));
#17527=CARTESIAN_POINT('Ctrl Pts',(-0.483826434209728,-1.93518714415077,
26.4916587158718));
#17528=CARTESIAN_POINT('Ctrl Pts',(-0.480798291678137,-1.93594170996259,
26.4918584646121));
#17529=CARTESIAN_POINT('Ctrl Pts',(-0.472400757895147,-1.93801332581395,
26.4924109537523));
#17530=CARTESIAN_POINT('Ctrl Pts',(-0.467027591755882,-1.93931517742277,
26.4927628269616));
#17531=CARTESIAN_POINT('Ctrl Pts',(-0.437259334388041,-1.94639676250448,
26.4947035647494));
#17532=CARTESIAN_POINT('Ctrl Pts',(-0.412761062312387,-1.95173884780165,
26.496268439976));
#17533=CARTESIAN_POINT('Ctrl Pts',(-0.229162515185292,-1.98816238159269,
26.5078004067795));
#17534=CARTESIAN_POINT('Ctrl Pts',(-0.0668850640269317,-2.00021145098082,
26.516940738108));
#17535=CARTESIAN_POINT('Ctrl Pts',(0.207682379064669,-1.98710948842253,
26.5330064919151));
#17536=CARTESIAN_POINT('Ctrl Pts',(0.319611763620731,-1.97220155669412,
26.5397209213675));
#17537=CARTESIAN_POINT('Ctrl Pts',(0.442320410307593,-1.94513442475644,
26.5475643696767));
#17538=CARTESIAN_POINT('Ctrl Pts',(0.454939108758556,-1.94222183863556,
26.5483765391001));
#17539=CARTESIAN_POINT('Ctrl Pts',(0.473589023105039,-1.93772543641813,
26.5495855364325));
#17540=CARTESIAN_POINT('Ctrl Pts',(0.479642786246814,-1.93623583943572,
26.5499793320645));
#17541=CARTESIAN_POINT('Ctrl Pts',(0.490386988582767,-1.93353862693419,
26.5506806904484));
#17542=CARTESIAN_POINT('Ctrl Pts',(0.495080220679038,-1.93234225613173,
26.5509878879997));
#17543=CARTESIAN_POINT('Ctrl Pts',(0.504931603781281,-1.92979275451388,
26.5516344880191));
#17544=CARTESIAN_POINT('Ctrl Pts',(0.510088771878332,-1.92843600976659,
26.5519740053624));
#17545=CARTESIAN_POINT('Ctrl Pts',(0.523637879894014,-1.92481336552385,
26.5528687267591));
#17546=CARTESIAN_POINT('Ctrl Pts',(0.532020484927929,-1.92251328240117,
26.5534250357786));
#17547=CARTESIAN_POINT('Ctrl Pts',(0.569741253302596,-1.91189757626506,
26.5559410358045));
#17548=CARTESIAN_POINT('Ctrl Pts',(0.598900094825213,-1.90296503988263,
26.5579206992819));
#17549=CARTESIAN_POINT('Ctrl Pts',(0.676240318042172,-1.87731899727726,
26.5632683232878));
#17550=CARTESIAN_POINT('Ctrl Pts',(0.724002204467846,-1.85942132128623,
26.5666733430939));
#17551=CARTESIAN_POINT('Ctrl Pts',(0.863764592783322,-1.80084703445125,
26.5769417616456));
#17552=CARTESIAN_POINT('Ctrl Pts',(0.953427038871567,-1.75502503740542,
26.583942198752));
#17553=CARTESIAN_POINT('Ctrl Pts',(1.05674765737386,-1.69196111948414,26.5923876798864));
#17554=CARTESIAN_POINT('Ctrl Pts',(1.07408476183507,-1.68100861780158,26.5938180630293));
#17555=CARTESIAN_POINT('Ctrl Pts',(1.17559554214738,-1.61466878461484,26.602262744138));
#17556=CARTESIAN_POINT('Ctrl Pts',(1.25565493814225,-1.55322765029401,26.6092172160306));
#17557=CARTESIAN_POINT('Ctrl Pts',(1.33658106659261,-1.48075662463046,26.6163132050611));
#17558=CARTESIAN_POINT('Ctrl Pts',(1.34239545496186,-1.47548757243513,26.6168233947685));
#17559=CARTESIAN_POINT('Ctrl Pts',(1.35079894185163,-1.46778146197996,26.6175610909664));
#17560=CARTESIAN_POINT('Ctrl Pts',(1.35341276377315,-1.46537165687626,26.6177905900025));
#17561=CARTESIAN_POINT('Ctrl Pts',(1.35801356460308,-1.46110715162975,26.6181946086389));
#17562=CARTESIAN_POINT('Ctrl Pts',(1.36000321195562,-1.45925536285512,26.6183693481036));
#17563=CARTESIAN_POINT('Ctrl Pts',(1.36417487842115,-1.45535679946785,26.6187357539314));
#17564=CARTESIAN_POINT('Ctrl Pts',(1.36635607490487,-1.45330918580058,26.6189273535179));
#17565=CARTESIAN_POINT('Ctrl Pts',(1.37213224134577,-1.44786227021083,26.619434822615));
#17566=CARTESIAN_POINT('Ctrl Pts',(1.37571921384765,-1.4444544600488,26.6197500431793));
#17567=CARTESIAN_POINT('Ctrl Pts',(1.39224129355025,-1.42864025403441,26.6212025955013));
#17568=CARTESIAN_POINT('Ctrl Pts',(1.40502200223316,-1.41607274613837,26.622327942864));
#17569=CARTESIAN_POINT('Ctrl Pts',(1.439588913497,-1.38115364771536,26.6253823062752));
#17570=CARTESIAN_POINT('Ctrl Pts',(1.46102340915189,-1.3584595908769,26.6272883250738));
#17571=CARTESIAN_POINT('Ctrl Pts',(1.53445356755619,-1.27696491137922,26.6339011045656));
#17572=CARTESIAN_POINT('Ctrl Pts',(1.58350646538346,-1.21560525531993,26.6384738714332));
#17573=CARTESIAN_POINT('Ctrl Pts',(1.72203520137679,-1.01965555229839,26.6524043996169));
#17574=CARTESIAN_POINT('Ctrl Pts',(1.79888496597703,-0.876988223770606,
26.6617097844222));
#17575=CARTESIAN_POINT('Ctrl Pts',(1.86143030003341,-0.717084212650901,
26.6723348320138));
#17576=CARTESIAN_POINT('Ctrl Pts',(1.86508874791876,-0.707514301115196,
26.6729711537058));
#17577=CARTESIAN_POINT('Ctrl Pts',(1.87357378104815,-0.684795611325849,
26.6744831068838));
#17578=CARTESIAN_POINT('Ctrl Pts',(1.87833586643428,-0.671623480303962,
26.6753607865642));
#17579=CARTESIAN_POINT('Ctrl Pts',(1.88506019929044,-0.652392629358714,
26.6766441375281));
#17580=CARTESIAN_POINT('Ctrl Pts',(1.8871328469539,-0.646372736285141,26.6770461469071));
#17581=CARTESIAN_POINT('Ctrl Pts',(1.89074251763782,-0.635723280272227,
26.6777578526926));
#17582=CARTESIAN_POINT('Ctrl Pts',(1.89229145233172,-0.631097786261059,
26.6780671525897));
#17583=CARTESIAN_POINT('Ctrl Pts',(1.89546336637253,-0.62150901625406,26.6787087263598));
#17584=CARTESIAN_POINT('Ctrl Pts',(1.89708385196261,-0.616544960496398,
26.6790410796741));
#17585=CARTESIAN_POINT('Ctrl Pts',(1.90119672856272,-0.603776189745432,
26.6798965524599));
#17586=CARTESIAN_POINT('Ctrl Pts',(1.90366054134505,-0.59596243841925,26.6804206063504));
#17587=CARTESIAN_POINT('Ctrl Pts',(1.91370779322722,-0.56340041594603,26.6826069442676));
#17588=CARTESIAN_POINT('Ctrl Pts',(1.92085701684684,-0.538521830995022,
26.6842833321697));
#17589=CARTESIAN_POINT('Ctrl Pts',(1.97447475946923,-0.337262192228768,
26.6978991188951));
#17590=CARTESIAN_POINT('Ctrl Pts',(1.99702493684115,-0.155434445352629,
26.7106518453713));
#17591=CARTESIAN_POINT('Ctrl Pts',(1.99370248397765,0.0911933319285907,
26.7278134125995));
#17592=CARTESIAN_POINT('Ctrl Pts',(1.98972480144048,0.15544192155548,26.7322585120981));
#17593=CARTESIAN_POINT('Ctrl Pts',(1.97889508195542,0.25331119533604,26.7388956553218));
#17594=CARTESIAN_POINT('Ctrl Pts',(1.97427130654853,0.287133174424992,26.7411642950898));
#17595=CARTESIAN_POINT('Ctrl Pts',(1.96784858906812,0.326547301282571,26.7437660239765));
#17596=CARTESIAN_POINT('Ctrl Pts',(1.96689067741463,0.332268377355896,26.7441426296243));
#17597=CARTESIAN_POINT('Ctrl Pts',(1.96531520264734,0.341432202951507,26.7447441025668));
#17598=CARTESIAN_POINT('Ctrl Pts',(1.96471352616173,0.344877595016709,26.7449698431203));
#17599=CARTESIAN_POINT('Ctrl Pts',(1.96362960052148,0.350989597476334,26.7453695674785));
#17600=CARTESIAN_POINT('Ctrl Pts',(1.96315097625513,0.353656825692593,26.7455437557285));
#17601=CARTESIAN_POINT('Ctrl Pts',(1.96212710995711,0.359296393844331,26.7459115262723));
#17602=CARTESIAN_POINT('Ctrl Pts',(1.96158055004727,0.362268464308082,26.7461050321147));
#17603=CARTESIAN_POINT('Ctrl Pts',(1.96009657599152,0.370236154242418,26.7466229882504));
#17604=CARTESIAN_POINT('Ctrl Pts',(1.95914681059267,0.375229493822779,26.7469467411475));
#17605=CARTESIAN_POINT('Ctrl Pts',(1.95448527410917,0.399237007486242,26.7484994632784));
#17606=CARTESIAN_POINT('Ctrl Pts',(1.95051556888445,0.418200858702199,26.7497143418867));
#17607=CARTESIAN_POINT('Ctrl Pts',(1.93864354439568,0.471062712964736,26.7530758453256));
#17608=CARTESIAN_POINT('Ctrl Pts',(1.93012914789979,0.504817435055281,26.7551934359065));
#17609=CARTESIAN_POINT('Ctrl Pts',(1.89564977476314,0.627837238823449,26.7628617639749));
#17610=CARTESIAN_POINT('Ctrl Pts',(1.8643371691419,0.715483693555913,26.7682327513939));
#17611=CARTESIAN_POINT('Ctrl Pts',(1.76518250623002,0.941752498827515,26.7825611851712));
#17612=CARTESIAN_POINT('Ctrl Pts',(1.68721054741629,1.07521087950721,26.7915459232161));
#17613=CARTESIAN_POINT('Ctrl Pts',(1.58708477675972,1.2084488925758,26.801952976811));
#17614=CARTESIAN_POINT('Ctrl Pts',(1.57940809276774,1.21846496848483,26.8027446031987));
#17615=CARTESIAN_POINT('Ctrl Pts',(1.56783790872435,1.23326798121766,26.8039288066492));
#17616=CARTESIAN_POINT('Ctrl Pts',(1.56401629744102,1.23811091646886,26.8043185312953));
#17617=CARTESIAN_POINT('Ctrl Pts',(1.55715935714487,1.24671796333868,26.8050153253286));
#17618=CARTESIAN_POINT('Ctrl Pts',(1.55413267812496,1.25048892908516,26.8053220467383));
#17619=CARTESIAN_POINT('Ctrl Pts',(1.54771729480738,1.25842264344559,26.8059704204983));
#17620=CARTESIAN_POINT('Ctrl Pts',(1.54432544439457,1.26258278740416,26.8063121983354));
#17621=CARTESIAN_POINT('Ctrl Pts',(1.53529710376685,1.27356534220925,26.8072192754075));
#17622=CARTESIAN_POINT('Ctrl Pts',(1.52963198258032,1.28036396051745,26.8077857355272));
#17623=CARTESIAN_POINT('Ctrl Pts',(1.50320909495184,1.31164796964203,26.8104155483966));
#17624=CARTESIAN_POINT('Ctrl Pts',(1.48190844501357,1.3356665528501,26.8125011550772));
#17625=CARTESIAN_POINT('Ctrl Pts',(1.42273690421611,1.39922989617158,26.8182081552235));
#17626=CARTESIAN_POINT('Ctrl Pts',(1.38380462716622,1.43774422154937,26.8218730297614));
#17627=CARTESIAN_POINT('Ctrl Pts',(1.26682262299384,1.54431280508697,26.8326281361314));
#17628=CARTESIAN_POINT('Ctrl Pts',(1.18500034915161,1.60795289803314,26.8398535337512));
#17629=CARTESIAN_POINT('Ctrl Pts',(1.00442903832286,1.7271028278075,26.8549414240114));
#17630=CARTESIAN_POINT('Ctrl Pts',(0.905123122068543,1.7811570744217,26.8627753378795));
#17631=CARTESIAN_POINT('Ctrl Pts',(0.795389644129964,1.82932539034632,26.8706017864889));
#17632=CARTESIAN_POINT('Ctrl Pts',(0.788997555393894,1.83209140896231,26.8710547836139));
#17633=CARTESIAN_POINT('Ctrl Pts',(0.779384327556876,1.83619165280441,26.8717315708446));
#17634=CARTESIAN_POINT('Ctrl Pts',(0.776174047680886,1.8375509690965,26.8719568324296));
#17635=CARTESIAN_POINT('Ctrl Pts',(0.770620563290229,1.83988530917972,26.8723452029793));
#17636=CARTESIAN_POINT('Ctrl Pts',(0.768279044638956,1.84086428430984,26.8725085502532));
#17637=CARTESIAN_POINT('Ctrl Pts',(0.763436227959547,1.84287818799214,26.8728455522712));
#17638=CARTESIAN_POINT('Ctrl Pts',(0.760934688422781,1.84391249521189,26.8730191668976));
#17639=CARTESIAN_POINT('Ctrl Pts',(0.754933708331309,1.84637941844366,26.8734345627591));
#17640=CARTESIAN_POINT('Ctrl Pts',(0.75143226087567,1.84780719197532,26.8736760505919));
#17641=CARTESIAN_POINT('Ctrl Pts',(0.743956420899055,1.85083082651158,26.8741897982653));
#17642=CARTESIAN_POINT('Ctrl Pts',(0.739980897419763,1.85242386532358,26.8744618913414));
#17643=CARTESIAN_POINT('Ctrl Pts',(0.729040933464063,1.85676679853037,26.8752076822775));
#17644=CARTESIAN_POINT('Ctrl Pts',(0.722066009535537,1.85949033574795,26.8756798806225));
#17645=CARTESIAN_POINT('Ctrl Pts',(0.660729874755481,1.88304343617787,26.8798048770609));
#17646=CARTESIAN_POINT('Ctrl Pts',(0.605490722030305,1.90152541885122,26.8833316051077));
#17647=CARTESIAN_POINT('Ctrl Pts',(0.439327508296859,1.94914281083134,26.8936068513424));
#17648=CARTESIAN_POINT('Ctrl Pts',(0.326616864578987,1.97116472661776,26.9001575546848));
#17649=CARTESIAN_POINT('Ctrl Pts',(0.0946988516750447,1.99602812463555,
26.9137649673544));
#17650=CARTESIAN_POINT('Ctrl Pts',(-0.0241112902371501,1.99812630916227,
26.9208089214977));
#17651=CARTESIAN_POINT('Ctrl Pts',(-0.155358036647482,1.98873335596743,
26.9290217024561));
#17652=CARTESIAN_POINT('Ctrl Pts',(-0.168312104225953,1.98767892365156,
26.9298367542556));
#17653=CARTESIAN_POINT('Ctrl Pts',(-0.187472306828389,1.98593068285675,
26.9310492263832));
#17654=CARTESIAN_POINT('Ctrl Pts',(-0.1936871543292,1.98533418540749,26.9314435887757));
#17655=CARTESIAN_POINT('Ctrl Pts',(-0.204719147762053,1.98422304747911,
26.9321455858987));
#17656=CARTESIAN_POINT('Ctrl Pts',(-0.209537433549834,1.98372001423352,
26.9324528530268));
#17657=CARTESIAN_POINT('Ctrl Pts',(-0.219650951059132,1.98262689625758,
26.9330992221074));
#17658=CARTESIAN_POINT('Ctrl Pts',(-0.224945739569568,1.98203313882651,
26.9334384374999));
#17659=CARTESIAN_POINT('Ctrl Pts',(-0.238851556323302,1.98041730221149,
26.934331508299));
#17660=CARTESIAN_POINT('Ctrl Pts',(-0.24745833586246,1.97936028174012,26.9348864612837));
#17661=CARTESIAN_POINT('Ctrl Pts',(-0.286092619304876,1.97435958660014,
26.9373876491137));
#17662=CARTESIAN_POINT('Ctrl Pts',(-0.316033502074888,1.96978867440507,
26.9393535692194));
#17663=CARTESIAN_POINT('Ctrl Pts',(-0.395603831471121,1.95578029875629,
26.9446551557187));
#17664=CARTESIAN_POINT('Ctrl Pts',(-0.444995765098567,1.94513675971318,
26.9480271007642));
#17665=CARTESIAN_POINT('Ctrl Pts',(-0.597703835169315,1.90610878474122,
26.9587030040645));
#17666=CARTESIAN_POINT('Ctrl Pts',(-0.699167089008799,1.87127284054934,
26.966171819159));
#17667=CARTESIAN_POINT('Ctrl Pts',(-0.903395741189436,1.78221546839838,
26.9817134233405));
#17668=CARTESIAN_POINT('Ctrl Pts',(-1.00524668134954,1.72681838756154,26.9897567143344));
#17669=CARTESIAN_POINT('Ctrl Pts',(-1.10814050981651,1.65864743691404,26.9978169065957));
#17670=CARTESIAN_POINT('Ctrl Pts',(-1.11452726749546,1.65436262172344,26.9983168735835));
#17671=CARTESIAN_POINT('Ctrl Pts',(-1.12380604525255,1.64805945559564,26.9990425487904));
#17672=CARTESIAN_POINT('Ctrl Pts',(-1.12671765027172,1.64607026993382,26.9992701607283));
#17673=CARTESIAN_POINT('Ctrl Pts',(-1.13179884374909,1.64257904002938,26.9996671829498));
#17674=CARTESIAN_POINT('Ctrl Pts',(-1.1339707440804,1.64108039941883,26.9998368225525));
#17675=CARTESIAN_POINT('Ctrl Pts',(-1.13614693334299,1.63957241634298,27.0000067302211));
#17676=CARTESIAN_POINT('Ctrl Pts',(-1.13615416727734,1.63956740354172,27.0000072950154));
#17677=CARTESIAN_POINT('Ctrl Pts',(-1.13616860543781,1.63955739838358,27.0000084222831));
#17678=CARTESIAN_POINT('Ctrl Pts',(-1.13617579222358,1.63955241811355,27.0000089833948));
#17679=CARTESIAN_POINT('Ctrl Pts',(-1.13619011434815,1.63954249308558,27.0000101016001));
#17680=CARTESIAN_POINT('Ctrl Pts',(-1.13619724899851,1.63953754880576,27.00001065864));
#17681=CARTESIAN_POINT('Ctrl Pts',(-1.13621146735668,1.63952769541166,27.0000117687408));
#17682=CARTESIAN_POINT('Ctrl Pts',(-1.13621855040836,1.6395227867531,27.0000123217507));
#17683=CARTESIAN_POINT('Ctrl Pts',(-1.13623266624489,1.63951300413619,27.0000134238444));
#17684=CARTESIAN_POINT('Ctrl Pts',(-1.13623969828764,1.63950813069313,27.0000139728704));
#17685=CARTESIAN_POINT('Ctrl Pts',(-1.13625371274421,1.63949841806804,27.0000150670461));
#17686=CARTESIAN_POINT('Ctrl Pts',(-1.13626069439538,1.63949357941554,27.0000156121364));
#17687=CARTESIAN_POINT('Ctrl Pts',(-1.13627460833467,1.63948393619013,27.0000166984616));
#17688=CARTESIAN_POINT('Ctrl Pts',(-1.13628154001269,1.63947913204103,27.0000172396489));
#17689=CARTESIAN_POINT('Ctrl Pts',(-1.13629535488644,1.6394695572148,27.000018318237));
#17690=CARTESIAN_POINT('Ctrl Pts',(-1.13630223722509,1.63946478713265,27.0000188555709));
#17691=CARTESIAN_POINT('Ctrl Pts',(-1.1363159539005,1.63945528011008,27.0000199264895));
#17692=CARTESIAN_POINT('Ctrl Pts',(-1.13632278740328,1.63945054374864,27.0000204600093));
#17693=CARTESIAN_POINT('Ctrl Pts',(-1.13633640710348,1.63944110368742,27.0000215233541));
#17694=CARTESIAN_POINT('Ctrl Pts',(-1.1363431923928,1.63943640061798,27.0000220531083));
#17695=CARTESIAN_POINT('Ctrl Pts',(-1.1363567158736,1.63942702699959,27.0000231089384));
#17696=CARTESIAN_POINT('Ctrl Pts',(-1.13636345336495,1.63942235693681,27.0000236349596));
#17697=CARTESIAN_POINT('Ctrl Pts',(-1.13637688186724,1.63941304890638,27.0000246833719));
#17698=CARTESIAN_POINT('Ctrl Pts',(-1.13638357207035,1.63940841149955,27.0000252056999));
#17699=CARTESIAN_POINT('Ctrl Pts',(-1.13639690669461,1.63939916829942,27.0000262467803));
#17700=CARTESIAN_POINT('Ctrl Pts',(-1.13640355018902,1.63939456314938,27.0000267654603));
#17701=CARTESIAN_POINT('Ctrl Pts',(-1.13641679171046,1.63938538424726,27.0000277992694));
#17702=CARTESIAN_POINT('Ctrl Pts',(-1.13642338891197,1.63938081106828,27.000028314334));
#17703=CARTESIAN_POINT('Ctrl Pts',(-1.13643653856968,1.63937169561022,27.0000293409686));
#17704=CARTESIAN_POINT('Ctrl Pts',(-1.13644309005181,1.6393671540072,27.0000298524626));
#17705=CARTESIAN_POINT('Ctrl Pts',(-1.13645614861715,1.63935810146337,27.000030871983));
#17706=CARTESIAN_POINT('Ctrl Pts',(-1.13646265482215,1.63935359113216,27.0000313799408));
#17707=CARTESIAN_POINT('Ctrl Pts',(-1.13647562332389,1.63934460079418,27.0000323924274));
#17708=CARTESIAN_POINT('Ctrl Pts',(-1.13648208470954,1.63934012141982,27.0000328968849));
#17709=CARTESIAN_POINT('Ctrl Pts',(-1.1364949641901,1.63933119256976,27.000033902419));
#17710=CARTESIAN_POINT('Ctrl Pts',(-1.13650138127918,1.63932674379216,27.0000344034171));
#17711=CARTESIAN_POINT('Ctrl Pts',(-1.13651417252758,1.63931787588764,27.0000354020604));
#17712=CARTESIAN_POINT('Ctrl Pts',(-1.13652054573941,1.63931345741839,27.0000358996317));
#17713=CARTESIAN_POINT('Ctrl Pts',(-1.13653324979937,1.6393046497404,27.0000368914658));
#17714=CARTESIAN_POINT('Ctrl Pts',(-1.13653957962073,1.63930026124429,27.0000373856485));
#17715=CARTESIAN_POINT('Ctrl Pts',(-1.13655219733819,1.63929151321081,27.0000383707394));
#17716=CARTESIAN_POINT('Ctrl Pts',(-1.13655848421218,1.63928715438284,27.000038861568));
#17717=CARTESIAN_POINT('Ctrl Pts',(-1.13657101653701,1.6392784653397,27.00003983999));
#17718=CARTESIAN_POINT('Ctrl Pts',(-1.13657726094238,1.63927413585014,27.0000403275018));
#17719=CARTESIAN_POINT('Ctrl Pts',(-1.13658970860037,1.63926550529847,27.0000412993116));
#17720=CARTESIAN_POINT('Ctrl Pts',(-1.13659591088148,1.63926120491069,27.0000417835337));
#17721=CARTESIAN_POINT('Ctrl Pts',(-1.13660827507727,1.6392526320195,27.0000427488253));
#17722=CARTESIAN_POINT('Ctrl Pts',(-1.13661443580719,1.63924836033828,27.0000432298024));
#17723=CARTESIAN_POINT('Ctrl Pts',(-1.1366267170069,1.63923984478854,27.0000441886123));
#17724=CARTESIAN_POINT('Ctrl Pts',(-1.13663283649539,1.63923560160117,27.0000446663686));
#17725=CARTESIAN_POINT('Ctrl Pts',(-1.13664503586386,1.63922714258933,27.0000456187878));
#17726=CARTESIAN_POINT('Ctrl Pts',(-1.13665111461065,1.63922292755133,27.0000460933622));
#17727=CARTESIAN_POINT('Ctrl Pts',(-1.13666323275968,1.63921452465721,27.0000470394385));
#17728=CARTESIAN_POINT('Ctrl Pts',(-1.13666927110875,1.63921033753206,27.0000475108581));
#17729=CARTESIAN_POINT('Ctrl Pts',(-1.13668130906122,1.63920199005035,27.0000484506714));
#17730=CARTESIAN_POINT('Ctrl Pts',(-1.13668730747326,1.63919783052058,27.000048918972));
#17731=CARTESIAN_POINT('Ctrl Pts',(-1.13669926598296,1.63918953793247,27.0000498525811));
#17732=CARTESIAN_POINT('Ctrl Pts',(-1.13670522489986,1.63918540569359,27.0000503177974));
#17733=CARTESIAN_POINT('Ctrl Pts',(-1.13671710459646,1.63917716756629,27.0000512452516));
#17734=CARTESIAN_POINT('Ctrl Pts',(-1.13672302431496,1.63917306241443,27.0000517074067));
#17735=CARTESIAN_POINT('Ctrl Pts',(-1.13673484376495,1.63916486587626,27.0000526301554));
#17736=CARTESIAN_POINT('Ctrl Pts',(-1.13674074236875,1.63916077527178,27.0000530906612));
#17737=CARTESIAN_POINT('Ctrl Pts',(-1.13675243253278,1.63915266820433,27.0000540033147));
#17738=CARTESIAN_POINT('Ctrl Pts',(-1.13675827556691,1.63914861604453,27.0000544594811));
#17739=CARTESIAN_POINT('Ctrl Pts',(-1.13676992373392,1.63914053791732,27.000055368854));
#17740=CARTESIAN_POINT('Ctrl Pts',(-1.13677572883104,1.6391365119753,27.0000558220578));
#17741=CARTESIAN_POINT('Ctrl Pts',(-1.13925346042638,1.63741813988066,27.0002492582776));
#17742=CARTESIAN_POINT('Ctrl Pts',(-1.14172152583069,1.63569819026981,27.0004418561164));
#17743=CARTESIAN_POINT('Ctrl Pts',(-1.14680250842919,1.63214024351572,27.0008382036692));
#17744=CARTESIAN_POINT('Ctrl Pts',(-1.14941492217656,1.63030153801773,27.0010419046971));
#17745=CARTESIAN_POINT('Ctrl Pts',(-1.15597054390786,1.62566387878496,27.0015528960393));
#17746=CARTESIAN_POINT('Ctrl Pts',(-1.15990803898893,1.62285682899108,27.0018596492554));
#17747=CARTESIAN_POINT('Ctrl Pts',(-1.1710594687979,1.61484562897684,27.0027280663771));
#17748=CARTESIAN_POINT('Ctrl Pts',(-1.17824896006961,1.60960743030116,27.0032875384669));
#17749=CARTESIAN_POINT('Ctrl Pts',(-1.25118828974313,1.55571390605083,27.0089620474535));
#17750=CARTESIAN_POINT('Ctrl Pts',(-1.31392972634342,1.50310007948615,27.0138322171744));
#17751=CARTESIAN_POINT('Ctrl Pts',(-1.45250522768332,1.37156519692618,27.0250263347644));
#17752=CARTESIAN_POINT('Ctrl Pts',(-1.52542867529026,1.28997301021428,27.0312780848205));
#17753=CARTESIAN_POINT('Ctrl Pts',(-1.65036240995438,1.12468827804653,27.0434563626732));
#17754=CARTESIAN_POINT('Ctrl Pts',(-1.7035774775518,1.0423241588984,27.0493321343861));
#17755=CARTESIAN_POINT('Ctrl Pts',(-1.75662703441401,0.945225351725706,
27.0562402803651));
#17756=CARTESIAN_POINT('Ctrl Pts',(-1.76262126908009,0.93399986799092,27.0570384941142));
#17757=CARTESIAN_POINT('Ctrl Pts',(-1.77137099424231,0.917229895786987,
27.0582306534771));
#17758=CARTESIAN_POINT('Ctrl Pts',(-1.77420882270258,0.911728541293544,
27.0586216895752));
#17759=CARTESIAN_POINT('Ctrl Pts',(-1.77921882373372,0.901904288128219,
27.0593199493309));
#17760=CARTESIAN_POINT('Ctrl Pts',(-1.78140097253769,0.897586509501173,
27.0596268194676));
#17761=CARTESIAN_POINT('Ctrl Pts',(-1.78596587102549,0.888471810392974,
27.0602745991854));
#17762=CARTESIAN_POINT('Ctrl Pts',(-1.78834504743077,0.883673152663318,
27.0606156307748));
#17763=CARTESIAN_POINT('Ctrl Pts',(-1.79458102689322,0.870967221096795,
27.0615186288622));
#17764=CARTESIAN_POINT('Ctrl Pts',(-1.79840486034249,0.863043982942444,
27.0620817376635));
#17765=CARTESIAN_POINT('Ctrl Pts',(-1.81570537622565,0.826581897798144,
27.0646733929321));
#17766=CARTESIAN_POINT('Ctrl Pts',(-1.82855533660106,0.797752366493689,
27.0667234136914));
#17767=CARTESIAN_POINT('Ctrl Pts',(-1.86131944681613,0.719289011886853,
27.0723088058111));
#17768=CARTESIAN_POINT('Ctrl Pts',(-1.8799294563882,0.669142103562591,27.075885419658));
#17769=CARTESIAN_POINT('Ctrl Pts',(-1.96163191599517,0.418542261647544,
27.0937817462154));
#17770=CARTESIAN_POINT('Ctrl Pts',(-1.99477977691127,0.209778699509114,
27.1089346316281));
#17771=CARTESIAN_POINT('Ctrl Pts',(-1.99474997993175,-0.000282952760035267,
27.122784593986));
#17772=CARTESIAN_POINT('',(-1.99423734260986,0.00182902437498021,27.9209545793481));
#17773=CARTESIAN_POINT('Ctrl Pts',(-1.99793803718199,-0.000404756772601905,
27.1209548813952));
#17774=CARTESIAN_POINT('Ctrl Pts',(-1.997998332643,-0.0221817108798109,
27.1223511044342));
#17775=CARTESIAN_POINT('Ctrl Pts',(-1.98780192015059,-0.704986784517505,
27.1661326599454));
#17776=CARTESIAN_POINT('Ctrl Pts',(-1.21104617766535,-2.02391951718273,
27.2522995479288));
#17777=CARTESIAN_POINT('Ctrl Pts',(1.04595081287402,-2.11397018747171,27.3794555453455));
#17778=CARTESIAN_POINT('Ctrl Pts',(2.34362649946087,-0.265137487911111,
27.5066115427623));
#17779=CARTESIAN_POINT('Ctrl Pts',(1.49178348806736,1.82687303368368,27.633767540179));
#17780=CARTESIAN_POINT('Ctrl Pts',(-0.728287993893816,2.24331889271703,
27.7609235375957));
#17781=CARTESIAN_POINT('Ctrl Pts',(-1.89678409583614,1.00784192457324,27.8566525506522));
#17782=CARTESIAN_POINT('Ctrl Pts',(-1.9957770503294,0.173571652796369,27.9099962312363));
#17783=CARTESIAN_POINT('Ctrl Pts',(-1.99423734260986,0.00182902437498021,
27.9209545793481));
#17784=CARTESIAN_POINT('',(-1.99474936733483,-0.00158871561299351,29.5209548813952));
#17785=CARTESIAN_POINT('Ctrl Pts',(-1.99474918095302,0.00180764687956112,
27.9206602738335));
#17786=CARTESIAN_POINT('Ctrl Pts',(-1.9948488587779,-0.108187431123657,
27.9270492254735));
#17787=CARTESIAN_POINT('Ctrl Pts',(-1.98585070424739,-0.217993836220585,
27.9334945456375));
#17788=CARTESIAN_POINT('Ctrl Pts',(-1.96280274044711,-0.356908002681124,
27.9421072468327));
#17789=CARTESIAN_POINT('Ctrl Pts',(-1.9570528110152,-0.387197695487376,
27.9440126623984));
#17790=CARTESIAN_POINT('Ctrl Pts',(-1.94891803625653,-0.425218712387804,
27.9464440727496));
#17791=CARTESIAN_POINT('Ctrl Pts',(-1.94718482462179,-0.433086274475436,
27.9469493474341));
#17792=CARTESIAN_POINT('Ctrl Pts',(-1.94419251863576,-0.446288079912747,
27.9478009135796));
#17793=CARTESIAN_POINT('Ctrl Pts',(-1.94295900246288,-0.451628069954507,
27.9481463870098));
#17794=CARTESIAN_POINT('Ctrl Pts',(-1.94048310403884,-0.462148532350955,
27.9488290667236));
#17795=CARTESIAN_POINT('Ctrl Pts',(-1.93924194380808,-0.467329247417154,
27.9491662313082));
#17796=CARTESIAN_POINT('Ctrl Pts',(-1.93683248032129,-0.477211668323058,
27.9498112941003));
#17797=CARTESIAN_POINT('Ctrl Pts',(-1.93566777079769,-0.481914218119599,
27.9501190743796));
#17798=CARTESIAN_POINT('Ctrl Pts',(-1.93296257107925,-0.492668507097055,
27.9508248557851));
#17799=CARTESIAN_POINT('Ctrl Pts',(-1.93141077643851,-0.498717325014549,
27.9512232197657));
#17800=CARTESIAN_POINT('Ctrl Pts',(-1.92654017102483,-0.517338982165583,
27.9524539630782));
#17801=CARTESIAN_POINT('Ctrl Pts',(-1.92312685526473,-0.529886533407515,
27.9532893933809));
#17802=CARTESIAN_POINT('Ctrl Pts',(-1.88442469594449,-0.666856263853798,
27.962477870555));
#17803=CARTESIAN_POINT('Ctrl Pts',(-1.83724525305854,-0.787573412683344,
27.9712312103594));
#17804=CARTESIAN_POINT('Ctrl Pts',(-1.74804307272968,-0.963311674636439,
27.9848971552858));
#17805=CARTESIAN_POINT('Ctrl Pts',(-1.71429530269545,-1.02216208096058,
27.9896414887885));
#17806=CARTESIAN_POINT('Ctrl Pts',(-1.63197275561775,-1.15013510460071,
28.0002342633297));
#17807=CARTESIAN_POINT('Ctrl Pts',(-1.58186718386549,-1.21813173898929,
28.0060598161889));
#17808=CARTESIAN_POINT('Ctrl Pts',(-1.51535754053711,-1.29733633466164,
28.012922383088));
#17809=CARTESIAN_POINT('Ctrl Pts',(-1.50290561404906,-1.31174114134049,
28.0141736481886));
#17810=CARTESIAN_POINT('Ctrl Pts',(-1.48686705141871,-1.32976682757914,
28.0157410995416));
#17811=CARTESIAN_POINT('Ctrl Pts',(-1.48347072918528,-1.33355466380578,
28.0160705710444));
#17812=CARTESIAN_POINT('Ctrl Pts',(-1.47803327046113,-1.33957245116844,
28.0165940985729));
#17813=CARTESIAN_POINT('Ctrl Pts',(-1.47600152080552,-1.34181079567804,
28.016788847474));
#17814=CARTESIAN_POINT('Ctrl Pts',(-1.47213897557386,-1.34604670832224,
28.0171574201381));
#17815=CARTESIAN_POINT('Ctrl Pts',(-1.47030922084485,-1.34804514003558,
28.0173313146525));
#17816=CARTESIAN_POINT('Ctrl Pts',(-1.46610954310895,-1.35261324460278,
28.0177288406101));
#17817=CARTESIAN_POINT('Ctrl Pts',(-1.46373693623552,-1.35518041744453,
28.0179522645005));
#17818=CARTESIAN_POINT('Ctrl Pts',(-1.45623345015291,-1.36325653303465,
28.0186552618542));
#17819=CARTESIAN_POINT('Ctrl Pts',(-1.45107805077573,-1.36874275563258,
28.0191330010981));
#17820=CARTESIAN_POINT('Ctrl Pts',(-1.36038545806823,-1.46416677106235,
28.0274485389371));
#17821=CARTESIAN_POINT('Ctrl Pts',(-1.26665378726315,-1.54597262294863,
28.0346804661315));
#17822=CARTESIAN_POINT('Ctrl Pts',(-1.0827549897518,-1.67844336836413,28.0478359617263));
#17823=CARTESIAN_POINT('Ctrl Pts',(-0.995108985266902,-1.73184504700242,
28.0537487871243));
#17824=CARTESIAN_POINT('Ctrl Pts',(-0.860785713910868,-1.80011069958239,
28.0627261743796));
#17825=CARTESIAN_POINT('Ctrl Pts',(-0.817043979552869,-1.8203816075785,
28.0656357674478));
#17826=CARTESIAN_POINT('Ctrl Pts',(-0.745720868464329,-1.85034558920585,
28.0703894867717));
#17827=CARTESIAN_POINT('Ctrl Pts',(-0.718584957935787,-1.86105183518369,
28.0722001092982));
#17828=CARTESIAN_POINT('Ctrl Pts',(-0.68325472321027,-1.87410318339886,
28.0745640509535));
#17829=CARTESIAN_POINT('Ctrl Pts',(-0.675265701005148,-1.87699653389703,
28.0750990168539));
#17830=CARTESIAN_POINT('Ctrl Pts',(-0.662223200767148,-1.88162603722634,
28.0759731616288));
#17831=CARTESIAN_POINT('Ctrl Pts',(-0.657180745557097,-1.88339310245237,
28.0763113109999));
#17832=CARTESIAN_POINT('Ctrl Pts',(-0.647556457609245,-1.88672245716853,
28.0769571081101));
#17833=CARTESIAN_POINT('Ctrl Pts',(-0.642975911679219,-1.88828837111734,
28.0772646330781));
#17834=CARTESIAN_POINT('Ctrl Pts',(-0.632502220472329,-1.89182639846025,
28.0779682095009));
#17835=CARTESIAN_POINT('Ctrl Pts',(-0.62660549108438,-1.89378766970104,
28.0783646157899));
#17836=CARTESIAN_POINT('Ctrl Pts',(-0.608489224189546,-1.89971932330413,
28.0795834222711));
#17837=CARTESIAN_POINT('Ctrl Pts',(-0.59624060283813,-1.90359916315779,
28.0804087883287));
#17838=CARTESIAN_POINT('Ctrl Pts',(-0.48345272111354,-1.93813019163594,
28.0880222251436));
#17839=CARTESIAN_POINT('Ctrl Pts',(-0.380692221166983,-1.96090339362935,
28.0950689128245));
#17840=CARTESIAN_POINT('Ctrl Pts',(-0.100033376169267,-2.00020475838216,
28.114555936729));
#17841=CARTESIAN_POINT('Ctrl Pts',(0.0790748157565712,-2.0011427882299,
28.1273016039473));
#17842=CARTESIAN_POINT('Ctrl Pts',(0.272842792996786,-1.97607579201594,
28.1402460280279));
#17843=CARTESIAN_POINT('Ctrl Pts',(0.289737189206642,-1.97366945921006,
28.1413667161402));
#17844=CARTESIAN_POINT('Ctrl Pts',(0.311873338906946,-1.97022614729791,
28.1428228900185));
#17845=CARTESIAN_POINT('Ctrl Pts',(0.31714413784571,-1.96938458621994,28.1431687038633));
#17846=CARTESIAN_POINT('Ctrl Pts',(0.325449628297174,-1.96802428321856,
28.1437121134531));
#17847=CARTESIAN_POINT('Ctrl Pts',(0.328486557322551,-1.9675196623847,28.1439104944396));
#17848=CARTESIAN_POINT('Ctrl Pts',(0.334183327919764,-1.96655952055514,
28.1442820105553));
#17849=CARTESIAN_POINT('Ctrl Pts',(0.336843382502719,-1.96610563813862,
28.1444552334097));
#17850=CARTESIAN_POINT('Ctrl Pts',(0.342911938531253,-1.96505748912088,
28.1448498488545));
#17851=CARTESIAN_POINT('Ctrl Pts',(0.346319813258752,-1.9644597528389,28.145071041712));
#17852=CARTESIAN_POINT('Ctrl Pts',(0.356765585649676,-1.96259955278517,
28.1457478338592));
#17853=CARTESIAN_POINT('Ctrl Pts',(0.36379836145671,-1.96130809502991,28.1462018152134));
#17854=CARTESIAN_POINT('Ctrl Pts',(0.419956561957444,-1.95068307309188,
28.1498146181818));
#17855=CARTESIAN_POINT('Ctrl Pts',(0.468726922964491,-1.93954221601898,
28.1528767133679));
#17856=CARTESIAN_POINT('Ctrl Pts',(0.536098762612736,-1.92146179429727,
28.1570657349328));
#17857=CARTESIAN_POINT('Ctrl Pts',(0.555089568336457,-1.91606182574416,
28.1582418990978));
#17858=CARTESIAN_POINT('Ctrl Pts',(0.728676409687609,-1.86390550983009,
28.1689753750146));
#17859=CARTESIAN_POINT('Ctrl Pts',(0.877138124724071,-1.79881777428652,
28.178080382989));
#17860=CARTESIAN_POINT('Ctrl Pts',(1.05538048424197,-1.69330442618159,28.190449385624));
#17861=CARTESIAN_POINT('Ctrl Pts',(1.09381852538397,-1.66873258359326,28.1932080947884));
#17862=CARTESIAN_POINT('Ctrl Pts',(1.15444640877626,-1.62698049305864,28.1977360210615));
#17863=CARTESIAN_POINT('Ctrl Pts',(1.1771759258225,-1.61061129777603,28.199475686612));
#17864=CARTESIAN_POINT('Ctrl Pts',(1.20617196199933,-1.5887873996286,28.2017539001802));
#17865=CARTESIAN_POINT('Ctrl Pts',(1.21276031457067,-1.58376406677148,28.2022755826487));
#17866=CARTESIAN_POINT('Ctrl Pts',(1.22353879826998,-1.57543924864277,28.2031358104581));
#17867=CARTESIAN_POINT('Ctrl Pts',(1.22774736325156,-1.57216170547532,28.2034734077741));
#17868=CARTESIAN_POINT('Ctrl Pts',(1.23575166575061,-1.5658763799264,28.2041187911353));
#17869=CARTESIAN_POINT('Ctrl Pts',(1.23954970052589,-1.5628715736948,28.2044264571183));
#17870=CARTESIAN_POINT('Ctrl Pts',(1.24820944106847,-1.5559690171367,28.2051312594031));
#17871=CARTESIAN_POINT('Ctrl Pts',(1.25306388184865,-1.55206227246578,28.2055287550005));
#17872=CARTESIAN_POINT('Ctrl Pts',(1.26793844878344,-1.53997628400777,28.2067541952492));
#17873=CARTESIAN_POINT('Ctrl Pts',(1.27789723030394,-1.53172240333836,28.2075851529109));
#17874=CARTESIAN_POINT('Ctrl Pts',(1.37287002259834,-1.4514376536507,28.2156127728789));
#17875=CARTESIAN_POINT('Ctrl Pts',(1.45177324786449,-1.37251234376398,28.2231016668819));
#17876=CARTESIAN_POINT('Ctrl Pts',(1.62898361928755,-1.16278435095738,28.2420294174698));
#17877=CARTESIAN_POINT('Ctrl Pts',(1.71860637284411,-1.02569372192877,28.2536460575304));
#17878=CARTESIAN_POINT('Ctrl Pts',(1.80169253844813,-0.85648865762175,28.2662394804382));
#17879=CARTESIAN_POINT('Ctrl Pts',(1.81242093894593,-0.833546227255345,
28.2679115426011));
#17880=CARTESIAN_POINT('Ctrl Pts',(1.82496317330089,-0.805337030873813,
28.2699191567834));
#17881=CARTESIAN_POINT('Ctrl Pts',(1.82719510511738,-0.800260186951465,
28.2702785854422));
#17882=CARTESIAN_POINT('Ctrl Pts',(1.8306513900512,-0.792308533959701,28.2708385281359));
#17883=CARTESIAN_POINT('Ctrl Pts',(1.83189018888251,-0.78944009341247,28.2710399079798));
#17884=CARTESIAN_POINT('Ctrl Pts',(1.83418396613771,-0.784094376031744,
28.2714140530573));
#17885=CARTESIAN_POINT('Ctrl Pts',(1.8352406577118,-0.781617899346844,28.2715869196527));
#17886=CARTESIAN_POINT('Ctrl Pts',(1.83761743222252,-0.77601626537026,28.2719768983158));
#17887=CARTESIAN_POINT('Ctrl Pts',(1.83893455534687,-0.772889884068806,
28.2721938287564));
#17888=CARTESIAN_POINT('Ctrl Pts',(1.84278904494335,-0.763675065119153,
28.2728311312038));
#17889=CARTESIAN_POINT('Ctrl Pts',(1.84530422713305,-0.7575773105841,28.2732501791638));
#17890=CARTESIAN_POINT('Ctrl Pts',(1.86229067836662,-0.715809173467616,
28.2761030371072));
#17891=CARTESIAN_POINT('Ctrl Pts',(1.87575816200899,-0.679736076481537,
28.2784798387642));
#17892=CARTESIAN_POINT('Ctrl Pts',(1.89084255242143,-0.635460831147216,
28.2813184266714));
#17893=CARTESIAN_POINT('Ctrl Pts',(1.89346222303099,-0.627612013538339,
28.2818186713254));
#17894=CARTESIAN_POINT('Ctrl Pts',(1.91942574578575,-0.548180092639143,
28.2868535298067));
#17895=CARTESIAN_POINT('Ctrl Pts',(1.93874935254281,-0.475341032032919,
28.2912452195888));
#17896=CARTESIAN_POINT('Ctrl Pts',(1.97421614778847,-0.302775202752894,
28.3014757249079));
#17897=CARTESIAN_POINT('Ctrl Pts',(1.98699887005701,-0.202574944284822,
28.307289862144));
#17898=CARTESIAN_POINT('Ctrl Pts',(1.99477475220788,-0.0504702691893337,
28.3163398191186));
#17899=CARTESIAN_POINT('Ctrl Pts',(1.99541273629413,0.000980898739392213,
28.319437753608));
#17900=CARTESIAN_POINT('Ctrl Pts',(1.99325562074871,0.0830746017359388,
28.3244779275436));
#17901=CARTESIAN_POINT('Ctrl Pts',(1.99174169969109,0.1137286266368,28.3263814704997));
#17902=CARTESIAN_POINT('Ctrl Pts',(1.98889097181835,0.153023406443363,28.3288539138327));
#17903=CARTESIAN_POINT('Ctrl Pts',(1.988203691165,0.161708191687293,28.329402389689));
#17904=CARTESIAN_POINT('Ctrl Pts',(1.98700367172813,0.175705591025923,28.3302897513201));
#17905=CARTESIAN_POINT('Ctrl Pts',(1.98652645835821,0.18102120184792,28.3306275188579));
#17906=CARTESIAN_POINT('Ctrl Pts',(1.98557559174698,0.191155904136875,28.3312730292296));
#17907=CARTESIAN_POINT('Ctrl Pts',(1.98510571109182,0.195975318188174,28.3315806511644));
#17908=CARTESIAN_POINT('Ctrl Pts',(1.98399157535436,0.206987329738948,28.3322850727164));
#17909=CARTESIAN_POINT('Ctrl Pts',(1.98333586890655,0.213178693600943,28.3326822302442));
#17910=CARTESIAN_POINT('Ctrl Pts',(1.98123169889738,0.232196314470544,28.3339056094976));
#17911=CARTESIAN_POINT('Ctrl Pts',(1.97968773895219,0.245011461753481,28.3347348295458));
#17912=CARTESIAN_POINT('Ctrl Pts',(1.96007379363193,0.395497073248164,28.3445307409932));
#17913=CARTESIAN_POINT('Ctrl Pts',(1.92780509994746,0.530905244818358,28.3539633486042));
#17914=CARTESIAN_POINT('Ctrl Pts',(1.85006895750508,0.751924979456092,28.3702475278558));
#17915=CARTESIAN_POINT('Ctrl Pts',(1.81195759263666,0.839616850551108,28.3769543942392));
#17916=CARTESIAN_POINT('Ctrl Pts',(1.7476381706149,0.962634550685788,28.3864960103221));
#17917=CARTESIAN_POINT('Ctrl Pts',(1.72631807205538,1.00036538123331,28.3894407175468));
#17918=CARTESIAN_POINT('Ctrl Pts',(1.69204864893731,1.05664951501344,28.3938302446829));
#17919=CARTESIAN_POINT('Ctrl Pts',(1.67998579527088,1.07572518001221,28.395317305614));
#17920=CARTESIAN_POINT('Ctrl Pts',(1.66466682059457,1.09906348074963,28.3971319636515));
#17921=CARTESIAN_POINT('Ctrl Pts',(1.6617144412548,1.10352221347523,28.397478433907));
#17922=CARTESIAN_POINT('Ctrl Pts',(1.6570329396053,1.11053090486523,28.3980226413182));
#17923=CARTESIAN_POINT('Ctrl Pts',(1.65531580609073,1.11308878173306,28.3982211675244));
#17924=CARTESIAN_POINT('Ctrl Pts',(1.65208367773634,1.11787940512931,28.3985928071755));
#17925=CARTESIAN_POINT('Ctrl Pts',(1.65057009619025,1.1201130301579,28.3987660090131));
#17926=CARTESIAN_POINT('Ctrl Pts',(1.64710722883944,1.12520099795319,28.3991603826025));
#17927=CARTESIAN_POINT('Ctrl Pts',(1.64515505739347,1.12805334389094,28.3993813555543));
#17928=CARTESIAN_POINT('Ctrl Pts',(1.63915172603117,1.1367761676498,28.4000568118091));
#17929=CARTESIAN_POINT('Ctrl Pts',(1.63507643004821,1.14263008357578,28.4005096864588));
#17930=CARTESIAN_POINT('Ctrl Pts',(1.60246143774226,1.18894773292987,28.404090633603));
#17931=CARTESIAN_POINT('Ctrl Pts',(1.57245273435331,1.22836180101792,28.4071238766074));
#17932=CARTESIAN_POINT('Ctrl Pts',(1.52751188910998,1.28303802050906,28.4113758953845));
#17933=CARTESIAN_POINT('Ctrl Pts',(1.51375665571716,1.2992382263748,28.4126415931688));
#17934=CARTESIAN_POINT('Ctrl Pts',(1.46585609938205,1.35385937919311,28.4169411445562));
#17935=CARTESIAN_POINT('Ctrl Pts',(1.43048526794351,1.39117992386851,28.4199348891131));
#17936=CARTESIAN_POINT('Ctrl Pts',(1.32175213313475,1.49736959089023,28.4287596645015));
#17937=CARTESIAN_POINT('Ctrl Pts',(1.24458219000189,1.56210064787829,28.4345587782487));
#17938=CARTESIAN_POINT('Ctrl Pts',(1.12136227061537,1.65050999415747,28.4435728786602));
#17939=CARTESIAN_POINT('Ctrl Pts',(1.07873527500381,1.67867989518207,28.4466498935754));
#17940=CARTESIAN_POINT('Ctrl Pts',(1.00897644832623,1.72102478567767,28.4516589950286));
#17941=CARTESIAN_POINT('Ctrl Pts',(0.982517221822658,1.73626597533137,28.4535529969281));
#17942=CARTESIAN_POINT('Ctrl Pts',(0.948086501498887,1.75505987768894,28.4560147039504));
#17943=CARTESIAN_POINT('Ctrl Pts',(0.940426228301183,1.75917642488258,28.4565622050836));
#17944=CARTESIAN_POINT('Ctrl Pts',(0.928024848082484,1.76573664242315,28.4574483696088));
#17945=CARTESIAN_POINT('Ctrl Pts',(0.923300371903209,1.76821164779454,28.4577859202893));
#17946=CARTESIAN_POINT('Ctrl Pts',(0.914266994254903,1.77289787680985,28.4584312689427));
#17947=CARTESIAN_POINT('Ctrl Pts',(0.90995984838636,1.77511241672905,28.4587389470827));
#17948=CARTESIAN_POINT('Ctrl Pts',(0.900091411353814,1.78014096639524,28.4594438541086));
#17949=CARTESIAN_POINT('Ctrl Pts',(0.894524932225519,1.78294462987522,28.4598414426709));
#17950=CARTESIAN_POINT('Ctrl Pts',(0.877359703756071,1.79148960536398,28.4610674500144));
#17951=CARTESIAN_POINT('Ctrl Pts',(0.86571833009461,1.79714407205301,28.4618988858538));
#17952=CARTESIAN_POINT('Ctrl Pts',(0.752116882131041,1.85096282619706,28.4700133791482));
#17953=CARTESIAN_POINT('Ctrl Pts',(0.646319007684455,1.8905044296857,28.4775960849527));
#17954=CARTESIAN_POINT('Ctrl Pts',(0.381651232324477,1.96459952588244,28.4965521000674));
#17955=CARTESIAN_POINT('Ctrl Pts',(0.220796412546314,1.98911000588865,28.5080893573319));
#17956=CARTESIAN_POINT('Ctrl Pts',(0.0336924542626241,1.99462296304493,
28.5205913915823));
#17957=CARTESIAN_POINT('Ctrl Pts',(0.00862257998748717,1.99488890472777,
28.5222462745928));
#17958=CARTESIAN_POINT('Ctrl Pts',(-0.0219751936630706,1.99463661249876,
28.5242360629406));
#17959=CARTESIAN_POINT('Ctrl Pts',(-0.0275032138512781,1.99456804848868,
28.5245943569389));
#17960=CARTESIAN_POINT('Ctrl Pts',(-0.0361511979486837,1.99442482735281,
28.5251529230146));
#17961=CARTESIAN_POINT('Ctrl Pts',(-0.0392713397609173,1.99436582985066,
28.5253540540604));
#17962=CARTESIAN_POINT('Ctrl Pts',(-0.0450836736811598,1.99424228134761,
28.5257279751567));
#17963=CARTESIAN_POINT('Ctrl Pts',(-0.0477758455136173,1.99417960150707,
28.5259008654485));
#17964=CARTESIAN_POINT('Ctrl Pts',(-0.0538645722213104,1.99402550507804,
28.526291201874));
#17965=CARTESIAN_POINT('Ctrl Pts',(-0.0572610162880835,1.99393086226059,
28.5265084649647));
#17966=CARTESIAN_POINT('Ctrl Pts',(-0.0672745137298622,1.99362622656238,
28.5271476455265));
#17967=CARTESIAN_POINT('Ctrl Pts',(-0.0738908635736979,1.99339196714712,
28.5275682272445));
#17968=CARTESIAN_POINT('Ctrl Pts',(-0.119437105290997,1.99155226927821,
28.5304521519316));
#17969=CARTESIAN_POINT('Ctrl Pts',(-0.158316924483955,1.9888393357482,28.5328570723449));
#17970=CARTESIAN_POINT('Ctrl Pts',(-0.205613072318936,1.98414316379529,
28.5357401070166));
#17971=CARTESIAN_POINT('Ctrl Pts',(-0.214125411102993,1.9832425828003,28.5362573075835));
#17972=CARTESIAN_POINT('Ctrl Pts',(-0.296658556264859,1.97397323843552,
28.54125779541));
#17973=CARTESIAN_POINT('Ctrl Pts',(-0.37016661640658,1.96151849363895,28.545602647005));
#17974=CARTESIAN_POINT('Ctrl Pts',(-0.54116471114962,1.92258768611686,28.5557867603395));
#17975=CARTESIAN_POINT('Ctrl Pts',(-0.637677343617685,1.8927675919447,28.5616010101356));
#17976=CARTESIAN_POINT('Ctrl Pts',(-0.779374357505934,1.83691302177656,
28.5706512359994));
#17977=CARTESIAN_POINT('Ctrl Pts',(-0.82648162855732,1.81620520495156,28.5737493275081));
#17978=CARTESIAN_POINT('Ctrl Pts',(-0.900330158003393,1.78027386590774,
28.578789734592));
#17979=CARTESIAN_POINT('Ctrl Pts',(-0.927612022138495,1.76621210705733,
28.5806933490642));
#17980=CARTESIAN_POINT('Ctrl Pts',(-0.962207341533233,1.74735814721426,
28.5831658728592));
#17981=CARTESIAN_POINT('Ctrl Pts',(-0.969829645405149,1.74313909879577,
28.5837143560037));
#17982=CARTESIAN_POINT('Ctrl Pts',(-0.982076390068085,1.7362551686107,28.5846017265861));
#17983=CARTESIAN_POINT('Ctrl Pts',(-0.986718258210205,1.73362139017375,
28.5849394957454));
#17984=CARTESIAN_POINT('Ctrl Pts',(-0.995551411923868,1.72856252313407,
28.5855850073296));
#17985=CARTESIAN_POINT('Ctrl Pts',(-0.999744552194042,1.7261407358168,28.5858926288472));
#17986=CARTESIAN_POINT('Ctrl Pts',(-1.00930878390367,1.72057028448836,28.5865970467841));
#17987=CARTESIAN_POINT('Ctrl Pts',(-1.01467401450222,1.71741170601885,28.5869942011008));
#17988=CARTESIAN_POINT('Ctrl Pts',(-1.03111665556537,1.70762777244415,28.5882175607874));
#17989=CARTESIAN_POINT('Ctrl Pts',(-1.04214444286321,1.70092007860325,28.5890467643408));
#17990=CARTESIAN_POINT('Ctrl Pts',(-1.17103221474944,1.6207996448405,28.5988428251249));
#17991=CARTESIAN_POINT('Ctrl Pts',(-1.28095765868645,1.53539606730419,28.6082756176316));
#17992=CARTESIAN_POINT('Ctrl Pts',(-1.4504619328874,1.37274409901416,28.6246034630679));
#17993=CARTESIAN_POINT('Ctrl Pts',(-1.51491446163045,1.30126893012597,28.6313547668556));
#17994=CARTESIAN_POINT('Ctrl Pts',(-1.61243254779729,1.17601450054307,28.6422622615272));
#17995=CARTESIAN_POINT('Ctrl Pts',(-1.64855816363113,1.12481402539167,28.6464949243507));
#17996=CARTESIAN_POINT('Ctrl Pts',(-1.68593207919727,1.06616525152659,28.6510299329688));
#17997=CARTESIAN_POINT('Ctrl Pts',(-1.68961565521088,1.06031799961346,28.6514787299775));
#17998=CARTESIAN_POINT('Ctrl Pts',(-1.69507253972901,1.05155517700529,28.6521461938519));
#17999=CARTESIAN_POINT('Ctrl Pts',(-1.69686882686442,1.04865408504055,28.6523663381321));
#18000=CARTESIAN_POINT('Ctrl Pts',(-1.69993623789927,1.04367154675,28.6527429858973));
#18001=CARTESIAN_POINT('Ctrl Pts',(-1.70121099411477,1.04159236948486,28.6528997283202));
#18002=CARTESIAN_POINT('Ctrl Pts',(-1.70385668843163,1.03725932482433,28.6532254843586));
#18003=CARTESIAN_POINT('Ctrl Pts',(-1.70522696424618,1.03500508320219,28.6533944545134));
#18004=CARTESIAN_POINT('Ctrl Pts',(-1.70901131811047,1.02875152449604,28.6538618280001));
#18005=CARTESIAN_POINT('Ctrl Pts',(-1.71141584531744,1.02474640279759,28.6541596091982));
#18006=CARTESIAN_POINT('Ctrl Pts',(-1.7208899483535,1.00883942184153,28.6553363152862));
#18007=CARTESIAN_POINT('Ctrl Pts',(-1.72784982559635,0.996872208043418,
28.656208360038));
#18008=CARTESIAN_POINT('Ctrl Pts',(-1.80206153953116,0.866155714711338,
28.6656017863877));
#18009=CARTESIAN_POINT('Ctrl Pts',(-1.85709241189678,0.740858143128636,
28.6734488105635));
#18010=CARTESIAN_POINT('Ctrl Pts',(-1.94471316947856,0.468503516428646,
28.6900445652401));
#18011=CARTESIAN_POINT('Ctrl Pts',(-1.97435651117497,0.321422753812011,
28.6987770975993));
#18012=CARTESIAN_POINT('Ctrl Pts',(-1.98849629030544,0.158450929540045,
28.7089755260542));
#18013=CARTESIAN_POINT('Ctrl Pts',(-1.98956099339607,0.14446878984764,28.7098542040393));
#18014=CARTESIAN_POINT('Ctrl Pts',(-1.99089936413085,0.124051394489923,
28.7111431302214));
#18015=CARTESIAN_POINT('Ctrl Pts',(-1.99128943734173,0.117623984478175,
28.7115497275067));
#18016=CARTESIAN_POINT('Ctrl Pts',(-1.99191996600305,0.106330374348276,
28.7122656839352));
#18017=CARTESIAN_POINT('Ctrl Pts',(-1.99217372820879,0.101464946733168,
28.7125746233066));
#18018=CARTESIAN_POINT('Ctrl Pts',(-1.99263245246311,0.092003464455076,
28.7131763823591));
#18019=CARTESIAN_POINT('Ctrl Pts',(-1.99283934402496,0.0874075305839507,
28.7134691395138));
#18020=CARTESIAN_POINT('Ctrl Pts',(-1.99334947385015,0.0751301183457592,
28.7142524272093));
#18021=CARTESIAN_POINT('Ctrl Pts',(-1.99362420707482,0.0674475930284423,
28.7147438478344));
#18022=CARTESIAN_POINT('Ctrl Pts',(-1.9944580660606,0.039628166695913,28.7165281078017));
#18023=CARTESIAN_POINT('Ctrl Pts',(-1.99475653782484,0.0194852291280238,
28.7178290653352));
#18024=CARTESIAN_POINT('Ctrl Pts',(-1.99471414962915,-0.108981530156663,
28.726186735529));
#18025=CARTESIAN_POINT('Ctrl Pts',(-1.98585510854521,-0.217104110198715,
28.7335099860569));
#18026=CARTESIAN_POINT('Ctrl Pts',(-1.95017202380689,-0.433903165838728,
28.7486975897034));
#18027=CARTESIAN_POINT('Ctrl Pts',(-1.92289666575832,-0.54213527506093,
28.7565445088277));
#18028=CARTESIAN_POINT('Ctrl Pts',(-1.88156110723056,-0.662577316698417,
28.7653130744021));
#18029=CARTESIAN_POINT('Ctrl Pts',(-1.87621425332714,-0.677569920442628,
28.7664049622123));
#18030=CARTESIAN_POINT('Ctrl Pts',(-1.85310804433251,-0.739988247359653,
28.7709483466015));
#18031=CARTESIAN_POINT('Ctrl Pts',(-1.83372374141393,-0.786797486294951,
28.7743499537053));
#18032=CARTESIAN_POINT('Ctrl Pts',(-1.80958200636124,-0.839340202702134,
28.7781224611971));
#18033=CARTESIAN_POINT('Ctrl Pts',(-1.80655206119685,-0.845841987371237,
28.7785884576203));
#18034=CARTESIAN_POINT('Ctrl Pts',(-1.80200678919792,-0.855459581685445,
28.7792763908909));
#18035=CARTESIAN_POINT('Ctrl Pts',(-1.80051835286999,-0.858587925396768,
28.7794999394336));
#18036=CARTESIAN_POINT('Ctrl Pts',(-1.79785583679301,-0.864146536755718,
28.7798967440929));
#18037=CARTESIAN_POINT('Ctrl Pts',(-1.79668497023471,-0.866578308597457,
28.7800701969766));
#18038=CARTESIAN_POINT('Ctrl Pts',(-1.79416923394782,-0.871776222614569,
28.7804406471021));
#18039=CARTESIAN_POINT('Ctrl Pts',(-1.79282290566948,-0.874541623698549,
28.7806375513462));
#18040=CARTESIAN_POINT('Ctrl Pts',(-1.78912837884946,-0.882085913014618,
28.7811742549826));
#18041=CARTESIAN_POINT('Ctrl Pts',(-1.78676741226213,-0.88685857383781,
28.7815132667839));
#18042=CARTESIAN_POINT('Ctrl Pts',(-1.77443295389376,-0.911543312931353,
28.7832642839135));
#18043=CARTESIAN_POINT('Ctrl Pts',(-1.76414514815424,-0.931297759400841,
28.7846574881144));
#18044=CARTESIAN_POINT('Ctrl Pts',(-1.73327129156678,-0.988232768113368,
28.788661286012));
#18045=CARTESIAN_POINT('Ctrl Pts',(-1.71182445327314,-1.02493459135154,
28.7912276651434));
#18046=CARTESIAN_POINT('Ctrl Pts',(-1.6667314124389,-1.09673233812433,28.7962749160996));
#18047=CARTESIAN_POINT('Ctrl Pts',(-1.64310909123347,-1.13181632821076,
28.7987548732284));
#18048=CARTESIAN_POINT('Ctrl Pts',(-1.51105934730419,-1.31507967487548,
28.8119230576086));
#18049=CARTESIAN_POINT('Ctrl Pts',(-1.38369502282115,-1.44848791593372,
28.8223800174364));
#18050=CARTESIAN_POINT('Ctrl Pts',(-1.22473389858077,-1.57462014987328,
28.8349569923934));
#18051=CARTESIAN_POINT('Ctrl Pts',(-1.20940731850038,-1.58642227525399,
28.8361642133571));
#18052=CARTESIAN_POINT('Ctrl Pts',(-1.18785383824973,-1.60252550942171,
28.8378556223933));
#18053=CARTESIAN_POINT('Ctrl Pts',(-1.18177011838386,-1.60701715427708,
28.8383323573164));
#18054=CARTESIAN_POINT('Ctrl Pts',(-1.17196385512846,-1.61417137558665,
28.8390997728462));
#18055=CARTESIAN_POINT('Ctrl Pts',(-1.16825739186188,-1.61685595316363,
28.8393895986907));
#18056=CARTESIAN_POINT('Ctrl Pts',(-1.16057559543045,-1.62237964532267,
28.8399898110114));
#18057=CARTESIAN_POINT('Ctrl Pts',(-1.15659900935151,-1.62521695694302,
28.8403002642142));
#18058=CARTESIAN_POINT('Ctrl Pts',(-1.14728884903925,-1.63180832183931,
28.8410265402503));
#18059=CARTESIAN_POINT('Ctrl Pts',(-1.14194722931651,-1.63555086320754,
28.8414427999714));
#18060=CARTESIAN_POINT('Ctrl Pts',(-1.1246950284426,-1.64751269306515,28.8427858967837));
#18061=CARTESIAN_POINT('Ctrl Pts',(-1.11271354660261,-1.65562843828706,
28.8437166466276));
#18062=CARTESIAN_POINT('Ctrl Pts',(-1.08455977215657,-1.6742549545944,28.8458994631623));
#18063=CARTESIAN_POINT('Ctrl Pts',(-1.06832145412354,-1.68466280891969,
28.847155256294));
#18064=CARTESIAN_POINT('Ctrl Pts',(-1.01114414279012,-1.72015115414572,
28.8515670047184));
#18065=CARTESIAN_POINT('Ctrl Pts',(-0.969455373519259,-1.74398627378409,
28.8547664537349));
#18066=CARTESIAN_POINT('Ctrl Pts',(-0.745721542894918,-1.86140173857443,
28.8718446249199));
#18067=CARTESIAN_POINT('Ctrl Pts',(-0.550969067616661,-1.92803863518309,
28.8865600281095));
#18068=CARTESIAN_POINT('Ctrl Pts',(-0.324646806815428,-1.96831644570493,
28.9019239899371));
#18069=CARTESIAN_POINT('Ctrl Pts',(-0.299703112936946,-1.97226858489174,
28.9035921542577));
#18070=CARTESIAN_POINT('Ctrl Pts',(-0.269474391401096,-1.97647131023088,
28.9055781287364));
#18071=CARTESIAN_POINT('Ctrl Pts',(-0.264256152169708,-1.97717575732305,
28.9059196788122));
#18072=CARTESIAN_POINT('Ctrl Pts',(-0.255690802489784,-1.97829753886518,
28.9064781426427));
#18073=CARTESIAN_POINT('Ctrl Pts',(-0.2523453553774,-1.97872705565714,28.9066957257752));
#18074=CARTESIAN_POINT('Ctrl Pts',(-0.246328760360316,-1.97948401011462,
28.9070860442729));
#18075=CARTESIAN_POINT('Ctrl Pts',(-0.243658038688621,-1.97981452791526,
28.9072589512672));
#18076=CARTESIAN_POINT('Ctrl Pts',(-0.237870546319849,-1.98051887628678,
28.9076328776779));
#18077=CARTESIAN_POINT('Ctrl Pts',(-0.2347535708981,-1.98089075352932,28.9078337854563));
#18078=CARTESIAN_POINT('Ctrl Pts',(-0.226061533751702,-1.98190697096103,
28.9083927393424));
#18079=CARTESIAN_POINT('Ctrl Pts',(-0.220484556727129,-1.98253514991819,
28.9087498846769));
#18080=CARTESIAN_POINT('Ctrl Pts',(-0.188728861274787,-1.98597638753548,
28.910775397344));
#18081=CARTESIAN_POINT('Ctrl Pts',(-0.162497652783014,-1.98829461373648,
28.9124172394034));
#18082=CARTESIAN_POINT('Ctrl Pts',(-0.0818331088866023,-1.99381629885062,
28.9173912975349));
#18083=CARTESIAN_POINT('Ctrl Pts',(-0.0273052753965819,-1.99530835900851,
28.9206496380073));
#18084=CARTESIAN_POINT('Ctrl Pts',(0.20736304840412,-1.99210592287502,28.9344791456531));
#18085=CARTESIAN_POINT('Ctrl Pts',(0.38633516320598,-1.96525631504857,28.9446191812516));
#18086=CARTESIAN_POINT('Ctrl Pts',(0.600730879483488,-1.90263375907195,
28.9581839365838));
#18087=CARTESIAN_POINT('Ctrl Pts',(0.641780317589034,-1.8891824699964,28.960844073649));
#18088=CARTESIAN_POINT('Ctrl Pts',(0.691040121572739,-1.87124997485393,
28.9641268921308));
#18089=CARTESIAN_POINT('Ctrl Pts',(0.699699385512237,-1.86802935826141,
28.9647074111543));
#18090=CARTESIAN_POINT('Ctrl Pts',(0.713940085196567,-1.86261994419518,
28.9656679321634));
#18091=CARTESIAN_POINT('Ctrl Pts',(0.719534645891043,-1.86046590773675,
28.9660467700006));
#18092=CARTESIAN_POINT('Ctrl Pts',(0.729607597320129,-1.85653535595333,
28.9667315926145));
#18093=CARTESIAN_POINT('Ctrl Pts',(0.734089440017328,-1.85476776642234,
28.9670372753345));
#18094=CARTESIAN_POINT('Ctrl Pts',(0.743650898288416,-1.85095674773058,
28.96769152649));
#18095=CARTESIAN_POINT('Ctrl Pts',(0.748728582957581,-1.84890861011862,
28.9680402518389));
#18096=CARTESIAN_POINT('Ctrl Pts',(0.762439089720262,-1.84331259148635,
28.9689853660675));
#18097=CARTESIAN_POINT('Ctrl Pts',(0.771055464585957,-1.83972501779039,
28.9695830949572));
#18098=CARTESIAN_POINT('Ctrl Pts',(0.814261921305348,-1.8213784299329,28.9725996871596));
#18099=CARTESIAN_POINT('Ctrl Pts',(0.848452900643053,-1.80570463168776,
28.9750495551128));
#18100=CARTESIAN_POINT('Ctrl Pts',(1.03735806830711,-1.71255698347804,28.9889518884468));
#18101=CARTESIAN_POINT('Ctrl Pts',(1.18190057624895,-1.61618457713856,29.0010869333275));
#18102=CARTESIAN_POINT('Ctrl Pts',(1.38119475596547,-1.44212606645502,29.0194783669569));
#18103=CARTESIAN_POINT('Ctrl Pts',(1.4459937290459,-1.37714670146729,29.025775024701));
#18104=CARTESIAN_POINT('Ctrl Pts',(1.51124880282904,-1.30200471192509,29.032275921467));
#18105=CARTESIAN_POINT('Ctrl Pts',(1.5163622153359,-1.29604585211747,29.0327864665345));
#18106=CARTESIAN_POINT('Ctrl Pts',(1.52374025164694,-1.28734449703983,29.033524580157));
#18107=CARTESIAN_POINT('Ctrl Pts',(1.5260328571933,-1.28462598751368,29.0337541443793));
#18108=CARTESIAN_POINT('Ctrl Pts',(1.53006500723379,-1.27981874679317,29.0341582379606));
#18109=CARTESIAN_POINT('Ctrl Pts',(1.53180756694164,-1.27773257343879,29.0343329874514));
#18110=CARTESIAN_POINT('Ctrl Pts',(1.53545875071363,-1.27334321161228,29.0346993718054));
#18111=CARTESIAN_POINT('Ctrl Pts',(1.53736645588965,-1.27103929533922,29.0348909400539));
#18112=CARTESIAN_POINT('Ctrl Pts',(1.54241442116777,-1.2649149270363,29.0353982368048));
#18113=CARTESIAN_POINT('Ctrl Pts',(1.54554569365455,-1.2610870427348,29.0357133171453));
#18114=CARTESIAN_POINT('Ctrl Pts',(1.55994474606134,-1.24335045875706,29.0371642809629));
#18115=CARTESIAN_POINT('Ctrl Pts',(1.57103966019165,-1.22930159609517,29.0382882119811));
#18116=CARTESIAN_POINT('Ctrl Pts',(1.60092235390202,-1.19039732681759,29.0413377954715));
#18117=CARTESIAN_POINT('Ctrl Pts',(1.61931996037841,-1.1652472988396,29.0432405385104));
#18118=CARTESIAN_POINT('Ctrl Pts',(1.68182768286329,-1.0754561395538,29.0498362511993));
#18119=CARTESIAN_POINT('Ctrl Pts',(1.7227193695473,-1.00865750056799,29.0543959596488));
#18120=CARTESIAN_POINT('Ctrl Pts',(1.83580657082673,-0.796885439706245,
29.0683330555924));
#18121=CARTESIAN_POINT('Ctrl Pts',(1.89436954801904,-0.645421549219721,
29.0776562873066));
#18122=CARTESIAN_POINT('Ctrl Pts',(1.93609728797778,-0.480237901491215,
29.0881992892549));
#18123=CARTESIAN_POINT('Ctrl Pts',(1.93814460186183,-0.471907458398522,
29.0887317670717));
#18124=CARTESIAN_POINT('Ctrl Pts',(1.94358041390635,-0.449157153770234,
29.0901882930147));
#18125=CARTESIAN_POINT('Ctrl Pts',(1.94686207603639,-0.434712562798446,
29.0911156242695));
#18126=CARTESIAN_POINT('Ctrl Pts',(1.951264204639,-0.414285627306019,29.0924311177005));
#18127=CARTESIAN_POINT('Ctrl Pts',(1.95251868579219,-0.4083324106673,29.0928149929511));
#18128=CARTESIAN_POINT('Ctrl Pts',(1.9546568830613,-0.397950282866235,29.0934853411271));
#18129=CARTESIAN_POINT('Ctrl Pts',(1.95555283410524,-0.393523913640471,
29.0937714212993));
#18130=CARTESIAN_POINT('Ctrl Pts',(1.9573948691668,-0.384261847740866,29.0943706401701));
#18131=CARTESIAN_POINT('Ctrl Pts',(1.95833808154993,-0.379425617353974,
29.0946838683166));
#18132=CARTESIAN_POINT('Ctrl Pts',(1.96053461222629,-0.367936714056487,
29.0954288079074));
#18133=CARTESIAN_POINT('Ctrl Pts',(1.96177199554775,-0.361281091261387,
29.0958610237646));
#18134=CARTESIAN_POINT('Ctrl Pts',(1.96579554065173,-0.339008984680679,
29.0973096749342));
#18135=CARTESIAN_POINT('Ctrl Pts',(1.9684292379113,-0.323365908056735,29.0983309345434));
#18136=CARTESIAN_POINT('Ctrl Pts',(1.98132649765105,-0.2407547901593,29.1037453602466));
#18137=CARTESIAN_POINT('Ctrl Pts',(1.98835883985264,-0.17333461019308,29.1082394640348));
#18138=CARTESIAN_POINT('Ctrl Pts',(2.00186604230606,0.0812282774462531,
29.1254932894691));
#18139=CARTESIAN_POINT('Ctrl Pts',(1.98542547337194,0.268584748349885,29.1388737696367));
#18140=CARTESIAN_POINT('Ctrl Pts',(1.9343622492687,0.488643386563524,29.1541608676364));
#18141=CARTESIAN_POINT('Ctrl Pts',(1.92450248806679,0.526137182303195,29.1567450723227));
#18142=CARTESIAN_POINT('Ctrl Pts',(1.91168903488861,0.569663307121081,29.1597026049817));
#18143=CARTESIAN_POINT('Ctrl Pts',(1.90979092533172,0.575994682353422,29.1601317459518));
#18144=CARTESIAN_POINT('Ctrl Pts',(1.90687014339245,0.585564127636601,29.1607786240099));
#18145=CARTESIAN_POINT('Ctrl Pts',(1.90587063928647,0.588809135512055,29.1609976772601));
#18146=CARTESIAN_POINT('Ctrl Pts',(1.90406363099731,0.594622991808482,29.1613895749004));
#18147=CARTESIAN_POINT('Ctrl Pts',(1.90325921006232,0.597192760236961,29.161562597133));
#18148=CARTESIAN_POINT('Ctrl Pts',(1.90151077950734,0.602738804891277,29.1619355779196));
#18149=CARTESIAN_POINT('Ctrl Pts',(1.90056498814935,0.605714485259134,29.1621354296799));
#18150=CARTESIAN_POINT('Ctrl Pts',(1.89792294039877,0.613959869602264,29.1626884926003));
#18151=CARTESIAN_POINT('Ctrl Pts',(1.89621171163819,0.619224802134308,29.1630408336124));
#18152=CARTESIAN_POINT('Ctrl Pts',(1.88659587582984,0.648396142182027,29.1649889176962));
#18153=CARTESIAN_POINT('Ctrl Pts',(1.87826066461932,0.672159635344352,29.1665604570017));
#18154=CARTESIAN_POINT('Ctrl Pts',(1.81278531401672,0.848089029542241,29.1781243127945));
#18155=CARTESIAN_POINT('Ctrl Pts',(1.73768097503996,0.992937477844196,29.1872866822992));
#18156=CARTESIAN_POINT('Ctrl Pts',(1.58243076691096,1.21964194985828,29.2033488437942));
#18157=CARTESIAN_POINT('Ctrl Pts',(1.51135606335686,1.30667941536661,29.2100326477412));
#18158=CARTESIAN_POINT('Ctrl Pts',(1.42434822255959,1.3965769767511,29.2178417766725));
#18159=CARTESIAN_POINT('Ctrl Pts',(1.41525595760601,1.40579005295335,29.2186535514238));
#18160=CARTESIAN_POINT('Ctrl Pts',(1.40165357133843,1.41930746499783,29.2198620728897));
#18161=CARTESIAN_POINT('Ctrl Pts',(1.39721177599965,1.42368032430728,29.2202557908326));
#18162=CARTESIAN_POINT('Ctrl Pts',(1.38928238885809,1.43141379862778,29.2209570617215));
#18163=CARTESIAN_POINT('Ctrl Pts',(1.38580290018288,1.43478268042937,29.221264249796));
#18164=CARTESIAN_POINT('Ctrl Pts',(1.37846608552437,1.44183468462931,29.2219108817663));
#18165=CARTESIAN_POINT('Ctrl Pts',(1.37460619328911,1.4455150705549,29.2222504407349));
#18166=CARTESIAN_POINT('Ctrl Pts',(1.36441447012293,1.45515508637172,29.2231453896666));
#18167=CARTESIAN_POINT('Ctrl Pts',(1.35805840411952,1.4610888195806,29.2237018856157));
#18168=CARTESIAN_POINT('Ctrl Pts',(1.32921678955223,1.48766324307162,29.2262199345689));
#18169=CARTESIAN_POINT('Ctrl Pts',(1.30629910538465,1.50782680502601,29.2282014999488));
#18170=CARTESIAN_POINT('Ctrl Pts',(1.24383269620646,1.56029310964375,29.2335555053475));
#18171=CARTESIAN_POINT('Ctrl Pts',(1.20349329841,1.59161474576416,29.2369651135961));
#18172=CARTESIAN_POINT('Ctrl Pts',(1.08022265222433,1.6799610180319,29.2472421948056));
#18173=CARTESIAN_POINT('Ctrl Pts',(0.994135253928337,1.73229379294682,29.2542466834574));
#18174=CARTESIAN_POINT('Ctrl Pts',(0.796145412018442,1.83301745511139,29.2697453494907));
#18175=CARTESIAN_POINT('Ctrl Pts',(0.682989870473569,1.87811944952291,29.2782169818174));
#18176=CARTESIAN_POINT('Ctrl Pts',(0.559148921622868,1.91479438893901,29.2866497187329));
#18177=CARTESIAN_POINT('Ctrl Pts',(0.551865436926842,1.91690626074134,29.2871426342446));
#18178=CARTESIAN_POINT('Ctrl Pts',(0.541197102529507,1.91993373607495,29.2878600029908));
#18179=CARTESIAN_POINT('Ctrl Pts',(0.53782171038397,1.9208820013229,29.2880862997733));
#18180=CARTESIAN_POINT('Ctrl Pts',(0.531831944999803,1.92254770920063,29.2884866561701));
#18181=CARTESIAN_POINT('Ctrl Pts',(0.529218591041382,1.92326872670535,29.2886609225122));
#18182=CARTESIAN_POINT('Ctrl Pts',(0.526598875463822,1.92398575537491,29.2888351988449));
#18183=CARTESIAN_POINT('Ctrl Pts',(0.526594021266306,1.92398708397222,29.2888355217685));
#18184=CARTESIAN_POINT('Ctrl Pts',(0.526585806943274,1.92398933220484,29.2888360682208));
#18185=CARTESIAN_POINT('Ctrl Pts',(0.526582446839744,1.92399025184443,29.2888362917487));
#18186=CARTESIAN_POINT('Ctrl Pts',(0.526575727171443,1.92399209095724,29.2888367387674));
#18187=CARTESIAN_POINT('Ctrl Pts',(0.526572367517595,1.92399301045483,29.288836962264));
#18188=CARTESIAN_POINT('Ctrl Pts',(0.526565648734988,1.9239948492874,29.288837409221));
#18189=CARTESIAN_POINT('Ctrl Pts',(0.526562289576874,1.9239957686304,29.2888376326834));
#18190=CARTESIAN_POINT('Ctrl Pts',(0.526555571464562,1.92399760724169,29.2888380795931));
#18191=CARTESIAN_POINT('Ctrl Pts',(0.52655221268682,1.92399852646169,29.2888383030288));
#18192=CARTESIAN_POINT('Ctrl Pts',(0.526545495467737,1.9240003647907,29.2888387498763));
#18193=CARTESIAN_POINT('Ctrl Pts',(0.526542137070716,1.9240012838876,29.2888389732853));
#18194=CARTESIAN_POINT('Ctrl Pts',(0.526535420810581,1.92400312191637,29.2888394200664));
#18195=CARTESIAN_POINT('Ctrl Pts',(0.526532062868687,1.92400404086981,29.2888396434437));
#18196=CARTESIAN_POINT('Ctrl Pts',(0.526525347386487,1.92400587864789,29.2888400901704));
#18197=CARTESIAN_POINT('Ctrl Pts',(0.526521989875334,1.92400679746456,29.2888403135177));
#18198=CARTESIAN_POINT('Ctrl Pts',(0.526515275131037,1.92400863500292,29.2888407601925));
#18199=CARTESIAN_POINT('Ctrl Pts',(0.526511917969968,1.92400955370489,29.2888409835152));
#18200=CARTESIAN_POINT('Ctrl Pts',(0.526505204189689,1.92401139094167,29.2888414301232));
#18201=CARTESIAN_POINT('Ctrl Pts',(0.526501847451382,1.92401230950906,29.2888416534164));
#18202=CARTESIAN_POINT('Ctrl Pts',(0.526495134525531,1.92401414647425,29.2888420999648));
#18203=CARTESIAN_POINT('Ctrl Pts',(0.526491778253567,1.92401506489515,29.2888423232257));
#18204=CARTESIAN_POINT('Ctrl Pts',(0.526485066010145,1.92401690163585,29.288842769726));
#18205=CARTESIAN_POINT('Ctrl Pts',(0.526481710127783,1.92401781993126,29.2888429929596));
#18206=CARTESIAN_POINT('Ctrl Pts',(0.526474998730395,1.92401965640269,29.2888434394009));
#18207=CARTESIAN_POINT('Ctrl Pts',(0.526471643256011,1.9240205745676,29.288843662606));
#18208=CARTESIAN_POINT('Ctrl Pts',(0.526464932562657,1.92402241080864,29.2888441089978));
#18209=CARTESIAN_POINT('Ctrl Pts',(0.526461577398764,1.92402332886972,29.2888443321809));
#18210=CARTESIAN_POINT('Ctrl Pts',(0.526454867820843,1.92402516476782,29.2888447784958));
#18211=CARTESIAN_POINT('Ctrl Pts',(0.526451513191697,1.92402608266371,29.2888450016419));
#18212=CARTESIAN_POINT('Ctrl Pts',(0.526444804048318,1.92402791840519,29.2888454479252));
#18213=CARTESIAN_POINT('Ctrl Pts',(0.526441449729462,1.92402883619733,29.2888456710493));
#18214=CARTESIAN_POINT('Ctrl Pts',(0.526434741628938,1.92403067161575,29.2888461172605));
#18215=CARTESIAN_POINT('Ctrl Pts',(0.526431387788079,1.92403158925825,29.2888463403515));
#18216=CARTESIAN_POINT('Ctrl Pts',(0.526424680200753,1.92403342449855,29.2888467865259));
#18217=CARTESIAN_POINT('Ctrl Pts',(0.526421326651363,1.92403434204245,29.2888470095962));
#18218=CARTESIAN_POINT('Ctrl Pts',(0.526414620032519,1.92403617698008,29.2888474557034));
#18219=CARTESIAN_POINT('Ctrl Pts',(0.526411266864753,1.92403709440071,29.2888476787469));
#18220=CARTESIAN_POINT('Ctrl Pts',(0.526404561024508,1.92403892908763,29.2888481247997));
#18221=CARTESIAN_POINT('Ctrl Pts',(0.52640120823694,1.9240398463854,29.2888483478165));
#18222=CARTESIAN_POINT('Ctrl Pts',(0.526394503275733,1.92404168079415,29.2888487938081));
#18223=CARTESIAN_POINT('Ctrl Pts',(0.526391150973658,1.92404259794026,29.2888490167914));
#18224=CARTESIAN_POINT('Ctrl Pts',(0.52638444638585,1.92404443220918,29.2888494627554));
#18225=CARTESIAN_POINT('Ctrl Pts',(0.52638109428231,1.92404534928214,29.2888496857241));
#18226=CARTESIAN_POINT('Ctrl Pts',(0.526374391079874,1.92404718313439,29.2888501315932));
#18227=CARTESIAN_POINT('Ctrl Pts',(0.526371039620971,1.92404810001216,29.2888503545177));
#18228=CARTESIAN_POINT('Ctrl Pts',(0.526364336506501,1.92404993380269,29.2888508003783));
#18229=CARTESIAN_POINT('Ctrl Pts',(0.526360985294928,1.92405085059398,29.288851023285));
#18230=CARTESIAN_POINT('Ctrl Pts',(0.526354283170577,1.924052684076,29.288851469077));
#18231=CARTESIAN_POINT('Ctrl Pts',(0.526350932321706,1.92405360074925,29.2888516919582));
#18232=CARTESIAN_POINT('Ctrl Pts',(0.526344230833431,1.92405543401962,29.2888521377053));
#18233=CARTESIAN_POINT('Ctrl Pts',(0.526340880232287,1.92405635060628,29.2888523605686));
#18234=CARTESIAN_POINT('Ctrl Pts',(0.526334179846777,1.92405818353736,29.2888528062396));
#18235=CARTESIAN_POINT('Ctrl Pts',(0.526330829737993,1.92405909997052,29.2888530290689));
#18236=CARTESIAN_POINT('Ctrl Pts',(0.523444962036975,1.92484853037316,29.2890449791875));
#18237=CARTESIAN_POINT('Ctrl Pts',(0.520560652967708,1.92563057205457,29.2892363261919));
#18238=CARTESIAN_POINT('Ctrl Pts',(0.512941638471936,1.92767799601785,29.2897404855866));
#18239=CARTESIAN_POINT('Ctrl Pts',(0.508203971277021,1.92893242639931,29.2900526682332));
#18240=CARTESIAN_POINT('Ctrl Pts',(0.497653502177141,1.93168439043918,29.2907450552458));
#18241=CARTESIAN_POINT('Ctrl Pts',(0.491838440440571,1.93317317981301,29.2911247740662));
#18242=CARTESIAN_POINT('Ctrl Pts',(0.474350811353059,1.93756639916924,29.2922612418029));
#18243=CARTESIAN_POINT('Ctrl Pts',(0.462658371402987,1.94039158179283,29.2930138074731));
#18244=CARTESIAN_POINT('Ctrl Pts',(0.299897405222967,1.97816377265397,29.3033977192652));
#18245=CARTESIAN_POINT('Ctrl Pts',(0.145259127038876,1.99549110389519,29.3121958439943));
#18246=CARTESIAN_POINT('Ctrl Pts',(-0.137514151733409,1.99409569077006,
29.3286539196592));
#18247=CARTESIAN_POINT('Ctrl Pts',(-0.264809590281865,1.98121090914016,
29.3362014417442));
#18248=CARTESIAN_POINT('Ctrl Pts',(-0.402758096348126,1.95371004751011,
29.3449807793766));
#18249=CARTESIAN_POINT('Ctrl Pts',(-0.415499521244889,1.95104002239023,
29.3457971510764));
#18250=CARTESIAN_POINT('Ctrl Pts',(-0.434315590364653,1.94690435376797,
29.3470112140561));
#18251=CARTESIAN_POINT('Ctrl Pts',(-0.440411125990315,1.94553453668032,
29.347405835616));
#18252=CARTESIAN_POINT('Ctrl Pts',(-0.451222159309834,1.94305162044443,
29.3481081250778));
#18253=CARTESIAN_POINT('Ctrl Pts',(-0.45594024713903,1.9419499290981,29.3484154242786));
#18254=CARTESIAN_POINT('Ctrl Pts',(-0.465836157238374,1.93960114510146,
29.3490616890073));
#18255=CARTESIAN_POINT('Ctrl Pts',(-0.471013085414775,1.93835048428567,
29.3494007673224));
#18256=CARTESIAN_POINT('Ctrl Pts',(-0.484596411258688,1.93501134618326,
29.3502930887589));
#18257=CARTESIAN_POINT('Ctrl Pts',(-0.492994250691818,1.93288883708351,
29.3508474261109));
#18258=CARTESIAN_POINT('Ctrl Pts',(-0.530599777236812,1.92312322612536,
29.3533419188591));
#18259=CARTESIAN_POINT('Ctrl Pts',(-0.559644193068901,1.91487265305356,
29.3553016304287));
#18260=CARTESIAN_POINT('Ctrl Pts',(-0.636546004130525,1.89112834085122,
29.3605824628041));
#18261=CARTESIAN_POINT('Ctrl Pts',(-0.684020968464962,1.87447907879639,
29.3639395134397));
#18262=CARTESIAN_POINT('Ctrl Pts',(-0.877009309647185,1.79849082090125,
29.3779855539883));
#18263=CARTESIAN_POINT('Ctrl Pts',(-1.01588641501043,1.72385612758125,29.3891084312968));
#18264=CARTESIAN_POINT('Ctrl Pts',(-1.15816819419156,1.62417691584422,29.4010730848067));
#18265=CARTESIAN_POINT('Ctrl Pts',(-1.17167120532949,1.61446301603628,29.4022141337267));
#18266=CARTESIAN_POINT('Ctrl Pts',(-1.2254971517718,1.57471026591049,29.4067807582112));
#18267=CARTESIAN_POINT('Ctrl Pts',(-1.26480316879583,1.54331773453885,29.4101574429467));
#18268=CARTESIAN_POINT('Ctrl Pts',(-1.30830599146299,1.50579356562667,29.4139055239344));
#18269=CARTESIAN_POINT('Ctrl Pts',(-1.31370266596423,1.50108765193655,29.4143706782977));
#18270=CARTESIAN_POINT('Ctrl Pts',(-1.32167084967598,1.4940634898813,29.4150576111325));
#18271=CARTESIAN_POINT('Ctrl Pts',(-1.32426177684032,1.49176750652514,29.4152809946002));
#18272=CARTESIAN_POINT('Ctrl Pts',(-1.32886183630325,1.48766967620366,29.4156776171537));
#18273=CARTESIAN_POINT('Ctrl Pts',(-1.33087329673132,1.48587049026725,29.4158510523132));
#18274=CARTESIAN_POINT('Ctrl Pts',(-1.33476567303237,1.48237464117745,29.4161866716514));
#18275=CARTESIAN_POINT('Ctrl Pts',(-1.33664699623711,1.48067848851036,29.4163488923398));
#18276=CARTESIAN_POINT('Ctrl Pts',(-1.34196330440937,1.47586705228716,29.4168073298297));
#18277=CARTESIAN_POINT('Ctrl Pts',(-1.3453906930421,1.47274334170204,29.4171029154284));
#18278=CARTESIAN_POINT('Ctrl Pts',(-1.35975657592307,1.45955832188375,29.4183421626729));
#18279=CARTESIAN_POINT('Ctrl Pts',(-1.37059369238887,1.44938656079903,29.4192777465109));
#18280=CARTESIAN_POINT('Ctrl Pts',(-1.39889776274354,1.42221886229217,29.4217265184902));
#18281=CARTESIAN_POINT('Ctrl Pts',(-1.41616916638921,1.40502186804519,29.423226181648));
#18282=CARTESIAN_POINT('Ctrl Pts',(-1.48724150274162,1.33161325546986,29.4294430938483));
#18283=CARTESIAN_POINT('Ctrl Pts',(-1.53804898580005,1.27259124628305,29.434002331739));
#18284=CARTESIAN_POINT('Ctrl Pts',(-1.69063016584929,1.07281037687863,29.4486235896082));
#18285=CARTESIAN_POINT('Ctrl Pts',(-1.77751339314154,0.921733095427336,
29.4585617250565));
#18286=CARTESIAN_POINT('Ctrl Pts',(-1.85148388442406,0.742593858594666,
29.4705631289605));
#18287=CARTESIAN_POINT('Ctrl Pts',(-1.85893201674481,0.723747140169397,
29.4718270808956));
#18288=CARTESIAN_POINT('Ctrl Pts',(-1.86881432579185,0.697581511353945,
29.4735850218788));
#18289=CARTESIAN_POINT('Ctrl Pts',(-1.87149529970507,0.69035663953955,29.4740707513966));
#18290=CARTESIAN_POINT('Ctrl Pts',(-1.87571106679072,0.678790656576213,
29.4748489253556));
#18291=CARTESIAN_POINT('Ctrl Pts',(-1.87727282945137,0.674459401861553,
29.4751404692842));
#18292=CARTESIAN_POINT('Ctrl Pts',(-1.88045569981373,0.665535606017815,
29.4757414333433));
#18293=CARTESIAN_POINT('Ctrl Pts',(-1.88207501034069,0.660942460883671,
29.4760509108131));
#18294=CARTESIAN_POINT('Ctrl Pts',(-1.88579229141064,0.650274024335524,
29.4767701154539));
#18295=CARTESIAN_POINT('Ctrl Pts',(-1.88787774294877,0.6441944575584,29.4771802540189));
#18296=CARTESIAN_POINT('Ctrl Pts',(-1.89439904545617,0.624879720646166,
29.4784842406023));
#18297=CARTESIAN_POINT('Ctrl Pts',(-1.89872529447193,0.611608247459151,
29.4793816888355));
#18298=CARTESIAN_POINT('Ctrl Pts',(-1.94370667663957,0.468541821870589,
29.4890736027176));
#18299=CARTESIAN_POINT('Ctrl Pts',(-1.9711160912107,0.334985082796009,29.4983125905171));
#18300=CARTESIAN_POINT('Ctrl Pts',(-1.99145641015902,0.132836524806506,
29.5124297477425));
#18301=CARTESIAN_POINT('Ctrl Pts',(-1.99480094638918,0.0656729622107595,
29.5171344356621));
#18302=CARTESIAN_POINT('Ctrl Pts',(-1.9947494135177,-0.00152963093166499,
29.5218050102941));
#18303=CARTESIAN_POINT('',(-1.99474949650966,0.00141727712894259,30.3209548813952));
#18304=CARTESIAN_POINT('Ctrl Pts',(-1.99474936733483,-0.00158871561299351,
29.5209548813952));
#18305=CARTESIAN_POINT('Ctrl Pts',(-1.99466579522125,-0.106519654372253,
29.5276724214068));
#18306=CARTESIAN_POINT('Ctrl Pts',(-1.98630072391948,-0.211129095682814,
29.5343899614184));
#18307=CARTESIAN_POINT('Ctrl Pts',(-1.96981585838482,-0.314409043374509,
29.54110750143));
#18308=CARTESIAN_POINT('Ctrl Pts',(-1.95888563255435,-0.382888410079444,
29.545561540148));
#18309=CARTESIAN_POINT('Ctrl Pts',(-1.94435854313491,-0.450932742343483,
29.550015578866));
#18310=CARTESIAN_POINT('Ctrl Pts',(-1.92628229647851,-0.518135191599125,
29.554469617584));
#18311=CARTESIAN_POINT('Ctrl Pts',(-1.90823322122938,-0.585236625132148,
29.5589169611897));
#18312=CARTESIAN_POINT('Ctrl Pts',(-1.88664570339129,-0.651498218418248,
29.5633643047955));
#18313=CARTESIAN_POINT('Ctrl Pts',(-1.86161877916089,-0.716521516477704,
29.5678116484013));
#18314=CARTESIAN_POINT('Ctrl Pts',(-1.83662135910167,-0.781468158752438,
29.572253749046));
#18315=CARTESIAN_POINT('Ctrl Pts',(-1.80819276081117,-0.84517895051031,
29.5766958496908));
#18316=CARTESIAN_POINT('Ctrl Pts',(-1.77648181383497,-0.907270592278627,
29.5811379503356));
#18317=CARTESIAN_POINT('Ctrl Pts',(-1.74479087026461,-0.969323066364258,
29.5855772488836));
#18318=CARTESIAN_POINT('Ctrl Pts',(-1.70982190759389,-1.02975798163676,
29.5900165474316));
#18319=CARTESIAN_POINT('Ctrl Pts',(-1.67177123838613,-1.08821343908487,
29.5944558459797));
#18320=CARTESIAN_POINT('Ctrl Pts',(-1.63373164200094,-1.14665188587529,
29.5988938526827));
#18321=CARTESIAN_POINT('Ctrl Pts',(-1.59261238627219,-1.20311160826029,
29.6033318593858));
#18322=CARTESIAN_POINT('Ctrl Pts',(-1.54865403648486,-1.25725822239472,
29.6077698660888));
#18323=CARTESIAN_POINT('Ctrl Pts',(-1.50469354195092,-1.31140747836554,
29.6122080893241));
#18324=CARTESIAN_POINT('Ctrl Pts',(-1.45789398876281,-1.36324302345215,
29.6166463125594));
#18325=CARTESIAN_POINT('Ctrl Pts',(-1.40853616203275,-1.41246360758289,
29.6210845357947));
#18326=CARTESIAN_POINT('Ctrl Pts',(-1.35912604613227,-1.46173633549065,
29.6255274608378));
#18327=CARTESIAN_POINT('Ctrl Pts',(-1.30715259458788,-1.50838822675202,
29.6299703858808));
#18328=CARTESIAN_POINT('Ctrl Pts',(-1.25293270040905,-1.55215566575833,
29.6344133109238));
#18329=CARTESIAN_POINT('Ctrl Pts',(-1.19868115584625,-1.59594865362029,
29.6388588294851));
#18330=CARTESIAN_POINT('Ctrl Pts',(-1.14218095524136,-1.63685355069029,
29.6433043480463));
#18331=CARTESIAN_POINT('Ctrl Pts',(-1.08377898084886,-1.67464942097449,
29.6477498666076));
#18332=CARTESIAN_POINT('Ctrl Pts',(-1.02527509338074,-1.71251124610742,
29.6522031427228));
#18333=CARTESIAN_POINT('Ctrl Pts',(-0.964863231852163,-1.74725297047359,
29.656656418838));
#18334=CARTESIAN_POINT('Ctrl Pts',(-0.902915217312026,-1.7786994329696,
29.6611096949532));
#18335=CARTESIAN_POINT('Ctrl Pts',(-0.869743836950932,-1.79553810933735,
29.6634942962511));
#18336=CARTESIAN_POINT('Ctrl Pts',(-0.83613235041454,-1.81143275734089,
29.6658788975489));
#18337=CARTESIAN_POINT('Ctrl Pts',(-0.802139872537429,-1.82636228262238,
29.6682634988468));
#18338=CARTESIAN_POINT('Ctrl Pts',(-0.738647576059334,-1.85424815339875,
29.6727175375648));
#18339=CARTESIAN_POINT('Ctrl Pts',(-0.673573653503056,-1.8788744012535,
29.6771715762827));
#18340=CARTESIAN_POINT('Ctrl Pts',(-0.607285994646577,-1.90006086302679,
29.6816256150007));
#18341=CARTESIAN_POINT('Ctrl Pts',(-0.541097976440631,-1.92121547825625,
29.6860729586065));
#18342=CARTESIAN_POINT('Ctrl Pts',(-0.473700305504764,-1.93894042180044,
29.6905203022122));
#18343=CARTESIAN_POINT('Ctrl Pts',(-0.405481605230866,-1.95310323084045,
29.694967645818));
#18344=CARTESIAN_POINT('Ctrl Pts',(-0.337343327792411,-1.96724934338439,
29.6994097464628));
#18345=CARTESIAN_POINT('Ctrl Pts',(-0.268386420431636,-1.97784156290728,
29.7038518471076));
#18346=CARTESIAN_POINT('Ctrl Pts',(-0.199013723142859,-1.98479749609395,
29.7082939477524));
#18347=CARTESIAN_POINT('Ctrl Pts',(-0.129684786458864,-1.99174904144715,
29.7127332463004));
#18348=CARTESIAN_POINT('Ctrl Pts',(-0.0599410661421116,-1.99506880207736,
29.7171725448484));
#18349=CARTESIAN_POINT('Ctrl Pts',(0.00980688254372123,-1.9947258928371,
29.7216118433964));
#18350=CARTESIAN_POINT('Ctrl Pts',(0.0795345344338355,-1.99438308338414,
29.7260498500995));
#18351=CARTESIAN_POINT('Ctrl Pts',(0.149265922945748,-1.99037972233577,
29.7304878568026));
#18352=CARTESIAN_POINT('Ctrl Pts',(0.218589667450933,-1.98273702739009,
29.7349258635056));
#18353=CARTESIAN_POINT('Ctrl Pts',(0.28791679429119,-1.97509395955407,29.7393640867409));
#18354=CARTESIAN_POINT('Ctrl Pts',(0.356835751287597,-1.96381126131426,
29.7438023099762));
#18355=CARTESIAN_POINT('Ctrl Pts',(0.424941239790018,-1.94896190450858,
29.7482405332115));
#18356=CARTESIAN_POINT('Ctrl Pts',(0.493118878541495,-1.93409681644812,
29.7526834582546));
#18357=CARTESIAN_POINT('Ctrl Pts',(0.560480849449957,-1.91565763265303,
29.7571263832976));
#18358=CARTESIAN_POINT('Ctrl Pts',(0.626633946079841,-1.89376805869156,
29.7615693083406));
#18359=CARTESIAN_POINT('Ctrl Pts',(0.692825658995164,-1.87186570688478,
29.7660148269019));
#18360=CARTESIAN_POINT('Ctrl Pts',(0.757806636869767,-1.84650913402551,
29.7704603454631));
#18361=CARTESIAN_POINT('Ctrl Pts',(0.821203319942807,-1.81787036661444,
29.7749058640244));
#18362=CARTESIAN_POINT('Ctrl Pts',(0.884710631997507,-1.7891816237548,29.7793591401396));
#18363=CARTESIAN_POINT('Ctrl Pts',(0.946627695619021,-1.75719947783284,
29.7838124162549));
#18364=CARTESIAN_POINT('Ctrl Pts',(1.00660593447129,-1.72214170589623,29.7882656923701));
#18365=CARTESIAN_POINT('Ctrl Pts',(1.03872255659511,-1.70336927717314,29.7906502936679));
#18366=CARTESIAN_POINT('Ctrl Pts',(1.0702837584668,-1.6837157177325,29.7930348949657));
#18367=CARTESIAN_POINT('Ctrl Pts',(1.10123979937458,-1.663219308081,29.7954194962635));
#18368=CARTESIAN_POINT('Ctrl Pts',(1.15906053648768,-1.62493542295007,29.7998735349814));
#18369=CARTESIAN_POINT('Ctrl Pts',(1.21499703220259,-1.58355697533055,29.8043275736994));
#18370=CARTESIAN_POINT('Ctrl Pts',(1.26869863310333,-1.53929572885191,29.8087816124174));
#18371=CARTESIAN_POINT('Ctrl Pts',(1.32231951215414,-1.49510101390373,29.8132289560232));
#18372=CARTESIAN_POINT('Ctrl Pts',(1.37371178925215,-1.44803240944277,29.8176762996289));
#18373=CARTESIAN_POINT('Ctrl Pts',(1.42255368997764,-1.39834493657001,29.8221236432347));
#18374=CARTESIAN_POINT('Ctrl Pts',(1.47133801112264,-1.3487160401204,29.8265657438795));
#18375=CARTESIAN_POINT('Ctrl Pts',(1.51757758591197,-1.2964747546224,29.8310078445243));
#18376=CARTESIAN_POINT('Ctrl Pts',(1.56098503920093,-1.2419151621149,29.8354499451691));
#18377=CARTESIAN_POINT('Ctrl Pts',(1.60436511087606,-1.18738998604005,29.8398892437171));
#18378=CARTESIAN_POINT('Ctrl Pts',(1.64491630099581,-1.13054978623273,29.8443285422651));
#18379=CARTESIAN_POINT('Ctrl Pts',(1.68239036315675,-1.07172301853478,29.8487678408131));
#18380=CARTESIAN_POINT('Ctrl Pts',(1.71985352028893,-1.01291336954658,29.8532058475162));
#18381=CARTESIAN_POINT('Ctrl Pts',(1.75424106418017,-0.952118712967176,
29.8576438542193));
#18382=CARTESIAN_POINT('Ctrl Pts',(1.78534810742408,-0.889696407667943,
29.8620818609223));
#18383=CARTESIAN_POINT('Ctrl Pts',(1.81645666839392,-0.827271056757785,
29.8665200841576));
#18384=CARTESIAN_POINT('Ctrl Pts',(1.84428419473193,-0.763218338697194,
29.8709583073929));
#18385=CARTESIAN_POINT('Ctrl Pts',(1.86867260456926,-0.697918519192841,
29.8753965306283));
#18386=CARTESIAN_POINT('Ctrl Pts',(1.89308685123536,-0.63254952173609,29.8798394556713));
#18387=CARTESIAN_POINT('Ctrl Pts',(1.91405453779159,-0.565931245383549,
29.8842823807143));
#18388=CARTESIAN_POINT('Ctrl Pts',(1.93146678400278,-0.498461257064151,
29.8887253057573));
#18389=CARTESIAN_POINT('Ctrl Pts',(1.94888919445878,-0.430951883735447,
29.8931708243186));
#18390=CARTESIAN_POINT('Ctrl Pts',(1.96275193628476,-0.362590288802527,
29.8976163428798));
#18391=CARTESIAN_POINT('Ctrl Pts',(1.97299739237546,-0.293783682629998,
29.9020618614411));
#18392=CARTESIAN_POINT('Ctrl Pts',(1.98326072707303,-0.224857007008966,
29.9065151375563));
#18393=CARTESIAN_POINT('Ctrl Pts',(1.98989412902908,-0.155484257288521,
29.9109684136716));
#18394=CARTESIAN_POINT('Ctrl Pts',(1.99289197257705,-0.0860764087190482,
29.9154216897868));
#18395=CARTESIAN_POINT('Ctrl Pts',(1.99449723158865,-0.0489105017563579,
29.9178062910846));
#18396=CARTESIAN_POINT('Ctrl Pts',(1.99506096221642,-0.0117345139403332,
29.9201908923825));
#18397=CARTESIAN_POINT('Ctrl Pts',(1.99458841887372,0.025389009331597,29.9225754936803));
#18398=CARTESIAN_POINT('Ctrl Pts',(1.99370578648303,0.0947295779843875,
29.9270295323983));
#18399=CARTESIAN_POINT('Ctrl Pts',(1.98920122678504,0.164161389297369,29.9314835711163));
#18400=CARTESIAN_POINT('Ctrl Pts',(1.9810629337309,0.233274977435445,29.9359376098343));
#18401=CARTESIAN_POINT('Ctrl Pts',(1.97293687379569,0.302284677112187,29.94038495344));
#18402=CARTESIAN_POINT('Ctrl Pts',(1.96118797813399,0.370976620758892,29.9448322970458));
#18403=CARTESIAN_POINT('Ctrl Pts',(1.94585644517227,0.438942202666316,29.9492796406515));
#18404=CARTESIAN_POINT('Ctrl Pts',(1.93054298651197,0.506827660138852,29.9537217412963));
#18405=CARTESIAN_POINT('Ctrl Pts',(1.911655386283,0.573987981347018,29.9581638419411));
#18406=CARTESIAN_POINT('Ctrl Pts',(1.88928530786421,0.640022333976274,29.9626059425859));
#18407=CARTESIAN_POINT('Ctrl Pts',(1.86692934058998,0.706015031843367,29.9670452411339));
#18408=CARTESIAN_POINT('Ctrl Pts',(1.84109540971041,0.770882707534618,29.971484539682));
#18409=CARTESIAN_POINT('Ctrl Pts',(1.81192526340182,0.834238816134948,29.97592383823));
#18410=CARTESIAN_POINT('Ctrl Pts',(1.78276360566548,0.89757648797808,29.9803618449331));
#18411=CARTESIAN_POINT('Ctrl Pts',(1.75026786441981,0.959403021476149,29.9847998516361));
#18412=CARTESIAN_POINT('Ctrl Pts',(1.71462756335534,1.01935267767447,29.9892378583392));
#18413=CARTESIAN_POINT('Ctrl Pts',(1.6789855233854,1.07930525884206,29.9936760815745));
#18414=CARTESIAN_POINT('Ctrl Pts',(1.64019887122271,1.13738036131342,29.9981143048098));
#18415=CARTESIAN_POINT('Ctrl Pts',(1.59850173072441,1.19323919620966,30.0025525280451));
#18416=CARTESIAN_POINT('Ctrl Pts',(1.55676041670735,1.24915720737701,30.0069954530881));
#18417=CARTESIAN_POINT('Ctrl Pts',(1.5121027535873,1.30285387159713,30.0114383781312));
#18418=CARTESIAN_POINT('Ctrl Pts',(1.46480404970151,1.35402239954813,30.0158813031742));
#18419=CARTESIAN_POINT('Ctrl Pts',(1.4174777356154,1.40522079667502,30.0203268217355));
#18420=CARTESIAN_POINT('Ctrl Pts',(1.36750766303851,1.45388777849408,30.0247723402967));
#18421=CARTESIAN_POINT('Ctrl Pts',(1.315205002565,1.49975443447519,30.029217858858));
#18422=CARTESIAN_POINT('Ctrl Pts',(1.26281107248893,1.54570112905136,30.0336711349732));
#18423=CARTESIAN_POINT('Ctrl Pts',(1.20807681366987,1.58883744016883,30.0381244110884));
#18424=CARTESIAN_POINT('Ctrl Pts',(1.15134471083882,1.62893613113697,30.0425776872037));
#18425=CARTESIAN_POINT('Ctrl Pts',(1.12096630120605,1.6504078270407,30.0449622885015));
#18426=CARTESIAN_POINT('Ctrl Pts',(1.0900155202146,1.67100930801374,30.0473468897992));
#18427=CARTESIAN_POINT('Ctrl Pts',(1.05854779817953,1.69071112892454,30.049731491097));
#18428=CARTESIAN_POINT('Ctrl Pts',(0.999771325801679,1.72751085441041,30.054185529815));
#18429=CARTESIAN_POINT('Ctrl Pts',(0.938957186119689,1.76131481712195,30.058639568533));
#18430=CARTESIAN_POINT('Ctrl Pts',(0.876443248680132,1.79189140138096,30.063093607251));
#18431=CARTESIAN_POINT('Ctrl Pts',(0.814023279401504,1.82242202428306,30.0675409508567));
#18432=CARTESIAN_POINT('Ctrl Pts',(0.749909019715537,1.84973468391449,30.0719882944625));
#18433=CARTESIAN_POINT('Ctrl Pts',(0.684465771850529,1.87364195343322,30.0764356380682));
#18434=CARTESIAN_POINT('Ctrl Pts',(0.619099674847843,1.89752103873862,30.080877738713));
#18435=CARTESIAN_POINT('Ctrl Pts',(0.552408159028457,1.91800254026798,30.0853198393578));
#18436=CARTESIAN_POINT('Ctrl Pts',(0.484777854815494,1.93494650933314,30.0897619400026));
#18437=CARTESIAN_POINT('Ctrl Pts',(0.417190212098042,1.95187979006755,30.0942012385506));
#18438=CARTESIAN_POINT('Ctrl Pts',(0.348665429541026,1.96527984640244,30.0986405370986));
#18439=CARTESIAN_POINT('Ctrl Pts',(0.279605241831666,1.97505657418725,30.1030798356467));
#18440=CARTESIAN_POINT('Ctrl Pts',(0.210565150778193,1.98483045692426,30.1075178423497));
#18441=CARTESIAN_POINT('Ctrl Pts',(0.140990448347648,1.9909830356668,30.1119558490528));
#18442=CARTESIAN_POINT('Ctrl Pts',(0.071291242688871,1.99347563848066,30.1163938557558));
#18443=CARTESIAN_POINT('Ctrl Pts',(0.00158863637605586,1.99596836290968,
30.1208320789912));
#18444=CARTESIAN_POINT('Ctrl Pts',(-0.0682379958922396,1.99480074177305,
30.1252703022265));
#18445=CARTESIAN_POINT('Ctrl Pts',(-0.137777057387593,1.9899861921525,30.1297085254618));
#18446=CARTESIAN_POINT('Ctrl Pts',(-0.207389787844344,1.98516654204796,
30.1341514505048));
#18447=CARTESIAN_POINT('Ctrl Pts',(-0.276713850096724,1.97669228594301,
30.1385943755478));
#18448=CARTESIAN_POINT('Ctrl Pts',(-0.345342253519151,1.96462879202009,
30.1430373005909));
#18449=CARTESIAN_POINT('Ctrl Pts',(-0.414010718165479,1.95255825613922,
30.1474828191521));
#18450=CARTESIAN_POINT('Ctrl Pts',(-0.481982238513912,1.93689442218222,
30.1519283377134));
#18451=CARTESIAN_POINT('Ctrl Pts',(-0.548862254567311,1.91775331782044,
30.1563738562746));
#18452=CARTESIAN_POINT('Ctrl Pts',(-0.615858978115655,1.89857881169722,
30.1608271323898));
#18453=CARTESIAN_POINT('Ctrl Pts',(-0.681759932334584,1.87591508167937,
30.1652804085051));
#18454=CARTESIAN_POINT('Ctrl Pts',(-0.746188640976332,1.84992704574475,
30.1697336846203));
#18455=CARTESIAN_POINT('Ctrl Pts',(-0.780688361691636,1.83601119983405,
30.1721182859181));
#18456=CARTESIAN_POINT('Ctrl Pts',(-0.814766331291456,1.82114298372511,
30.174502887216));
#18457=CARTESIAN_POINT('Ctrl Pts',(-0.848367782930703,1.80535305892926,
30.1768874885138));
#18458=CARTESIAN_POINT('Ctrl Pts',(-0.911129707416232,1.77586010492511,
30.1813415272318));
#18459=CARTESIAN_POINT('Ctrl Pts',(-0.972476139029651,1.7430320253504,30.1857955659497));
#18460=CARTESIAN_POINT('Ctrl Pts',(-1.03202941857197,1.70702748709621,30.1902496046677));
#18461=CARTESIAN_POINT('Ctrl Pts',(-1.09149318028213,1.67107706925717,30.1946969482735));
#18462=CARTESIAN_POINT('Ctrl Pts',(-1.14916872406153,1.63195992057579,30.1991442918792));
#18463=CARTESIAN_POINT('Ctrl Pts',(-1.20470069042879,1.58988169653607,30.203591635485));
#18464=CARTESIAN_POINT('Ctrl Pts',(-1.26016719031588,1.54785307839722,30.2080337361298));
#18465=CARTESIAN_POINT('Ctrl Pts',(-1.31349474353205,1.50287061231141,30.2124758367746));
#18466=CARTESIAN_POINT('Ctrl Pts',(-1.3643563608736,1.45518359083785,30.2169179374193));
#18467=CARTESIAN_POINT('Ctrl Pts',(-1.41518589448164,1.40752665054867,30.2213572359674));
#18468=CARTESIAN_POINT('Ctrl Pts',(-1.46355222170617,1.35716887334317,30.2257965345154));
#18469=CARTESIAN_POINT('Ctrl Pts',(-1.50916208288596,1.30439923722735,30.2302358330634));
#18470=CARTESIAN_POINT('Ctrl Pts',(-1.55475867150285,1.25164495718359,30.2346738397665));
#18471=CARTESIAN_POINT('Ctrl Pts',(-1.59760006647602,1.19648058172043,30.2391118464695));
#18472=CARTESIAN_POINT('Ctrl Pts',(-1.63743171667576,1.13922997490598,30.2435498531726));
#18473=CARTESIAN_POINT('Ctrl Pts',(-1.67726531027866,1.08197657481006,30.2479880764079));
#18474=CARTESIAN_POINT('Ctrl Pts',(-1.71408858993195,1.02263714450766,30.2524262996432));
#18475=CARTESIAN_POINT('Ctrl Pts',(-1.74768999280331,0.961565001211662,
30.2568645228785));
#18476=CARTESIAN_POINT('Ctrl Pts',(-1.78132699265284,0.900428158719596,
30.2613074479216));
#18477=CARTESIAN_POINT('Ctrl Pts',(-1.8117350666283,0.837555369209269,30.2657503729646));
#18478=CARTESIAN_POINT('Ctrl Pts',(-1.83874882397477,0.773324204219296,
30.2701932980076));
#18479=CARTESIAN_POINT('Ctrl Pts',(-1.86577835036331,0.70905554485449,30.2746388165689));
#18480=CARTESIAN_POINT('Ctrl Pts',(-1.88940945046268,0.643427392505011,
30.2790843351301));
#18481=CARTESIAN_POINT('Ctrl Pts',(-1.90952605595385,0.576834295212516,
30.2835298536914));
#18482=CARTESIAN_POINT('Ctrl Pts',(-1.92967776548315,0.510124991106323,
30.2879831298066));
#18483=CARTESIAN_POINT('Ctrl Pts',(-1.94630262127761,0.44244785615585,30.2924364059218));
#18484=CARTESIAN_POINT('Ctrl Pts',(-1.95933545066732,0.374208704145551,
30.2968896820371));
#18485=CARTESIAN_POINT('Ctrl Pts',(-1.96631415602319,0.337668600582921,
30.2992742833349));
#18486=CARTESIAN_POINT('Ctrl Pts',(-1.97226380792002,0.300967462935943,
30.3016588846326));
#18487=CARTESIAN_POINT('Ctrl Pts',(-1.97718053383544,0.264167937347107,
30.3040434859304));
#18488=CARTESIAN_POINT('Ctrl Pts',(-1.98880353854548,0.177174871920036,
30.309680617752));
#18489=CARTESIAN_POINT('Ctrl Pts',(-1.99468698571734,0.0893982153310911,
30.3153177495736));
#18490=CARTESIAN_POINT('Ctrl Pts',(-1.99474949650966,0.00141727712894259,
30.3209548813952));
#18491=CARTESIAN_POINT('',(-1.99474901027189,-0.00181008235116998,31.9203783954114));
#18492=CARTESIAN_POINT('Ctrl Pts',(-1.994749448555,0.00148323617099721,
30.3220724695856));
#18493=CARTESIAN_POINT('Ctrl Pts',(-1.99486339498652,-0.151759103715625,
30.3311167672701));
#18494=CARTESIAN_POINT('Ctrl Pts',(-1.97731920438673,-0.304509772329282,
30.3397836599352));
#18495=CARTESIAN_POINT('Ctrl Pts',(-1.93170678897217,-0.499769147293737,
30.3517403697977));
#18496=CARTESIAN_POINT('Ctrl Pts',(-1.91932723631203,-0.545383159862958,
30.3545948799917));
#18497=CARTESIAN_POINT('Ctrl Pts',(-1.89969508734825,-0.608728035408092,
30.3586714187028));
#18498=CARTESIAN_POINT('Ctrl Pts',(-1.89378881198397,-0.62686134308302,
30.359851501595));
#18499=CARTESIAN_POINT('Ctrl Pts',(-1.88298687396782,-0.658478308137421,
30.3619337530981));
#18500=CARTESIAN_POINT('Ctrl Pts',(-1.87820400918912,-0.671999205833263,
30.3628322232345));
#18501=CARTESIAN_POINT('Ctrl Pts',(-1.87104275201591,-0.691569817744031,
30.364144836028));
#18502=CARTESIAN_POINT('Ctrl Pts',(-1.86877985749518,-0.697661547803978,
30.3645551329124));
#18503=CARTESIAN_POINT('Ctrl Pts',(-1.86476516292163,-0.708309449584588,
30.3652753665149));
#18504=CARTESIAN_POINT('Ctrl Pts',(-1.86302632129088,-0.712870475402617,
30.3655848675377));
#18505=CARTESIAN_POINT('Ctrl Pts',(-1.85962237571779,-0.721701592300385,
30.3661860676579));
#18506=CARTESIAN_POINT('Ctrl Pts',(-1.85795926001988,-0.725972421051901,
30.3664776983657));
#18507=CARTESIAN_POINT('Ctrl Pts',(-1.85350030155023,-0.737307202484019,
30.3672540581546));
#18508=CARTESIAN_POINT('Ctrl Pts',(-1.85067881829888,-0.744360925583806,
30.3677396486224));
#18509=CARTESIAN_POINT('Ctrl Pts',(-1.84044782789998,-0.769520684348089,
30.3694806031659));
#18510=CARTESIAN_POINT('Ctrl Pts',(-1.83281253926961,-0.78753313669766,
30.3707435783314));
#18511=CARTESIAN_POINT('Ctrl Pts',(-1.75159838836013,-0.971545216472034,
30.3838216678952));
#18512=CARTESIAN_POINT('Ctrl Pts',(-1.65595850478544,-1.12684049535055,
30.396458586788));
#18513=CARTESIAN_POINT('Ctrl Pts',(-1.49613467506367,-1.32118362177827,
30.4139916377149));
#18514=CARTESIAN_POINT('Ctrl Pts',(-1.44876431476313,-1.37296337027864,
30.4188527721933));
#18515=CARTESIAN_POINT('Ctrl Pts',(-1.38108385926314,-1.4395311006474,30.4252648687568));
#18516=CARTESIAN_POINT('Ctrl Pts',(-1.36308196423649,-1.45658851365651,
30.4269235183857));
#18517=CARTESIAN_POINT('Ctrl Pts',(-1.33363276270172,-1.48346837601047,
30.4295563417819));
#18518=CARTESIAN_POINT('Ctrl Pts',(-1.32238446779618,-1.49350397425057,
30.4305437666554));
#18519=CARTESIAN_POINT('Ctrl Pts',(-1.30751815263498,-1.50646787860957,
30.4318239776783));
#18520=CARTESIAN_POINT('Ctrl Pts',(-1.30400249660119,-1.50951206642114,
30.4321249405963));
#18521=CARTESIAN_POINT('Ctrl Pts',(-1.29855487980258,-1.51419589449613,
30.4325884948834));
#18522=CARTESIAN_POINT('Ctrl Pts',(-1.29663041669918,-1.5158441692452,30.4327517174545));
#18523=CARTESIAN_POINT('Ctrl Pts',(-1.29265032105877,-1.51923993799457,
30.4330881734918));
#18524=CARTESIAN_POINT('Ctrl Pts',(-1.29059430903508,-1.52098690702118,
30.4332613650642));
#18525=CARTESIAN_POINT('Ctrl Pts',(-1.28589753409171,-1.52496132051165,
30.4336556194801));
#18526=CARTESIAN_POINT('Ctrl Pts',(-1.28325453054251,-1.5271860749503,30.4338764839836));
#18527=CARTESIAN_POINT('Ctrl Pts',(-1.27636353039978,-1.53295607062898,
30.4344497974799));
#18528=CARTESIAN_POINT('Ctrl Pts',(-1.27210650360312,-1.53649055364581,
30.434801474389));
#18529=CARTESIAN_POINT('Ctrl Pts',(-1.24521294785643,-1.55863108785729,
30.4370079128167));
#18530=CARTESIAN_POINT('Ctrl Pts',(-1.22218205700449,-1.57675533706004,
30.4388296970858));
#18531=CARTESIAN_POINT('Ctrl Pts',(-1.1128894596893,-1.65892931781301,30.4472084576566));
#18532=CARTESIAN_POINT('Ctrl Pts',(-1.02193505155617,-1.71645656980635,
30.4534330831218));
#18533=CARTESIAN_POINT('Ctrl Pts',(-0.849168405902545,-1.80710335158789,
30.4647488712847));
#18534=CARTESIAN_POINT('Ctrl Pts',(-0.768958918600692,-1.84266400643804,
30.4698246504608));
#18535=CARTESIAN_POINT('Ctrl Pts',(-0.638721543276217,-1.89041555838437,
30.4780696528934));
#18536=CARTESIAN_POINT('Ctrl Pts',(-0.590113963383805,-1.90614823789107,
30.4811464465909));
#18537=CARTESIAN_POINT('Ctrl Pts',(-0.511572290956982,-1.92827733384457,
30.4861552193534));
#18538=CARTESIAN_POINT('Ctrl Pts',(-0.482000855644467,-1.93588085954542,
30.488049120221));
#18539=CARTESIAN_POINT('Ctrl Pts',(-0.443798081162261,-1.94477413826615,
30.490510713536));
#18540=CARTESIAN_POINT('Ctrl Pts',(-0.435315694382959,-1.94669037807191,
30.4910582043222));
#18541=CARTESIAN_POINT('Ctrl Pts',(-0.421611186598649,-1.94969228751494,
30.49194435614));
#18542=CARTESIAN_POINT('Ctrl Pts',(-0.416396703231105,-1.95081259820036,
30.4922819045187));
#18543=CARTESIAN_POINT('Ctrl Pts',(-0.406438702614553,-1.95291028966642,
30.49292725146));
#18544=CARTESIAN_POINT('Ctrl Pts',(-0.401695989322101,-1.95389133524634,
30.493234930201));
#18545=CARTESIAN_POINT('Ctrl Pts',(-0.390841669741732,-1.95609539621993,
30.4939398424017));
#18546=CARTESIAN_POINT('Ctrl Pts',(-0.384727833572551,-1.95730705371852,
30.4943374355564));
#18547=CARTESIAN_POINT('Ctrl Pts',(-0.365901448791162,-1.96094650490501,
30.4955634709181));
#18548=CARTESIAN_POINT('Ctrl Pts',(-0.353171071807441,-1.96327920740757,
30.4963949303834));
#18549=CARTESIAN_POINT('Ctrl Pts',(-0.230003854588047,-1.98461155955905,
30.5044639779534));
#18550=CARTESIAN_POINT('Ctrl Pts',(-0.118193260868712,-1.99439398798779,
30.5119972909011));
#18551=CARTESIAN_POINT('Ctrl Pts',(0.165010467986752,-1.9952698910346,30.5315249135389));
#18552=CARTESIAN_POINT('Ctrl Pts',(0.335543026691079,-1.97376359847848,
30.5437336824178));
#18553=CARTESIAN_POINT('Ctrl Pts',(0.512698639338938,-1.92777278888097,
30.5558598579801));
#18554=CARTESIAN_POINT('Ctrl Pts',(0.524135297764521,-1.92469478762665,
30.556639783861));
#18555=CARTESIAN_POINT('Ctrl Pts',(0.541261978256587,-1.91992142189045,
30.5578026825184));
#18556=CARTESIAN_POINT('Ctrl Pts',(0.546972725007384,-1.9183022795032,30.5581895924199));
#18557=CARTESIAN_POINT('Ctrl Pts',(0.557253096091754,-1.91533789152785,
30.5588844621814));
#18558=CARTESIAN_POINT('Ctrl Pts',(0.561825263686943,-1.91400173094101,
30.5591929178396));
#18559=CARTESIAN_POINT('Ctrl Pts',(0.569270786304491,-1.91179688889727,
30.5596942150529));
#18560=CARTESIAN_POINT('Ctrl Pts',(0.57214701044523,-1.91093808671764,30.5598876221662));
#18561=CARTESIAN_POINT('Ctrl Pts',(0.577607769266245,-1.90929414272724,
30.5602543413023));
#18562=CARTESIAN_POINT('Ctrl Pts',(0.580192616621806,-1.90851025312674,
30.5604277205826));
#18563=CARTESIAN_POINT('Ctrl Pts',(0.586108382582246,-1.90670308860113,
30.5608240571881));
#18564=CARTESIAN_POINT('Ctrl Pts',(0.589438211649311,-1.90567633645207,
30.5610468081733));
#18565=CARTESIAN_POINT('Ctrl Pts',(0.599712284950682,-1.90247882297546,
30.56173310812));
#18566=CARTESIAN_POINT('Ctrl Pts',(0.606647453901798,-1.90027876038925,
30.562194972301));
#18567=CARTESIAN_POINT('Ctrl Pts',(0.664692071413225,-1.88151495452746,
30.5660500557109));
#18568=CARTESIAN_POINT('Ctrl Pts',(0.715130415396461,-1.86292880750781,
30.5693314713035));
#18569=CARTESIAN_POINT('Ctrl Pts',(0.787160307041539,-1.83302874296689,
30.5740006035073));
#18570=CARTESIAN_POINT('Ctrl Pts',(0.809388358443597,-1.8233228656232,30.5754390245067));
#18571=CARTESIAN_POINT('Ctrl Pts',(0.954956575308382,-1.75657374073807,
30.5848763214426));
#18572=CARTESIAN_POINT('Ctrl Pts',(1.07236769065602,-1.68746039417972,30.5925967011685));
#18573=CARTESIAN_POINT('Ctrl Pts',(1.25048146368272,-1.5564649688693,30.6056792896637));
#18574=CARTESIAN_POINT('Ctrl Pts',(1.31580685651395,-1.501644632093,30.6108269963243));
#18575=CARTESIAN_POINT('Ctrl Pts',(1.38581103446804,-1.43481351558923,30.6168777072078));
#18576=CARTESIAN_POINT('Ctrl Pts',(1.39412895587978,-1.42673280367127,30.6176057939713));
#18577=CARTESIAN_POINT('Ctrl Pts',(1.40661575435763,-1.414388641094,30.6187129932036));
#18578=CARTESIAN_POINT('Ctrl Pts',(1.41083685144731,-1.41017817519839,30.6190897762606));
#18579=CARTESIAN_POINT('Ctrl Pts',(1.41840172413926,-1.40256439223164,30.6197695873615));
#18580=CARTESIAN_POINT('Ctrl Pts',(1.42175229845131,-1.39916786934136,30.6200723120978));
#18581=CARTESIAN_POINT('Ctrl Pts',(1.428926957879,-1.39184243770791,30.6207240751154));
#18582=CARTESIAN_POINT('Ctrl Pts',(1.43274708700504,-1.3879097254672,30.6210732828345));
#18583=CARTESIAN_POINT('Ctrl Pts',(1.44304985958778,-1.37721545463019,30.6220210452301));
#18584=CARTESIAN_POINT('Ctrl Pts',(1.44950110448985,-1.37042396682332,30.6226209527871));
#18585=CARTESIAN_POINT('Ctrl Pts',(1.47868708987422,-1.33926204888278,30.6253648656451));
#18586=CARTESIAN_POINT('Ctrl Pts',(1.50085554452308,-1.31437085962979,30.6275327697879));
#18587=CARTESIAN_POINT('Ctrl Pts',(1.52668795766337,-1.28385969045721,30.6301639994736));
#18588=CARTESIAN_POINT('Ctrl Pts',(1.53096141755554,-1.27876071298762,30.6306028708265));
#18589=CARTESIAN_POINT('Ctrl Pts',(1.66677555185849,-1.11505430237392,30.6446660489814));
#18590=CARTESIAN_POINT('Ctrl Pts',(1.77296153164015,-0.937048985632428,
30.6593369465018));
#18591=CARTESIAN_POINT('Ctrl Pts',(1.86475313632124,-0.709422684456393,
30.676157820554));
#18592=CARTESIAN_POINT('Ctrl Pts',(1.87842333115145,-0.672392008025104,
30.6788321917695));
#18593=CARTESIAN_POINT('Ctrl Pts',(1.89544833846604,-0.621690924862446,
30.6823893307402));
#18594=CARTESIAN_POINT('Ctrl Pts',(1.89976994599906,-0.608356957110443,
30.6833151849895));
#18595=CARTESIAN_POINT('Ctrl Pts',(1.90688191613028,-0.585598404351281,
30.6848778075225));
#18596=CARTESIAN_POINT('Ctrl Pts',(1.9097437678265,-0.576196914324994,30.6855182432239));
#18597=CARTESIAN_POINT('Ctrl Pts',(1.91365499477745,-0.562998784093583,
30.6864098371225));
#18598=CARTESIAN_POINT('Ctrl Pts',(1.91476272450163,-0.5592197952835,30.6866642704505));
#18599=CARTESIAN_POINT('Ctrl Pts',(1.91663149296347,-0.552773890383566,
30.6870967782753));
#18600=CARTESIAN_POINT('Ctrl Pts',(1.91739817054981,-0.550108634379652,
30.6872751800331));
#18601=CARTESIAN_POINT('Ctrl Pts',(1.91885361008304,-0.545008977960254,
30.6876156947161));
#18602=CARTESIAN_POINT('Ctrl Pts',(1.91954330002405,-0.542574863493146,
30.6877778627617));
#18603=CARTESIAN_POINT('Ctrl Pts',(1.92116396173383,-0.536813313000923,
30.6881608711194));
#18604=CARTESIAN_POINT('Ctrl Pts',(1.9220909265001,-0.533484743532981,30.6883814784617));
#18605=CARTESIAN_POINT('Ctrl Pts',(1.92482762873337,-0.523557993642024,
30.6890374598215));
#18606=CARTESIAN_POINT('Ctrl Pts',(1.92661209615481,-0.516952809482917,
30.689471403394));
#18607=CARTESIAN_POINT('Ctrl Pts',(1.95931465938991,-0.393383053584198,
30.6975444595539));
#18608=CARTESIAN_POINT('Ctrl Pts',(1.97956782976853,-0.273833846997455,
30.7046079769933));
#18609=CARTESIAN_POINT('Ctrl Pts',(1.9965979475928,-0.0527030153000745,
30.7174866778348));
#18610=CARTESIAN_POINT('Ctrl Pts',(1.99671136958516,0.0482033673076015,
30.7232952989587));
#18611=CARTESIAN_POINT('Ctrl Pts',(1.98537695738878,0.199845621745218,30.7323320830419));
#18612=CARTESIAN_POINT('Ctrl Pts',(1.9795804643585,0.250839619821902,30.7354223276943));
#18613=CARTESIAN_POINT('Ctrl Pts',(1.96719461776964,0.331830036590219,30.7404510820538));
#18614=CARTESIAN_POINT('Ctrl Pts',(1.9618673992654,0.361997217729801,30.7423511208136));
#18615=CARTESIAN_POINT('Ctrl Pts',(1.95413690544867,0.400564995504602,30.7448196213694));
#18616=CARTESIAN_POINT('Ctrl Pts',(1.95237002333362,0.409090025516215,30.7453677397847));
#18617=CARTESIAN_POINT('Ctrl Pts',(1.94943037014696,0.422820605588681,30.7462546624203));
#18618=CARTESIAN_POINT('Ctrl Pts',(1.94829240739916,0.428033558181985,30.7465923504312));
#18619=CARTESIAN_POINT('Ctrl Pts',(1.94608178426778,0.437968836955508,30.747237801401));
#18620=CARTESIAN_POINT('Ctrl Pts',(1.94501281433492,0.442691952260742,30.7475454438513));
#18621=CARTESIAN_POINT('Ctrl Pts',(1.94252965595338,0.453480861724678,30.7482500429725));
#18622=CARTESIAN_POINT('Ctrl Pts',(1.94110424019645,0.459543995114412,30.7486473581997));
#18623=CARTESIAN_POINT('Ctrl Pts',(1.93663470927983,0.478163673360718,30.7498716986004));
#18624=CARTESIAN_POINT('Ctrl Pts',(1.93349702365987,0.490697200061785,30.7507017289416));
#18625=CARTESIAN_POINT('Ctrl Pts',(1.90241319493669,0.6099326689843,30.7586556496614));
#18626=CARTESIAN_POINT('Ctrl Pts',(1.86578885299894,0.714155680104044,30.7660656178356));
#18627=CARTESIAN_POINT('Ctrl Pts',(1.7504920215807,0.971796052374219,30.7855151316985));
#18628=CARTESIAN_POINT('Ctrl Pts',(1.66022992120136,1.11903860830284,30.7977858858425));
#18629=CARTESIAN_POINT('Ctrl Pts',(1.54047938103484,1.26739854869901,30.8104301363296));
#18630=CARTESIAN_POINT('Ctrl Pts',(1.52855476108158,1.28175512836226,30.8116561243319));
#18631=CARTESIAN_POINT('Ctrl Pts',(1.51317000171402,1.29975739504236,30.8131942625387));
#18632=CARTESIAN_POINT('Ctrl Pts',(1.50989567813382,1.30355965821875,30.8135191802807));
#18633=CARTESIAN_POINT('Ctrl Pts',(1.50463599353901,1.309620988541,30.8140371624583));
#18634=CARTESIAN_POINT('Ctrl Pts',(1.50265983767933,1.31188795985032,30.8142308948687));
#18635=CARTESIAN_POINT('Ctrl Pts',(1.49889082445507,1.31619193980454,30.8145987006605));
#18636=CARTESIAN_POINT('Ctrl Pts',(1.49709895952063,1.31822973397114,30.8147728399328));
#18637=CARTESIAN_POINT('Ctrl Pts',(1.4929701742655,1.32290590864273,30.8151724425145));
#18638=CARTESIAN_POINT('Ctrl Pts',(1.49063041757929,1.32554175453735,30.8153976906953));
#18639=CARTESIAN_POINT('Ctrl Pts',(1.48436040477098,1.3325676230156,30.8159981408393));
#18640=CARTESIAN_POINT('Ctrl Pts',(1.48041762566146,1.33694649739031,30.8163724232446));
#18641=CARTESIAN_POINT('Ctrl Pts',(1.45228777589943,1.36791065535068,30.8190199880785));
#18642=CARTESIAN_POINT('Ctrl Pts',(1.42740368168694,1.3938574047772,30.8212433878503));
#18643=CARTESIAN_POINT('Ctrl Pts',(1.34747252838203,1.47281475136465,30.8280792903375));
#18644=CARTESIAN_POINT('Ctrl Pts',(1.29007000064105,1.52334724299725,30.8325595986038));
#18645=CARTESIAN_POINT('Ctrl Pts',(1.14781640890008,1.63475275359846,30.8430721567568));
#18646=CARTESIAN_POINT('Ctrl Pts',(1.06081618589832,1.69250328575342,30.8490645059462));
#18647=CARTESIAN_POINT('Ctrl Pts',(0.920949457372957,1.77030843599053,30.8585425940331));
#18648=CARTESIAN_POINT('Ctrl Pts',(0.871084148335126,1.79536946538252,30.8618920317424));
#18649=CARTESIAN_POINT('Ctrl Pts',(0.790577342626261,1.83168603485874,30.867304212372));
#18650=CARTESIAN_POINT('Ctrl Pts',(0.760596238883982,1.84433712651924,30.869320473659));
#18651=CARTESIAN_POINT('Ctrl Pts',(0.722046714252709,1.85950400799374,30.8719195019825));
#18652=CARTESIAN_POINT('Ctrl Pts',(0.713751432085641,1.86270381499112,30.8724791449987));
#18653=CARTESIAN_POINT('Ctrl Pts',(0.700405716205775,1.8677495298035,30.8733802236168));
#18654=CARTESIAN_POINT('Ctrl Pts',(0.695368663239752,1.86963068402178,30.8737204768945));
#18655=CARTESIAN_POINT('Ctrl Pts',(0.685789262623026,1.87316417129478,30.8743678973662));
#18656=CARTESIAN_POINT('Ctrl Pts',(0.681248387502507,1.874820407186,30.8746749316005));
#18657=CARTESIAN_POINT('Ctrl Pts',(0.670913660495918,1.87854738542141,30.8753740620321));
#18658=CARTESIAN_POINT('Ctrl Pts',(0.665116178913216,1.88060785020684,30.8757664968253));
#18659=CARTESIAN_POINT('Ctrl Pts',(0.647477083563837,1.8867851389567,30.8769612881837));
#18660=CARTESIAN_POINT('Ctrl Pts',(0.63560628641287,1.89081711729916,30.8777664430997));
#18661=CARTESIAN_POINT('Ctrl Pts',(0.474428311750013,1.94387274851212,30.8887148909155));
#18662=CARTESIAN_POINT('Ctrl Pts',(0.319907205858484,1.97518669768371,30.8994672139777));
#18663=CARTESIAN_POINT('Ctrl Pts',(0.0728499961683398,1.99548641557686,
30.9167474341474));
#18664=CARTESIAN_POINT('Ctrl Pts',(-0.0180556620561916,1.99673443990206,
30.9231081777207));
#18665=CARTESIAN_POINT('Ctrl Pts',(-0.142959146209348,1.98991587033445,
30.9316428457092));
#18666=CARTESIAN_POINT('Ctrl Pts',(-0.177133731669345,1.98716542383185,
30.9339560064639));
#18667=CARTESIAN_POINT('Ctrl Pts',(-0.230279295259759,1.98150606611897,
30.9375025755029));
#18668=CARTESIAN_POINT('Ctrl Pts',(-0.249306786369179,1.97920212135878,
30.938762136657));
#18669=CARTESIAN_POINT('Ctrl Pts',(-0.273316927669692,1.97594308203664,
30.9403361485827));
#18670=CARTESIAN_POINT('Ctrl Pts',(-0.278332348221803,1.97524284879026,
30.9406640886255));
#18671=CARTESIAN_POINT('Ctrl Pts',(-0.286332199636548,1.97409486610209,
30.9411857514131));
#18672=CARTESIAN_POINT('Ctrl Pts',(-0.289318333071517,1.97365943652027,
30.9413801586184));
#18673=CARTESIAN_POINT('Ctrl Pts',(-0.294985113746101,1.97281998521662,
30.9417484704258));
#18674=CARTESIAN_POINT('Ctrl Pts',(-0.297665892261701,1.97241728041262,
30.9419224441514));
#18675=CARTESIAN_POINT('Ctrl Pts',(-0.303811077270586,1.97148134099633,
30.9423206543658));
#18676=CARTESIAN_POINT('Ctrl Pts',(-0.307274901448389,1.97094443959432,
30.9425446808002));
#18677=CARTESIAN_POINT('Ctrl Pts',(-0.318223433167899,1.96921782560283,
30.9432514775746));
#18678=CARTESIAN_POINT('Ctrl Pts',(-0.32570289680005,1.96799456948557,30.9437323853592));
#18679=CARTESIAN_POINT('Ctrl Pts',(-0.453220661742656,1.94639231382624,
30.9519010928209));
#18680=CARTESIAN_POINT('Ctrl Pts',(-0.571172914234161,1.91510398424772,
30.9590062235002));
#18681=CARTESIAN_POINT('Ctrl Pts',(-0.779934036278527,1.83870388260991,
30.971913531284));
#18682=CARTESIAN_POINT('Ctrl Pts',(-0.871570577203989,1.79707892404917,
30.977708657515));
#18683=CARTESIAN_POINT('Ctrl Pts',(-1.00437105303593,1.72419999591981,30.9867132523392));
#18684=CARTESIAN_POINT('Ctrl Pts',(-1.04810647246567,1.69796910002529,30.9897847281217));
#18685=CARTESIAN_POINT('Ctrl Pts',(-1.1163151962039,1.65341998241997,30.994785598706));
#18686=CARTESIAN_POINT('Ctrl Pts',(-1.14145669976805,1.63616432573231,30.9966770699671));
#18687=CARTESIAN_POINT('Ctrl Pts',(-1.17324378991871,1.61325823280222,30.9991359287365));
#18688=CARTESIAN_POINT('Ctrl Pts',(-1.18026236019065,1.60813055239652,30.9996831705399));
#18689=CARTESIAN_POINT('Ctrl Pts',(-1.19153232237129,1.59978333655726,31.0005690165759));
#18690=CARTESIAN_POINT('Ctrl Pts',(-1.19580476153005,1.59659229942491,31.0009065095651));
#18691=CARTESIAN_POINT('Ctrl Pts',(-1.20393313718495,1.59047037751699,31.0015518153356));
#18692=CARTESIAN_POINT('Ctrl Pts',(-1.20779130059531,1.58754250150899,31.0018595085681));
#18693=CARTESIAN_POINT('Ctrl Pts',(-1.21659132000148,1.58081371179655,31.0025645454249));
#18694=CARTESIAN_POINT('Ctrl Pts',(-1.22152607713847,1.5770036375097,31.0029622491975));
#18695=CARTESIAN_POINT('Ctrl Pts',(-1.23665677050138,1.56520775759385,31.004188959543));
#18696=CARTESIAN_POINT('Ctrl Pts',(-1.2467926984259,1.55714586550453,31.0050209881958));
#18697=CARTESIAN_POINT('Ctrl Pts',(-1.3444485473297,1.47790778560608,31.0131390546253));
#18698=CARTESIAN_POINT('Ctrl Pts',(-1.42584497091852,1.39953974556395,31.0207249829138));
#18699=CARTESIAN_POINT('Ctrl Pts',(-1.60699223410081,1.19284118011406,31.0396813484366));
#18700=CARTESIAN_POINT('Ctrl Pts',(-1.69855696436631,1.05839457902608,31.051215189611));
#18701=CARTESIAN_POINT('Ctrl Pts',(-1.78433231401984,0.892083818100652,
31.0637132140072));
#18702=CARTESIAN_POINT('Ctrl Pts',(-1.79539737586752,0.86959976587737,31.0653672913686));
#18703=CARTESIAN_POINT('Ctrl Pts',(-1.80838329073121,0.841907352272181,
31.067356243298));
#18704=CARTESIAN_POINT('Ctrl Pts',(-1.81070933565115,0.836892955853869,
31.0677144837592));
#18705=CARTESIAN_POINT('Ctrl Pts',(-1.81431587511598,0.829032692511845,
31.0682729848755));
#18706=CARTESIAN_POINT('Ctrl Pts',(-1.81561056394719,0.82619342793486,31.0684741041768));
#18707=CARTESIAN_POINT('Ctrl Pts',(-1.81801013308818,0.820898270458103,
31.0688480147248));
#18708=CARTESIAN_POINT('Ctrl Pts',(-1.81911669132216,0.818443203857005,
31.0690209061598));
#18709=CARTESIAN_POINT('Ctrl Pts',(-1.8216082945035,0.812885188778279,31.0694112595866));
#18710=CARTESIAN_POINT('Ctrl Pts',(-1.82299038087419,0.809780945934544,
31.0696285384681));
#18711=CARTESIAN_POINT('Ctrl Pts',(-1.82704226331502,0.800617246149869,
31.0702678082462));
#18712=CARTESIAN_POINT('Ctrl Pts',(-1.8296898609783,0.794547935859148,31.0706884628325));
#18713=CARTESIAN_POINT('Ctrl Pts',(-1.84771682335492,0.752655252470618,
31.0735738540965));
#18714=CARTESIAN_POINT('Ctrl Pts',(-1.86207456068305,0.716398079434474,
31.0759801010687));
#18715=CARTESIAN_POINT('Ctrl Pts',(-1.93366207878036,0.518892619388813,
31.0887229589495));
#18716=CARTESIAN_POINT('Ctrl Pts',(-1.97103251085257,0.351200079802946,
31.0983088032602));
#18717=CARTESIAN_POINT('Ctrl Pts',(-1.99199024364157,0.12090298573795,31.1119603016667));
#18718=CARTESIAN_POINT('Ctrl Pts',(-1.99472892756107,0.0608133453232126,
31.1155593179837));
#18719=CARTESIAN_POINT('Ctrl Pts',(-1.99476161122894,-0.0329699496448909,
31.1212980005034));
#18720=CARTESIAN_POINT('Ctrl Pts',(-1.99392110288183,-0.0666282922424112,
31.1233817344041));
#18721=CARTESIAN_POINT('Ctrl Pts',(-1.99176245094213,-0.109527298676257,
31.1260746683796));
#18722=CARTESIAN_POINT('Ctrl Pts',(-1.99123068893374,-0.118803320202428,
31.1266591688895));
#18723=CARTESIAN_POINT('Ctrl Pts',(-1.99027977406249,-0.133583107009423,
31.1275941251489));
#18724=CARTESIAN_POINT('Ctrl Pts',(-1.98990254352114,-0.139089510067221,
31.1279432641407));
#18725=CARTESIAN_POINT('Ctrl Pts',(-1.9891535798515,-0.149394658826164,
31.1285982157194));
#18726=CARTESIAN_POINT('Ctrl Pts',(-1.98878732101095,-0.154193772381355,
31.1289038541489));
#18727=CARTESIAN_POINT('Ctrl Pts',(-1.98793081947946,-0.164905483622833,
31.1295874664061));
#18728=CARTESIAN_POINT('Ctrl Pts',(-1.98743156155206,-0.17081729554009,
31.129965720991));
#18729=CARTESIAN_POINT('Ctrl Pts',(-1.98589097507003,-0.188137823472534,
31.1310768227705));
#18730=CARTESIAN_POINT('Ctrl Pts',(-1.98477774199113,-0.199539748630938,
31.1318119227424));
#18731=CARTESIAN_POINT('Ctrl Pts',(-1.9750825026045,-0.290712347049115,
31.1377201748076));
#18732=CARTESIAN_POINT('Ctrl Pts',(-1.96179428833453,-0.369898289376839,
31.1430415488625));
#18733=CARTESIAN_POINT('Ctrl Pts',(-1.92076118483009,-0.547908037891753,
31.1554441052938));
#18734=CARTESIAN_POINT('Ctrl Pts',(-1.8900879170194,-0.64582593183677,31.162590044847));
#18735=CARTESIAN_POINT('Ctrl Pts',(-1.8089546633255,-0.848622853619035,
31.1778265384721));
#18736=CARTESIAN_POINT('Ctrl Pts',(-1.75656185825405,-0.95235233947074,
31.1858893772912));
#18737=CARTESIAN_POINT('Ctrl Pts',(-1.69139589264723,-1.0574812221192,31.1939664512548));
#18738=CARTESIAN_POINT('Ctrl Pts',(-1.68730992401064,-1.0639886398782,31.1944659542551));
#18739=CARTESIAN_POINT('Ctrl Pts',(-1.68129477289349,-1.07344672613286,
31.195191083263));
#18740=CARTESIAN_POINT('Ctrl Pts',(-1.67939527139257,-1.07641604879225,
31.1954186090028));
#18741=CARTESIAN_POINT('Ctrl Pts',(-1.67601952907078,-1.08166236152653,
31.1958203662638));
#18742=CARTESIAN_POINT('Ctrl Pts',(-1.67454650166678,-1.0839413915343,31.1959948095547));
#18743=CARTESIAN_POINT('Ctrl Pts',(-1.67143129868892,-1.08873964710231,
31.1963619000435));
#18744=CARTESIAN_POINT('Ctrl Pts',(-1.66978807998935,-1.09125816085304,
31.1965544754713));
#18745=CARTESIAN_POINT('Ctrl Pts',(-1.66538832977033,-1.09796832451124,
31.1970673118286));
#18746=CARTESIAN_POINT('Ctrl Pts',(-1.66262164745684,-1.10215334200357,
31.197386899192));
#18747=CARTESIAN_POINT('Ctrl Pts',(-1.64949489575883,-1.12184758998798,
31.1988898378255));
#18748=CARTESIAN_POINT('Ctrl Pts',(-1.63893301141333,-1.13722208525549,
31.2000601680128));
#18749=CARTESIAN_POINT('Ctrl Pts',(-1.52880180633214,-1.29281351054718,
31.2118985563979));
#18750=CARTESIAN_POINT('Ctrl Pts',(-1.41169782662066,-1.41976390645456,
31.2215601666435));
#18751=CARTESIAN_POINT('Ctrl Pts',(-1.19512902499347,-1.60089388611909,
31.2380750574649));
#18752=CARTESIAN_POINT('Ctrl Pts',(-1.10480553221594,-1.66451019209258,
31.2446527987425));
#18753=CARTESIAN_POINT('Ctrl Pts',(-0.998552940405137,-1.72687189089505,
31.2523431478212));
#18754=CARTESIAN_POINT('Ctrl Pts',(-0.987346834026734,-1.73330341232639,
31.2531534616558));
#18755=CARTESIAN_POINT('Ctrl Pts',(-0.970647347051169,-1.74267325810439,
31.2543602214951));
#18756=CARTESIAN_POINT('Ctrl Pts',(-0.965201255853096,-1.74569553219334,
31.2547536516862));
#18757=CARTESIAN_POINT('Ctrl Pts',(-0.955495897536749,-1.75102215949897,
31.2554545986315));
#18758=CARTESIAN_POINT('Ctrl Pts',(-0.951242206671017,-1.75333661252938,
31.255761751733));
#18759=CARTESIAN_POINT('Ctrl Pts',(-0.94228405452954,-1.75816859056641,
31.2564085026703));
#18760=CARTESIAN_POINT('Ctrl Pts',(-0.937577841947787,-1.76068277144161,
31.2567482163119));
#18761=CARTESIAN_POINT('Ctrl Pts',(-0.925166228396138,-1.76724950378136,
31.2576440107137));
#18762=CARTESIAN_POINT('Ctrl Pts',(-0.917444351300789,-1.77127050928435,
31.2582012012529));
#18763=CARTESIAN_POINT('Ctrl Pts',(-0.882436988769638,-1.78920952658631,
31.2607268786577));
#18764=CARTESIAN_POINT('Ctrl Pts',(-0.854860700788525,-1.80254785730686,
31.2627155268454));
#18765=CARTESIAN_POINT('Ctrl Pts',(-0.78030175782316,-1.83651541931024,
31.2680933192741));
#18766=CARTESIAN_POINT('Ctrl Pts',(-0.732814525939007,-1.85597463156181,
31.2715200394762));
#18767=CARTESIAN_POINT('Ctrl Pts',(-0.589948822745992,-1.90817981500322,
31.2818293976884));
#18768=CARTESIAN_POINT('Ctrl Pts',(-0.492785294275005,-1.93554880165563,
31.2888489631142));
#18769=CARTESIAN_POINT('Ctrl Pts',(-0.31055985986979,-1.97226301299191,
31.3018182539593));
#18770=CARTESIAN_POINT('Ctrl Pts',(-0.226145057893152,-1.98371598325275,
31.3077486088162));
#18771=CARTESIAN_POINT('Ctrl Pts',(-0.104000930112791,-1.9923870143389,
31.3160252832614));
#18772=CARTESIAN_POINT('Ctrl Pts',(-0.0666797487889978,-1.99398507070906,
31.318513038267));
#18773=CARTESIAN_POINT('Ctrl Pts',(-0.0233727295804408,-1.99462197154133,
31.3213358046737));
#18774=CARTESIAN_POINT('Ctrl Pts',(-0.0174121017075229,-1.99468291082677,
31.3217229134923));
#18775=CARTESIAN_POINT('Ctrl Pts',(-0.00790670810490513,-1.99473747904275,
31.3223378959271));
#18776=CARTESIAN_POINT('Ctrl Pts',(-0.0043621354115291,-1.99474837976677,
31.3225667050627));
#18777=CARTESIAN_POINT('Ctrl Pts',(0.00189893929976689,-1.99475094577658,
31.3229699314499));
#18778=CARTESIAN_POINT('Ctrl Pts',(0.00461541722253504,-1.99474651019386,
31.3231445657359));
#18779=CARTESIAN_POINT('Ctrl Pts',(0.0103288967384952,-1.99472550952791,
31.3235112032417));
#18780=CARTESIAN_POINT('Ctrl Pts',(0.0133258654602947,-1.99470773951213,
31.3237031379598));
#18781=CARTESIAN_POINT('Ctrl Pts',(0.0212939952866249,-1.99464253505055,
31.3242124501749));
#18782=CARTESIAN_POINT('Ctrl Pts',(0.0262650786026712,-1.99458327070993,
31.3245291703128));
#18783=CARTESIAN_POINT('Ctrl Pts',(0.0494035287369734,-1.994220899404,31.3259988236147));
#18784=CARTESIAN_POINT('Ctrl Pts',(0.0675671473895573,-1.99368815045075,
31.3271394256868));
#18785=CARTESIAN_POINT('Ctrl Pts',(0.241673483147874,-1.98619924508064,
31.3379688731667));
#18786=CARTESIAN_POINT('Ctrl Pts',(0.396322512233222,-1.96120799433469,
31.3468203829917));
#18787=CARTESIAN_POINT('Ctrl Pts',(0.668230310714495,-1.88375123072126,
31.3632796418581));
#18788=CARTESIAN_POINT('Ctrl Pts',(0.786372787210431,-1.83756943174109,
31.3707668742538));
#18789=CARTESIAN_POINT('Ctrl Pts',(0.910950628707126,-1.77464527598959,
31.3794778856057));
#18790=CARTESIAN_POINT('Ctrl Pts',(0.922508205036043,-1.768664892623,31.380293946435));
#18791=CARTESIAN_POINT('Ctrl Pts',(0.9395257587789,-1.75964710414976,31.3815076347467));
#18792=CARTESIAN_POINT('Ctrl Pts',(0.945031470324931,-1.75669635999092,
31.3819021952866));
#18793=CARTESIAN_POINT('Ctrl Pts',(0.954782659815761,-1.75141117618418,
31.3826044159038));
#18794=CARTESIAN_POINT('Ctrl Pts',(0.959033682556298,-1.74908702773522,
31.3829117075387));
#18795=CARTESIAN_POINT('Ctrl Pts',(0.967940325547837,-1.74417529479058,
31.3835579967661));
#18796=CARTESIAN_POINT('Ctrl Pts',(0.972594126987176,-1.74158450728703,
31.3838971072994));
#18797=CARTESIAN_POINT('Ctrl Pts',(0.984790681146831,-1.73473051071344,
31.384789604866));
#18798=CARTESIAN_POINT('Ctrl Pts',(0.992316067389571,-1.73043677981765,
31.3853440869163));
#18799=CARTESIAN_POINT('Ctrl Pts',(1.02595722414324,-1.71095066460426,31.3878401516244));
#18800=CARTESIAN_POINT('Ctrl Pts',(1.05175260086252,-1.69521582769805,31.3898013207235));
#18801=CARTESIAN_POINT('Ctrl Pts',(1.11955404455345,-1.65171457975108,31.3950870229719));
#18802=CARTESIAN_POINT('Ctrl Pts',(1.16088075581609,-1.62293483096847,31.3984475676285));
#18803=CARTESIAN_POINT('Ctrl Pts',(1.28094432433038,-1.53238934424328,31.4086318343161));
#18804=CARTESIAN_POINT('Ctrl Pts',(1.35616562476787,-1.46623563772346,31.4155927916674));
#18805=CARTESIAN_POINT('Ctrl Pts',(1.51227113446591,-1.30661846339647,31.4311702917142));
#18806=CARTESIAN_POINT('Ctrl Pts',(1.59010096463137,-1.21070317562561,31.4397668142298));
#18807=CARTESIAN_POINT('Ctrl Pts',(1.66278311415867,-1.10192421029253,31.4483081012237));
#18808=CARTESIAN_POINT('Ctrl Pts',(1.66694508326684,-1.09561797345798,31.4487992025702));
#18809=CARTESIAN_POINT('Ctrl Pts',(1.67298291261794,-1.08635537106709,31.4495144323402));
#18810=CARTESIAN_POINT('Ctrl Pts',(1.67488691938656,-1.0834175676466,31.4497403889765));
#18811=CARTESIAN_POINT('Ctrl Pts',(1.67825123764825,-1.0781964994122,31.4501403587169));
#18812=CARTESIAN_POINT('Ctrl Pts',(1.67971463995098,-1.07591525535121,31.450314577153));
#18813=CARTESIAN_POINT('Ctrl Pts',(1.68279889382045,-1.07108569507647,31.4506822621726));
#18814=CARTESIAN_POINT('Ctrl Pts',(1.68441860454787,-1.068536685468,31.45087565288));
#18815=CARTESIAN_POINT('Ctrl Pts',(1.68874437659218,-1.06169475117012,31.451392975273));
#18816=CARTESIAN_POINT('Ctrl Pts',(1.69143987832476,-1.05739512648215,31.4517162125306));
#18817=CARTESIAN_POINT('Ctrl Pts',(1.70429856072879,-1.03670911002054,31.4532626778878));
#18818=CARTESIAN_POINT('Ctrl Pts',(1.71424061994018,-1.02018553545962,31.4544719522605));
#18819=CARTESIAN_POINT('Ctrl Pts',(1.74133536787651,-0.973639588628749,
31.4578139384052));
#18820=CARTESIAN_POINT('Ctrl Pts',(1.7579500889906,-0.94331049498492,31.4599180227951));
#18821=CARTESIAN_POINT('Ctrl Pts',(1.81570467359106,-0.83105163146685,31.4674973916642));
#18822=CARTESIAN_POINT('Ctrl Pts',(1.85197477854992,-0.746740896551033,
31.4727975064046));
#18823=CARTESIAN_POINT('Ctrl Pts',(1.93387665227392,-0.513238090566147,
31.4871489607838));
#18824=CARTESIAN_POINT('Ctrl Pts',(1.96803228989639,-0.360737962115578,
31.4962243243801));
#18825=CARTESIAN_POINT('Ctrl Pts',(1.9854000917869,-0.193318893556025,31.5067350360599));
#18826=CARTESIAN_POINT('Ctrl Pts',(1.98657939846431,-0.180798233188507,
31.5075239625511));
#18827=CARTESIAN_POINT('Ctrl Pts',(1.9881598890501,-0.162128870647861,31.5087049036983));
#18828=CARTESIAN_POINT('Ctrl Pts',(1.9886511197695,-0.155987940499084,31.5090940891839));
#18829=CARTESIAN_POINT('Ctrl Pts',(1.98947704994391,-0.145024141891785,
31.5097902819723));
#18830=CARTESIAN_POINT('Ctrl Pts',(1.98982267984085,-0.140202125881214,
31.5100969435755));
#18831=CARTESIAN_POINT('Ctrl Pts',(1.990515392184,-0.130018842934366,31.5107455680417));
#18832=CARTESIAN_POINT('Ctrl Pts',(1.9908583505561,-0.124657342861111,31.511087657839));
#18833=CARTESIAN_POINT('Ctrl Pts',(1.99171018268322,-0.110439169708111,
31.511996440212));
#18834=CARTESIAN_POINT('Ctrl Pts',(1.99218163557418,-0.101580454187658,
31.5125643014764));
#18835=CARTESIAN_POINT('Ctrl Pts',(1.99409664275567,-0.0604256581406491,
31.515210242771));
#18836=CARTESIAN_POINT('Ctrl Pts',(1.99481396147143,-0.0281022429469557,
31.5173109107531));
#18837=CARTESIAN_POINT('Ctrl Pts',(1.99462848699205,0.0595108459868649,
31.5230696566777));
#18838=CARTESIAN_POINT('Ctrl Pts',(1.99221291629348,0.114765431808765,31.5267721887616));
#18839=CARTESIAN_POINT('Ctrl Pts',(1.9786568764814,0.273397176545756,31.5375973993595));
#18840=CARTESIAN_POINT('Ctrl Pts',(1.9617288349155,0.376092801969814,31.5448548867649));
#18841=CARTESIAN_POINT('Ctrl Pts',(1.91982099236979,0.546264088238355,31.5570762498082));
#18842=CARTESIAN_POINT('Ctrl Pts',(1.89905670194791,0.614574610478577,31.5620342278734));
#18843=CARTESIAN_POINT('Ctrl Pts',(1.87180484754695,0.689525026096684,31.5674433288023));
#18844=CARTESIAN_POINT('Ctrl Pts',(1.86888403523982,0.697402764452382,31.5680114404149));
#18845=CARTESIAN_POINT('Ctrl Pts',(1.85393417509735,0.736955652157489,31.5708609669836));
#18846=CARTESIAN_POINT('Ctrl Pts',(1.84114838143125,0.768341417690629,31.5731128651521));
#18847=CARTESIAN_POINT('Ctrl Pts',(1.825248821063,0.804691122415102,31.5756976405419));
#18848=CARTESIAN_POINT('Ctrl Pts',(1.82290627416089,0.809983813984174,31.5760734080373));
#18849=CARTESIAN_POINT('Ctrl Pts',(1.81911278480998,0.818454913064945,31.5766738015535));
#18850=CARTESIAN_POINT('Ctrl Pts',(1.81767649248571,0.821639785855652,31.5768992959467));
#18851=CARTESIAN_POINT('Ctrl Pts',(1.81511154039312,0.827287736378873,31.5772987410034));
#18852=CARTESIAN_POINT('Ctrl Pts',(1.81398622271243,0.829752304600239,31.5774728951019));
#18853=CARTESIAN_POINT('Ctrl Pts',(1.81159425920694,0.834962841633406,31.5778407641809));
#18854=CARTESIAN_POINT('Ctrl Pts',(1.8103263931149,0.837708217454025,31.5780344020515));
#18855=CARTESIAN_POINT('Ctrl Pts',(1.80690679726172,0.845068824695993,31.5785530849939));
#18856=CARTESIAN_POINT('Ctrl Pts',(1.80474361190948,0.849678756419764,31.5788774292591));
#18857=CARTESIAN_POINT('Ctrl Pts',(1.79422115995368,0.871881513028842,31.5804373605036));
#18858=CARTESIAN_POINT('Ctrl Pts',(1.7856218200629,0.889360291550394,31.5816586982367));
#18859=CARTESIAN_POINT('Ctrl Pts',(1.76082648907991,0.937948576875685,31.5850427452575));
#18860=CARTESIAN_POINT('Ctrl Pts',(1.74406351044277,0.968762217277947,31.5871759463878));
#18861=CARTESIAN_POINT('Ctrl Pts',(1.6793539848186,1.0805813788873,31.5949278823048));
#18862=CARTESIAN_POINT('Ctrl Pts',(1.62650269323416,1.15861006759258,31.6003629717028));
#18863=CARTESIAN_POINT('Ctrl Pts',(1.4741393642354,1.35247112854636,31.6146650352651));
#18864=CARTESIAN_POINT('Ctrl Pts',(1.36653146868423,1.46111179526675,31.6235619180456));
#18865=CARTESIAN_POINT('Ctrl Pts',(1.23772666560627,1.56435954324196,31.6338692246638));
#18866=CARTESIAN_POINT('Ctrl Pts',(1.22776598683763,1.57218915816348,31.6346639562076));
#18867=CARTESIAN_POINT('Ctrl Pts',(1.21283747479742,1.58369536325086,31.6358519105663));
#18868=CARTESIAN_POINT('Ctrl Pts',(1.20792591540474,1.58744471568395,31.6362422541167));
#18869=CARTESIAN_POINT('Ctrl Pts',(1.19913902701572,1.59408799907364,31.6369397392887));
#18870=CARTESIAN_POINT('Ctrl Pts',(1.19527042730956,1.59699078263677,31.6372465303173));
#18871=CARTESIAN_POINT('Ctrl Pts',(1.18709063689994,1.60308207373148,31.6378946209762));
#18872=CARTESIAN_POINT('Ctrl Pts',(1.18277707606709,1.60626731982539,31.6382360444444));
#18873=CARTESIAN_POINT('Ctrl Pts',(1.17150506883954,1.61452084020461,31.6391273782408));
#18874=CARTESIAN_POINT('Ctrl Pts',(1.16452662147575,1.61956148811715,31.6396783519874));
#18875=CARTESIAN_POINT('Ctrl Pts',(1.14915533829825,1.63051370881752,31.6408902213807));
#18876=CARTESIAN_POINT('Ctrl Pts',(1.14074909498099,1.63640595266676,31.6415518392329));
#18877=CARTESIAN_POINT('Ctrl Pts',(1.11578178752173,1.65362058048429,31.6435137726419));
#18878=CARTESIAN_POINT('Ctrl Pts',(1.09909537341397,1.66475804039522,31.6448209789791));
#18879=CARTESIAN_POINT('Ctrl Pts',(1.03961029349712,1.70317758601556,31.6494680590969));
#18880=CARTESIAN_POINT('Ctrl Pts',(0.995944244245937,1.72907425543426,31.6528566974803));
#18881=CARTESIAN_POINT('Ctrl Pts',(0.819969521404237,1.82455950937282,31.666420412365));
#18882=CARTESIAN_POINT('Ctrl Pts',(0.68100801141268,1.88084745961469,31.676977320569));
#18883=CARTESIAN_POINT('Ctrl Pts',(0.46675892014263,1.94074642214977,31.6923454881173));
#18884=CARTESIAN_POINT('Ctrl Pts',(0.395392680491269,1.95653463536107,31.6973140243895));
#18885=CARTESIAN_POINT('Ctrl Pts',(0.315812509173411,1.96960600202633,31.702580553906));
#18886=CARTESIAN_POINT('Ctrl Pts',(0.308304467064475,1.97079519592032,31.7030747501903));
#18887=CARTESIAN_POINT('Ctrl Pts',(0.297266964541532,1.9724787989843,31.7037971522802));
#18888=CARTESIAN_POINT('Ctrl Pts',(0.293742796407353,1.97300669808625,31.7040271937461));
#18889=CARTESIAN_POINT('Ctrl Pts',(0.287526848072439,1.97392078580919,31.7044318364722));
#18890=CARTESIAN_POINT('Ctrl Pts',(0.284835669729489,1.97431091741512,31.7046066598221));
#18891=CARTESIAN_POINT('Ctrl Pts',(0.279186113964529,1.97511812353048,31.7049728891172));
#18892=CARTESIAN_POINT('Ctrl Pts',(0.276227601326714,1.97553405454891,31.7051642296273));
#18893=CARTESIAN_POINT('Ctrl Pts',(0.26838537885304,1.97661861477747,31.7056702739139));
#18894=CARTESIAN_POINT('Ctrl Pts',(0.263500067111318,1.97727579658209,31.705984335218));
#18895=CARTESIAN_POINT('Ctrl Pts',(0.241394414231006,1.98016610999669,31.7074003129144));
#18896=CARTESIAN_POINT('Ctrl Pts',(0.224147152122042,1.98219252093038,31.7084910317905));
#18897=CARTESIAN_POINT('Ctrl Pts',(0.177025709124408,1.98710596697326,31.7114380964622));
#18898=CARTESIAN_POINT('Ctrl Pts',(0.147108356580656,1.98954456057873,31.7132732349823));
#18899=CARTESIAN_POINT('Ctrl Pts',(0.0438243656781907,1.9956206098865,31.7195197359325));
#18900=CARTESIAN_POINT('Ctrl Pts',(-0.0296846664218811,1.99588139112504,
31.7238125094491));
#18901=CARTESIAN_POINT('Ctrl Pts',(-0.231575504118225,1.98543814595198,
31.7355605813361));
#18902=CARTESIAN_POINT('Ctrl Pts',(-0.35915154540047,1.96636708545194,31.7429565556513));
#18903=CARTESIAN_POINT('Ctrl Pts',(-0.489162829433394,1.93384994966077,
31.7510296138392));
#18904=CARTESIAN_POINT('Ctrl Pts',(-0.494321966244416,1.93253763080756,
31.7513508270761));
#18905=CARTESIAN_POINT('Ctrl Pts',(-0.547525015231715,1.91877749789665,
31.754672430475));
#18906=CARTESIAN_POINT('Ctrl Pts',(-0.595090240832385,1.90456233695754,
31.757719614464));
#18907=CARTESIAN_POINT('Ctrl Pts',(-0.651226834633883,1.88547729968685,
31.7614303712885));
#18908=CARTESIAN_POINT('Ctrl Pts',(-0.6603576727969,1.88229880106584,31.7620375981266));
#18909=CARTESIAN_POINT('Ctrl Pts',(-0.675236709955617,1.87699773314875,
31.7630332409085));
#18910=CARTESIAN_POINT('Ctrl Pts',(-0.680998944901184,1.87491480883781,
31.7634203397282));
#18911=CARTESIAN_POINT('Ctrl Pts',(-0.691286782467627,1.87114229338679,
31.7641142131815));
#18912=CARTESIAN_POINT('Ctrl Pts',(-0.695816035630299,1.86946274143192,
31.7644206509254));
#18913=CARTESIAN_POINT('Ctrl Pts',(-0.705387508850471,1.8658738152518,31.7650702824904));
#18914=CARTESIAN_POINT('Ctrl Pts',(-0.710428169980008,1.86396041976275,
31.7654136089461));
#18915=CARTESIAN_POINT('Ctrl Pts',(-0.72338247670079,1.85898288574999,31.7662990923728));
#18916=CARTESIAN_POINT('Ctrl Pts',(-0.731284374631854,1.85588866498951,
31.7668422561172));
#18917=CARTESIAN_POINT('Ctrl Pts',(-0.767167960746504,1.84157263896357,
31.769322880701));
#18918=CARTESIAN_POINT('Ctrl Pts',(-0.794911509966742,1.82976828871729,
31.7712799077328));
#18919=CARTESIAN_POINT('Ctrl Pts',(-0.868300506866143,1.79655858791936,
31.776565498473));
#18920=CARTESIAN_POINT('Ctrl Pts',(-0.913417500753582,1.7740451741792,31.7799303033142));
#18921=CARTESIAN_POINT('Ctrl Pts',(-1.03578884163965,1.7070756619626,31.7893781633339));
#18922=CARTESIAN_POINT('Ctrl Pts',(-1.11098733074868,1.65911739166735,31.7955588969136));
#18923=CARTESIAN_POINT('Ctrl Pts',(-1.28322350500532,1.53229934263323,31.8104770178804));
#18924=CARTESIAN_POINT('Ctrl Pts',(-1.37656752317831,1.44902442193596,31.8192216794944));
#18925=CARTESIAN_POINT('Ctrl Pts',(-1.47114721374974,1.34720207922994,31.8283894168494));
#18926=CARTESIAN_POINT('Ctrl Pts',(-1.48066187909967,1.33673781807645,31.8293153497696));
#18927=CARTESIAN_POINT('Ctrl Pts',(-1.49319632535118,1.32265433253208,31.8305390479337));
#18928=CARTESIAN_POINT('Ctrl Pts',(-1.49631544689657,1.31912464683561,31.8308438853024));
#18929=CARTESIAN_POINT('Ctrl Pts',(-1.5011670570152,1.31359507833088,31.8313185091842));
#18930=CARTESIAN_POINT('Ctrl Pts',(-1.50290809294974,1.31160277036519,31.8314889262303));
#18931=CARTESIAN_POINT('Ctrl Pts',(-1.50624487384275,1.30776904673698,31.831815711239));
#18932=CARTESIAN_POINT('Ctrl Pts',(-1.50784119014367,1.30592819288101,31.8319721200723));
#18933=CARTESIAN_POINT('Ctrl Pts',(-1.51165352281501,1.30151554504969,31.8323458435939));
#18934=CARTESIAN_POINT('Ctrl Pts',(-1.51386634857698,1.29894101717877,31.8325629204929));
#18935=CARTESIAN_POINT('Ctrl Pts',(-1.52050776387904,1.29117399150973,31.8332149466197));
#18936=CARTESIAN_POINT('Ctrl Pts',(-1.52491634669059,1.28596433668023,31.8336484456093));
#18937=CARTESIAN_POINT('Ctrl Pts',(-1.55774094453056,1.24676909900251,31.8368821570024));
#18938=CARTESIAN_POINT('Ctrl Pts',(-1.58504700276328,1.21186498156154,31.8396064832872));
#18939=CARTESIAN_POINT('Ctrl Pts',(-1.65353665537894,1.11803740971378,31.8466186035995));
#18940=CARTESIAN_POINT('Ctrl Pts',(-1.6927389853383,1.05774631889586,31.8508209615641));
#18941=CARTESIAN_POINT('Ctrl Pts',(-1.76233776563529,0.936889773050073,
31.8589277130956));
#18942=CARTESIAN_POINT('Ctrl Pts',(-1.79307194369008,0.876635478967391,
31.8628298354817));
#18943=CARTESIAN_POINT('Ctrl Pts',(-1.86718057560378,0.711066249269365,
31.8734281650186));
#18944=CARTESIAN_POINT('Ctrl Pts',(-1.90469293873118,0.603421726761332,
31.8802027303199));
#18945=CARTESIAN_POINT('Ctrl Pts',(-1.93602775299199,0.480616393460285,
31.8881135814245));
#18946=CARTESIAN_POINT('Ctrl Pts',(-1.93910990009059,0.468026025727867,
31.8889264749027));
#18947=CARTESIAN_POINT('Ctrl Pts',(-1.94349290799761,0.449334813640755,
31.8901363451999));
#18948=CARTESIAN_POINT('Ctrl Pts',(-1.94488825245045,0.443256294069004,
31.8905302833063));
#18949=CARTESIAN_POINT('Ctrl Pts',(-1.94731658961138,0.432445514538081,
31.8912318021872));
#18950=CARTESIAN_POINT('Ctrl Pts',(-1.94836089941323,0.427715826430847,
31.8915390171575));
#18951=CARTESIAN_POINT('Ctrl Pts',(-1.9505184963178,0.417772166165348,31.8921855587713));
#18952=CARTESIAN_POINT('Ctrl Pts',(-1.95162812518011,0.412557447389252,
31.8925249999285));
#18953=CARTESIAN_POINT('Ctrl Pts',(-1.95383721984987,0.401967391309332,
31.8932151275237));
#18954=CARTESIAN_POINT('Ctrl Pts',(-1.95493543980102,0.396591843789078,
31.8935658506495));
#18955=CARTESIAN_POINT('Ctrl Pts',(-1.95759427977766,0.383297969662468,
31.89443424546));
#18956=CARTESIAN_POINT('Ctrl Pts',(-1.95912903714579,0.375374626731649,
31.8949527378347));
#18957=CARTESIAN_POINT('Ctrl Pts',(-1.96623799565932,0.337442314827941,
31.8974395116789));
#18958=CARTESIAN_POINT('Ctrl Pts',(-1.97117076890211,0.307318727113851,
31.8994280055389));
#18959=CARTESIAN_POINT('Ctrl Pts',(-1.98837368233782,0.184679224694825,
31.9075830637462));
#18960=CARTESIAN_POINT('Ctrl Pts',(-1.99483390543644,0.0914821201817975,
31.9139244644951));
#18961=CARTESIAN_POINT('Ctrl Pts',(-1.99474917736343,-0.00181160368489115,
31.9203782084164));
#18962=CARTESIAN_POINT('',(-1.99474925803387,0.00172048636055072,33.5209548813952));
#18963=CARTESIAN_POINT('Ctrl Pts',(-1.99474917872611,-0.00181010262051109,
31.9203781045778));
#18964=CARTESIAN_POINT('Ctrl Pts',(-1.99460252920774,-0.16341917550937,
31.9315576712192));
#18965=CARTESIAN_POINT('Ctrl Pts',(-1.97481767395285,-0.324419874890402,
31.9430492725144));
#18966=CARTESIAN_POINT('Ctrl Pts',(-1.93294150007795,-0.492856000596897,
31.9545502494962));
#18967=CARTESIAN_POINT('Ctrl Pts',(-1.92995931024995,-0.504407530381109,
31.9553359810977));
#18968=CARTESIAN_POINT('Ctrl Pts',(-1.92533025441611,-0.521695868119121,
31.9565066885494));
#18969=CARTESIAN_POINT('Ctrl Pts',(-1.92376104628966,-0.527452942263791,
31.9568956620103));
#18970=CARTESIAN_POINT('Ctrl Pts',(-1.92083256957472,-0.538009932115742,
31.9576072193171));
#18971=CARTESIAN_POINT('Ctrl Pts',(-1.91948108940886,-0.542811934376364,
31.957930226192));
#18972=CARTESIAN_POINT('Ctrl Pts',(-1.91728779153198,-0.550494406747934,
31.9584458809308));
#18973=CARTESIAN_POINT('Ctrl Pts',(-1.91645747436394,-0.553378095578015,
31.9586391864287));
#18974=CARTESIAN_POINT('Ctrl Pts',(-1.91486342593632,-0.558867601387181,
31.9590066786028));
#18975=CARTESIAN_POINT('Ctrl Pts',(-1.91410089066589,-0.561473700453169,
31.9591809291117));
#18976=CARTESIAN_POINT('Ctrl Pts',(-1.91233281169241,-0.567470960080185,
31.9595814419069));
#18977=CARTESIAN_POINT('Ctrl Pts',(-1.91132356872471,-0.570861007004688,
31.9598074857575));
#18978=CARTESIAN_POINT('Ctrl Pts',(-1.90859668714099,-0.579932301769424,
31.9604114478899));
#18979=CARTESIAN_POINT('Ctrl Pts',(-1.90686268444612,-0.585608652263019,
31.9607884295772));
#18980=CARTESIAN_POINT('Ctrl Pts',(-1.89419062109161,-0.626438211830169,
31.9634937694718));
#18981=CARTESIAN_POINT('Ctrl Pts',(-1.88230572916969,-0.661293052708772,
31.9657697635236));
#18982=CARTESIAN_POINT('Ctrl Pts',(-1.86528990525225,-0.707010738500025,
31.9687351437457));
#18983=CARTESIAN_POINT('Ctrl Pts',(-1.86101709121346,-0.718182436511426,
31.9694581646588));
#18984=CARTESIAN_POINT('Ctrl Pts',(-1.84774248610002,-0.7519760751726,31.9716422706262));
#18985=CARTESIAN_POINT('Ctrl Pts',(-1.83842659305895,-0.77447275424995,
31.9730921712081));
#18986=CARTESIAN_POINT('Ctrl Pts',(-1.79448605613852,-0.875319534647171,
31.9795966136992));
#18987=CARTESIAN_POINT('Ctrl Pts',(-1.75524759582562,-0.95156265087637,
31.9845311265067));
#18988=CARTESIAN_POINT('Ctrl Pts',(-1.68091434912792,-1.0756553270946,31.9929320771693));
#18989=CARTESIAN_POINT('Ctrl Pts',(-1.64837183615551,-1.12488989467681,
31.9963721626078));
#18990=CARTESIAN_POINT('Ctrl Pts',(-1.56949208003522,-1.2334410527669,32.004323521974));
#18991=CARTESIAN_POINT('Ctrl Pts',(-1.52188760685677,-1.29171916462684,
32.0088642042278));
#18992=CARTESIAN_POINT('Ctrl Pts',(-1.46022191589947,-1.35905831162468,
32.0145429407434));
#18993=CARTESIAN_POINT('Ctrl Pts',(-1.44918911949883,-1.37081669449004,
32.0155515798706));
#18994=CARTESIAN_POINT('Ctrl Pts',(-1.43432210778034,-1.3862813750418,32.0169017064251));
#18995=CARTESIAN_POINT('Ctrl Pts',(-1.43061362308862,-1.39010813255543,
32.0172377533172));
#18996=CARTESIAN_POINT('Ctrl Pts',(-1.4237314943523,-1.39715304198638,32.0178600586814));
#18997=CARTESIAN_POINT('Ctrl Pts',(-1.42056215296713,-1.40037536387611,
32.0181461281878));
#18998=CARTESIAN_POINT('Ctrl Pts',(-1.41398778118754,-1.40701435135392,
32.0187385012264));
#18999=CARTESIAN_POINT('Ctrl Pts',(-1.41058125726587,-1.41042948999318,
32.0190448696595));
#19000=CARTESIAN_POINT('Ctrl Pts',(-1.40286752908041,-1.41810682835442,
32.0197373480939));
#19001=CARTESIAN_POINT('Ctrl Pts',(-1.39855323826709,-1.42236181021825,
32.0201237721689));
#19002=CARTESIAN_POINT('Ctrl Pts',(-1.38746265193813,-1.43320068990382,
32.0211149418448));
#19003=CARTESIAN_POINT('Ctrl Pts',(-1.38065890500309,-1.43975616372936,
32.0217209185731));
#19004=CARTESIAN_POINT('Ctrl Pts',(-1.34032893501446,-1.4780657068254,32.0253011037511));
#19005=CARTESIAN_POINT('Ctrl Pts',(-1.30575726045412,-1.5086938974447,32.0283230096475));
#19006=CARTESIAN_POINT('Ctrl Pts',(-1.26283843678116,-1.54413623642788,
32.0320230364921));
#19007=CARTESIAN_POINT('Ctrl Pts',(-1.25547757605955,-1.55012699004072,
32.0326558418));
#19008=CARTESIAN_POINT('Ctrl Pts',(-1.22678999376674,-1.57313646426422,
32.0351152222687));
#19009=CARTESIAN_POINT('Ctrl Pts',(-1.20515842159974,-1.58976888156951,
32.0369551975045));
#19010=CARTESIAN_POINT('Ctrl Pts',(-1.1075329151385,-1.66169497587215,32.0451928170896));
#19011=CARTESIAN_POINT('Ctrl Pts',(-1.02803340041024,-1.71201754397389,
32.0517340861286));
#19012=CARTESIAN_POINT('Ctrl Pts',(-0.876292452786206,-1.79367738510105,
32.063757075621));
#19013=CARTESIAN_POINT('Ctrl Pts',(-0.805163029398242,-1.82671310937933,
32.0692220707789));
#19014=CARTESIAN_POINT('Ctrl Pts',(-0.702995319109108,-1.86703393796488,
32.0766957938108));
#19015=CARTESIAN_POINT('Ctrl Pts',(-0.673448107138935,-1.8778940398252,
32.0788145500876));
#19016=CARTESIAN_POINT('Ctrl Pts',(-0.626652773150874,-1.89384701632228,
32.0820908752231));
#19017=CARTESIAN_POINT('Ctrl Pts',(-0.609572685989556,-1.89941343982065,
32.0832704101091));
#19018=CARTESIAN_POINT('Ctrl Pts',(-0.587650401972819,-1.9062317558416,
32.0847615362654));
#19019=CARTESIAN_POINT('Ctrl Pts',(-0.582876170339136,-1.90769700772375,
32.0850848999818));
#19020=CARTESIAN_POINT('Ctrl Pts',(-0.575223217954676,-1.91001435184936,
32.0856009893714));
#19021=CARTESIAN_POINT('Ctrl Pts',(-0.572348028118944,-1.91087788980509,
32.0857943746047));
#19022=CARTESIAN_POINT('Ctrl Pts',(-0.566868817688548,-1.91251004638703,
32.0861619249559));
#19023=CARTESIAN_POINT('Ctrl Pts',(-0.564265209478509,-1.91327982988665,
32.0863361542917));
#19024=CARTESIAN_POINT('Ctrl Pts',(-0.558268326463397,-1.91503956410968,
32.0867364952955));
#19025=CARTESIAN_POINT('Ctrl Pts',(-0.554873988370586,-1.91602581244035,
32.0869623891513));
#19026=CARTESIAN_POINT('Ctrl Pts',(-0.545780951681496,-1.91864166678052,
32.0875656887129));
#19027=CARTESIAN_POINT('Ctrl Pts',(-0.540077527244917,-1.9202549204255,
32.0879421610499));
#19028=CARTESIAN_POINT('Ctrl Pts',(-0.4990570264107,-1.93166063937621,32.0906365277402));
#19029=CARTESIAN_POINT('Ctrl Pts',(-0.463480527727685,-1.94050430400641,
32.0929025339778));
#19030=CARTESIAN_POINT('Ctrl Pts',(-0.357583642502776,-1.96374933176799,
32.0994942583546));
#19031=CARTESIAN_POINT('Ctrl Pts',(-0.286704381305827,-1.97534293697457,
32.103709992737));
#19032=CARTESIAN_POINT('Ctrl Pts',(-0.0893910275549665,-1.99676975127825,
32.1152687563291));
#19033=CARTESIAN_POINT('Ctrl Pts',(0.0375775172028492,-1.99841604695161,
32.1225262440107));
#19034=CARTESIAN_POINT('Ctrl Pts',(0.207362483962403,-1.98442313844537,
32.1327173192462));
#19035=CARTESIAN_POINT('Ctrl Pts',(0.250750174591868,-1.97940858510854,
32.1353624102951));
#19036=CARTESIAN_POINT('Ctrl Pts',(0.311766711138105,-1.97031826397244,
32.1391598462591));
#19037=CARTESIAN_POINT('Ctrl Pts',(0.329559857134827,-1.96742034443492,
32.1402765781414));
#19038=CARTESIAN_POINT('Ctrl Pts',(0.360680684387621,-1.96191777278961,
32.142247536168));
#19039=CARTESIAN_POINT('Ctrl Pts',(0.374025763436493,-1.95941741777467,
32.1430984687277));
#19040=CARTESIAN_POINT('Ctrl Pts',(0.393572809090104,-1.95554808800512,
32.1443537219922));
#19041=CARTESIAN_POINT('Ctrl Pts',(0.399795615123871,-1.95428537966441,
32.1447546545595));
#19042=CARTESIAN_POINT('Ctrl Pts',(0.410788308822708,-1.95200008315828,
32.1454652923288));
#19043=CARTESIAN_POINT('Ctrl Pts',(0.415560695784435,-1.95098966341245,
32.1457746061943));
#19044=CARTESIAN_POINT('Ctrl Pts',(0.424815088748768,-1.94899480764177,
32.1463759797159));
#19045=CARTESIAN_POINT('Ctrl Pts',(0.429297502412028,-1.94801239053715,
32.1466679728914));
#19046=CARTESIAN_POINT('Ctrl Pts',(0.4412202199058,-1.94535612163037,32.1474465668618));
#19047=CARTESIAN_POINT('Ctrl Pts',(0.448654325315004,-1.9436550661366,32.1479340382652));
#19048=CARTESIAN_POINT('Ctrl Pts',(0.475306592498861,-1.93739549973819,
32.1496889902946));
#19049=CARTESIAN_POINT('Ctrl Pts',(0.494466041284157,-1.93259436163314,
32.1509642443329));
#19050=CARTESIAN_POINT('Ctrl Pts',(0.518108159569669,-1.9262953419642,32.1525553853301));
#19051=CARTESIAN_POINT('Ctrl Pts',(0.522661483916753,-1.92506487736978,
32.1528626380069));
#19052=CARTESIAN_POINT('Ctrl Pts',(0.532138335301516,-1.92246780551564,
32.1535038191477));
#19053=CARTESIAN_POINT('Ctrl Pts',(0.537061056009767,-1.92109840780178,
32.1538378344566));
#19054=CARTESIAN_POINT('Ctrl Pts',(0.746345972827151,-1.86201245102816,
32.1680790841398));
#19055=CARTESIAN_POINT('Ctrl Pts',(0.940164518691378,-1.77205298992048,
32.1831462798589));
#19056=CARTESIAN_POINT('Ctrl Pts',(1.15327514841124,-1.62818825993466,32.2008387844464));
#19057=CARTESIAN_POINT('Ctrl Pts',(1.18960681367958,-1.60183544162223,32.2038918576719));
#19058=CARTESIAN_POINT('Ctrl Pts',(1.24322178855893,-1.56011505909323,32.208419867963));
#19059=CARTESIAN_POINT('Ctrl Pts',(1.2611764906913,-1.54563688704249,32.2099402012554));
#19060=CARTESIAN_POINT('Ctrl Pts',(1.28303408548211,-1.52737698035299,32.2117918319514));
#19061=CARTESIAN_POINT('Ctrl Pts',(1.28717707561612,-1.5238871619295,32.2121428349445));
#19062=CARTESIAN_POINT('Ctrl Pts',(1.29366567520833,-1.51837619485871,32.2126925497014));
#19063=CARTESIAN_POINT('Ctrl Pts',(1.29602084382523,-1.51636642043307,32.2128920770251));
#19064=CARTESIAN_POINT('Ctrl Pts',(1.3004180102707,-1.51259638671973,32.2132645791995));
#19065=CARTESIAN_POINT('Ctrl Pts',(1.30246109610733,-1.5108374908643,32.2134376470236));
#19066=CARTESIAN_POINT('Ctrl Pts',(1.30709781585268,-1.50682933605535,32.2138304033565));
#19067=CARTESIAN_POINT('Ctrl Pts',(1.30968920694528,-1.50457752536953,32.2140498993328));
#19068=CARTESIAN_POINT('Ctrl Pts',(1.31638830382908,-1.49872586809576,32.2146173411055));
#19069=CARTESIAN_POINT('Ctrl Pts',(1.32048709491006,-1.49511579083626,32.2149645406434));
#19070=CARTESIAN_POINT('Ctrl Pts',(1.34561735429383,-1.47279794790838,32.2170937382671));
#19071=CARTESIAN_POINT('Ctrl Pts',(1.36626698134848,-1.45366247508109,32.2188453447964));
#19072=CARTESIAN_POINT('Ctrl Pts',(1.52841085904421,-1.2968992086817,32.232683053994));
#19073=CARTESIAN_POINT('Ctrl Pts',(1.64918308215051,-1.13938762449178,32.2436132713659));
#19074=CARTESIAN_POINT('Ctrl Pts',(1.76937314968082,-0.922444594052505,
32.2583606975573));
#19075=CARTESIAN_POINT('Ctrl Pts',(1.7921895088438,-0.877292170717651,32.261408478619));
#19076=CARTESIAN_POINT('Ctrl Pts',(1.82589763842589,-0.803768787432854,
32.2663741237908));
#19077=CARTESIAN_POINT('Ctrl Pts',(1.83790050341204,-0.775930431535747,
32.2682547491953));
#19078=CARTESIAN_POINT('Ctrl Pts',(1.85251591244637,-0.739788888702187,
32.2707013980596));
#19079=CARTESIAN_POINT('Ctrl Pts',(1.85571536527151,-0.731726236361655,
32.2712475246266));
#19080=CARTESIAN_POINT('Ctrl Pts',(1.86079517436667,-0.718677449071006,
32.2721320010526));
#19081=CARTESIAN_POINT('Ctrl Pts',(1.86270833973315,-0.713704138238731,
32.272469245974));
#19082=CARTESIAN_POINT('Ctrl Pts',(1.86632270486252,-0.704194995302186,
32.2731143680412));
#19083=CARTESIAN_POINT('Ctrl Pts',(1.86802735586801,-0.699660508491388,
32.2734221268617));
#19084=CARTESIAN_POINT('Ctrl Pts',(1.87189071192426,-0.689268953521005,
32.2741277253156));
#19085=CARTESIAN_POINT('Ctrl Pts',(1.874038466982,-0.683407894660107,32.2745259271383));
#19086=CARTESIAN_POINT('Ctrl Pts',(1.88057104249785,-0.665318624547086,
32.275755679142));
#19087=CARTESIAN_POINT('Ctrl Pts',(1.8848638787623,-0.653057779460557,32.2765902731791));
#19088=CARTESIAN_POINT('Ctrl Pts',(1.93001052458401,-0.519959299641784,
32.2856633390346));
#19089=CARTESIAN_POINT('Ctrl Pts',(1.95929563314645,-0.395534648478494,
32.2942905487739));
#19090=CARTESIAN_POINT('Ctrl Pts',(1.99745154162072,-0.11537668503847,32.3138866368626));
#19091=CARTESIAN_POINT('Ctrl Pts',(2.0003749271544,0.0403581757162858,32.3249010773372));
#19092=CARTESIAN_POINT('Ctrl Pts',(1.98343881142725,0.212900461363933,32.3363915194624));
#19093=CARTESIAN_POINT('Ctrl Pts',(1.98142222563669,0.230915884995325,32.337581849748));
#19094=CARTESIAN_POINT('Ctrl Pts',(1.97854045645687,0.253830450614741,32.3390817747177));
#19095=CARTESIAN_POINT('Ctrl Pts',(1.97790224287163,0.258756554367711,32.3394033910826));
#19096=CARTESIAN_POINT('Ctrl Pts',(1.97684958585329,0.266650058701996,32.3399173520342));
#19097=CARTESIAN_POINT('Ctrl Pts',(1.9764468513592,0.269618958787515,32.3401103467698));
#19098=CARTESIAN_POINT('Ctrl Pts',(1.9756661743089,0.275278242874885,32.3404776139538));
#19099=CARTESIAN_POINT('Ctrl Pts',(1.97528942918531,0.27796872906143,32.3406519487306));
#19100=CARTESIAN_POINT('Ctrl Pts',(1.97440821043105,0.284169593650608,32.3410531389782));
#19101=CARTESIAN_POINT('Ctrl Pts',(1.97389987136427,0.287679400854737,32.3412797735571));
#19102=CARTESIAN_POINT('Ctrl Pts',(1.97251110822302,0.297091058185662,32.3418863475102));
#19103=CARTESIAN_POINT('Ctrl Pts',(1.97161354931177,0.302990401265001,32.3422653375212));
#19104=CARTESIAN_POINT('Ctrl Pts',(1.96488639775802,0.345909598558773,32.3450142944206));
#19105=CARTESIAN_POINT('Ctrl Pts',(1.95804060256359,0.382765520545583,32.3473299829406));
#19106=CARTESIAN_POINT('Ctrl Pts',(1.93229126099402,0.50249418724707,32.3547696227162));
#19107=CARTESIAN_POINT('Ctrl Pts',(1.90912974723013,0.584359455018703,32.3597275441746));
#19108=CARTESIAN_POINT('Ctrl Pts',(1.84724713772239,0.759512377896457,32.3705144928822));
#19109=CARTESIAN_POINT('Ctrl Pts',(1.80652972150162,0.851839357662067,32.3763231316148));
#19110=CARTESIAN_POINT('Ctrl Pts',(1.73481793027285,0.985934443870743,32.3853599576982));
#19111=CARTESIAN_POINT('Ctrl Pts',(1.7088874064594,1.03022483231553,32.3884502268421));
#19112=CARTESIAN_POINT('Ctrl Pts',(1.66479579497099,1.09928195182521,32.3934790175597));
#19113=CARTESIAN_POINT('Ctrl Pts',(1.64771989280784,1.12471545022883,32.3953790674676));
#19114=CARTESIAN_POINT('Ctrl Pts',(1.62504771948245,1.15685922677724,32.3978475805561));
#19115=CARTESIAN_POINT('Ctrl Pts',(1.61998310947063,1.16394075550822,32.3983957000973));
#19116=CARTESIAN_POINT('Ctrl Pts',(1.61174009998203,1.17530842025117,32.3992826241084));
#19117=CARTESIAN_POINT('Ctrl Pts',(1.60859053886871,1.17961540764901,32.3996203123622));
#19118=CARTESIAN_POINT('Ctrl Pts',(1.60254961999386,1.187807109193,32.4002657634995));
#19119=CARTESIAN_POINT('Ctrl Pts',(1.59966131801297,1.19169403798347,32.4005734058732));
#19120=CARTESIAN_POINT('Ctrl Pts',(1.59302583627002,1.20055613824791,32.4012780043997));
#19121=CARTESIAN_POINT('Ctrl Pts',(1.58926946538158,1.20552433449504,32.401675319107));
#19122=CARTESIAN_POINT('Ctrl Pts',(1.57764953966693,1.22074420934558,32.4028996563797));
#19123=CARTESIAN_POINT('Ctrl Pts',(1.56970972536805,1.23093698445045,32.4037296840909));
#19124=CARTESIAN_POINT('Ctrl Pts',(1.49304891595192,1.32740275463032,32.4116834009324));
#19125=CARTESIAN_POINT('Ctrl Pts',(1.41739477913876,1.40789833920321,32.4190931509539));
#19126=CARTESIAN_POINT('Ctrl Pts',(1.20773083437981,1.59687059640301,32.4385423439482));
#19127=CARTESIAN_POINT('Ctrl Pts',(1.06561989148885,1.69501168981905,32.450813010916));
#19128=CARTESIAN_POINT('Ctrl Pts',(0.896085979347844,1.78224741857242,32.463457483311));
#19129=CARTESIAN_POINT('Ctrl Pts',(0.879369522662083,1.79055445270757,32.4646837191852));
#19130=CARTESIAN_POINT('Ctrl Pts',(0.858013506626741,1.80079581462543,32.466222122607));
#19131=CARTESIAN_POINT('Ctrl Pts',(0.853480582225938,1.80294859622175,32.4665470629523));
#19132=CARTESIAN_POINT('Ctrl Pts',(0.846218045305775,1.80636420107997,32.4670650726523));
#19133=CARTESIAN_POINT('Ctrl Pts',(0.843493654461969,1.80763797877819,32.4672588101046));
#19134=CARTESIAN_POINT('Ctrl Pts',(0.838305621625072,1.81004933929399,32.4676266196097));
#19135=CARTESIAN_POINT('Ctrl Pts',(0.835842569635021,1.81118804236173,32.4678007575777));
#19136=CARTESIAN_POINT('Ctrl Pts',(0.830175153705129,1.81379414419,32.4682003494771));
#19137=CARTESIAN_POINT('Ctrl Pts',(0.82696922151543,1.81525807819708,32.4684255883185));
#19138=CARTESIAN_POINT('Ctrl Pts',(0.816764217709754,1.8198853723048,32.4691400675413));
#19139=CARTESIAN_POINT('Ctrl Pts',(0.809750641604358,1.82301685638878,32.4696273873885));
#19140=CARTESIAN_POINT('Ctrl Pts',(0.696326753875739,1.87287563856048,32.4774512653194));
#19141=CARTESIAN_POINT('Ctrl Pts',(0.586032626659973,1.91026400213153,32.4842576744113));
#19142=CARTESIAN_POINT('Ctrl Pts',(0.37366553422335,1.96211034209167,32.4969613709237));
#19143=CARTESIAN_POINT('Ctrl Pts',(0.272519811608386,1.97869525897723,32.502852902173));
#19144=CARTESIAN_POINT('Ctrl Pts',(0.117426383721725,1.99200439431928,32.512088663048));
#19145=CARTESIAN_POINT('Ctrl Pts',(0.0641449312344817,1.99443105205114,
32.5152954628198));
#19146=CARTESIAN_POINT('Ctrl Pts',(-0.0206624008000958,1.99489163263012,
32.5204970118216));
#19147=CARTESIAN_POINT('Ctrl Pts',(-0.0521560952106073,1.99431670743821,
32.5224497923833));
#19148=CARTESIAN_POINT('Ctrl Pts',(-0.0924053732654867,1.99262793786886,
32.5249775869389));
#19149=CARTESIAN_POINT('Ctrl Pts',(-0.101186429457066,1.99220133377433,
32.5255310185995));
#19150=CARTESIAN_POINT('Ctrl Pts',(-0.115310827594806,1.99142151449313,
32.5264244672017));
#19151=CARTESIAN_POINT('Ctrl Pts',(-0.120656134923171,1.99110480174702,
32.5267633376429));
#19152=CARTESIAN_POINT('Ctrl Pts',(-0.130828596879996,1.99046096392345,
32.5274096829841));
#19153=CARTESIAN_POINT('Ctrl Pts',(-0.135655970521717,1.99013779112121,
32.5277170315977));
#19154=CARTESIAN_POINT('Ctrl Pts',(-0.146659476612136,1.98936093024505,
32.5284190447982));
#19155=CARTESIAN_POINT('Ctrl Pts',(-0.152834744385373,1.98889603859645,
32.5288140585213));
#19156=CARTESIAN_POINT('Ctrl Pts',(-0.171705819438603,1.98738696475351,
32.5300244141063));
#19157=CARTESIAN_POINT('Ctrl Pts',(-0.184393678265809,1.9862499326624,32.5308426623224));
#19158=CARTESIAN_POINT('Ctrl Pts',(-0.209671478215072,1.98374035800143,
32.5324820331688));
#19159=CARTESIAN_POINT('Ctrl Pts',(-0.222260971720968,1.9823692857021,32.5333030731097));
#19160=CARTESIAN_POINT('Ctrl Pts',(-0.381563468186005,1.96348371912612,
32.5437511959232));
#19161=CARTESIAN_POINT('Ctrl Pts',(-0.525875533563065,1.9298439829871,32.5539033747445));
#19162=CARTESIAN_POINT('Ctrl Pts',(-0.748316915354061,1.85117160846283,
32.5703567213781));
#19163=CARTESIAN_POINT('Ctrl Pts',(-0.829469932932192,1.81625864628333,
32.576532693651));
#19164=CARTESIAN_POINT('Ctrl Pts',(-0.93792137154601,1.76081141065677,32.5848375287752));
#19165=CARTESIAN_POINT('Ctrl Pts',(-0.967407486900249,1.74478547497055,
32.5871003654876));
#19166=CARTESIAN_POINT('Ctrl Pts',(-1.01282855005604,1.71859308044977,32.5905784648162));
#19167=CARTESIAN_POINT('Ctrl Pts',(-1.0290462240517,1.70893176601492,32.5918187427292));
#19168=CARTESIAN_POINT('Ctrl Pts',(-1.04941580267103,1.69640190187168,32.5933721623471));
#19169=CARTESIAN_POINT('Ctrl Pts',(-1.05369662545826,1.69374625089209,32.5936983764786));
#19170=CARTESIAN_POINT('Ctrl Pts',(-1.06052067794381,1.68947699747894,32.5942179375137));
#19171=CARTESIAN_POINT('Ctrl Pts',(-1.06307035749912,1.68787382486348,32.5944119594439));
#19172=CARTESIAN_POINT('Ctrl Pts',(-1.06790935141657,1.68481587622807,32.5947799808687));
#19173=CARTESIAN_POINT('Ctrl Pts',(-1.07019930113276,1.68336222351895,32.594954047644));
#19174=CARTESIAN_POINT('Ctrl Pts',(-1.07545096872875,1.68001343426015,32.5953530461423));
#19175=CARTESIAN_POINT('Ctrl Pts',(-1.07841064327152,1.67811513620968,32.595577764936));
#19176=CARTESIAN_POINT('Ctrl Pts',(-1.0877826054208,1.67206904366776,32.5962889424361));
#19177=CARTESIAN_POINT('Ctrl Pts',(-1.09417619705265,1.6678921840968,32.5967735056396));
#19178=CARTESIAN_POINT('Ctrl Pts',(-1.19955079536049,1.59818547145711,32.604752462756));
#19179=CARTESIAN_POINT('Ctrl Pts',(-1.29252904310272,1.52397399843088,32.6116934166522));
#19180=CARTESIAN_POINT('Ctrl Pts',(-1.45175067020464,1.3717704282141,32.6244883012895));
#19181=CARTESIAN_POINT('Ctrl Pts',(-1.51967224776997,1.2961208804621,32.630336566891));
#19182=CARTESIAN_POINT('Ctrl Pts',(-1.61338813931342,1.17419664340804,32.6394681910315));
#19183=CARTESIAN_POINT('Ctrl Pts',(-1.64359552490643,1.13152647364536,32.6426139009881));
#19184=CARTESIAN_POINT('Ctrl Pts',(-1.68901936743565,1.06169905722731,32.6477249611765));
#19185=CARTESIAN_POINT('Ctrl Pts',(-1.70533701470487,1.0352858601333,32.6496501971835));
#19186=CARTESIAN_POINT('Ctrl Pts',(-1.72545342597985,1.00095681779064,32.6521470383302));
#19187=CARTESIAN_POINT('Ctrl Pts',(-1.72982608843033,0.993380982386406,
32.6526977129275));
#19188=CARTESIAN_POINT('Ctrl Pts',(-1.73679007928916,0.981130139438561,
32.6535877751254));
#19189=CARTESIAN_POINT('Ctrl Pts',(-1.73941272486202,0.976472990774916,
32.6539260319847));
#19190=CARTESIAN_POINT('Ctrl Pts',(-1.74437477108422,0.967578239889731,
32.654571910364));
#19191=CARTESIAN_POINT('Ctrl Pts',(-1.74671752989929,0.963342546743949,
32.6548794085877));
#19192=CARTESIAN_POINT('Ctrl Pts',(-1.75203120629353,0.953652343689352,
32.6555827496625));
#19193=CARTESIAN_POINT('Ctrl Pts',(-1.7549920998638,0.948192421623277,32.6559789464901));
#19194=CARTESIAN_POINT('Ctrl Pts',(-1.76399174393227,0.931410406796379,
32.6571964794157));
#19195=CARTESIAN_POINT('Ctrl Pts',(-1.76994669050432,0.920043976410978,
32.6580207723699));
#19196=CARTESIAN_POINT('Ctrl Pts',(-1.823175507855,0.816014608763925,32.6655631253834));
#19197=CARTESIAN_POINT('Ctrl Pts',(-1.86323516851332,0.719859141452695,
32.6725342699386));
#19198=CARTESIAN_POINT('Ctrl Pts',(-1.94773814415773,0.461926119686491,
32.6911894243867));
#19199=CARTESIAN_POINT('Ctrl Pts',(-1.97962349760519,0.296898541243526,
32.7031229913283));
#19200=CARTESIAN_POINT('Ctrl Pts',(-1.99236283910541,0.101583410512929,
32.7162383097549));
#19201=CARTESIAN_POINT('Ctrl Pts',(-1.99360388671717,0.0732981554110923,
32.7181113729829));
#19202=CARTESIAN_POINT('Ctrl Pts',(-1.99437183448897,0.0392611111762049,
32.7203262884057));
#19203=CARTESIAN_POINT('Ctrl Pts',(-1.99447646588938,0.0335272730109116,
32.7206980781848));
#19204=CARTESIAN_POINT('Ctrl Pts',(-1.99460047908786,0.0246274957505847,
32.7212730016537));
#19205=CARTESIAN_POINT('Ctrl Pts',(-1.99463705283118,0.0214618857429049,
32.7214770771693));
#19206=CARTESIAN_POINT('Ctrl Pts',(-1.99469075505927,0.0156072187183045,
32.7218537091782));
#19207=CARTESIAN_POINT('Ctrl Pts',(-1.99470998215074,0.0129182376887925,
32.7220263790629));
#19208=CARTESIAN_POINT('Ctrl Pts',(-1.99474089383969,0.00689035271397881,
32.7224127566872));
#19209=CARTESIAN_POINT('Ctrl Pts',(-1.99474963291524,0.00355146445775524,
32.7226262972717));
#19210=CARTESIAN_POINT('Ctrl Pts',(-1.99475068666113,-0.00633823889024117,
32.7232574286588));
#19211=CARTESIAN_POINT('Ctrl Pts',(-1.99471911541581,-0.0128890916739229,
32.7236737035634));
#19212=CARTESIAN_POINT('Ctrl Pts',(-1.99419126645478,-0.0670500302154172,
32.7271015191955));
#19213=CARTESIAN_POINT('Ctrl Pts',(-1.99202275248162,-0.114632995312579,
32.7300246171534));
#19214=CARTESIAN_POINT('Ctrl Pts',(-1.98147383093918,-0.244017678124576,
32.7378416200914));
#19215=CARTESIAN_POINT('Ctrl Pts',(-1.96973736723722,-0.325453161411386,
32.7426199669138));
#19216=CARTESIAN_POINT('Ctrl Pts',(-1.92122278996094,-0.55886227595734,
32.7564518222252));
#19217=CARTESIAN_POINT('Ctrl Pts',(-1.87159144210308,-0.707504260175679,
32.765477840962));
#19218=CARTESIAN_POINT('Ctrl Pts',(-1.79612707593495,-0.86798806934733,
32.7764498410277));
#19219=CARTESIAN_POINT('Ctrl Pts',(-1.7868141226834,-0.887001126595059,
32.7777695626261));
#19220=CARTESIAN_POINT('Ctrl Pts',(-1.77363745489507,-0.912852290322353,
32.7795928394159));
#19221=CARTESIAN_POINT('Ctrl Pts',(-1.77003314329996,-0.919821609950433,
32.7800873026031));
#19222=CARTESIAN_POINT('Ctrl Pts',(-1.76423606829243,-0.930870618268236,
32.7808759446446));
#19223=CARTESIAN_POINT('Ctrl Pts',(-1.76207002545037,-0.934964297413323,
32.7811691777283));
#19224=CARTESIAN_POINT('Ctrl Pts',(-1.75760286506079,-0.943336276271809,
32.7817710207486));
#19225=CARTESIAN_POINT('Ctrl Pts',(-1.75530033774357,-0.947613784741125,
32.7820796792714));
#19226=CARTESIAN_POINT('Ctrl Pts',(-1.74995553255246,-0.957456749030787,
32.7827926296714));
#19227=CARTESIAN_POINT('Ctrl Pts',(-1.74690230167209,-0.963016167596326,
32.783197310371));
#19228=CARTESIAN_POINT('Ctrl Pts',(-1.73726226688231,-0.980372341362477,
32.7844670310505));
#19229=CARTESIAN_POINT('Ctrl Pts',(-1.73058220030843,-0.992116598329498,
32.7853354084742));
#19230=CARTESIAN_POINT('Ctrl Pts',(-1.6639604327434,-1.10652428336738,32.7938870200653));
#19231=CARTESIAN_POINT('Ctrl Pts',(-1.59508479454828,-1.20368418472471,
32.8019045945793));
#19232=CARTESIAN_POINT('Ctrl Pts',(-1.43637719390949,-1.3898455920855,32.8188180254318));
#19233=CARTESIAN_POINT('Ctrl Pts',(-1.34590099732977,-1.47763342105424,
32.827700295468));
#19234=CARTESIAN_POINT('Ctrl Pts',(-1.20755873497289,-1.58854794168747,
32.8398112385958));
#19235=CARTESIAN_POINT('Ctrl Pts',(-1.16611853459211,-1.61921316900989,
32.8432742835422));
#19236=CARTESIAN_POINT('Ctrl Pts',(-1.11758059817273,-1.65229932750113,
32.8471069350772));
#19237=CARTESIAN_POINT('Ctrl Pts',(-1.11160590301737,-1.65632478134333,
32.8475749726356));
#19238=CARTESIAN_POINT('Ctrl Pts',(-1.10272079340768,-1.66224139596949,
32.848265330155));
#19239=CARTESIAN_POINT('Ctrl Pts',(-1.09982712406865,-1.66415741572107,
32.8484892781032));
#19240=CARTESIAN_POINT('Ctrl Pts',(-1.09467367350379,-1.66755041868017,
32.8488865238553));
#19241=CARTESIAN_POINT('Ctrl Pts',(-1.09241588527345,-1.66903037247035,
32.8490600201042));
#19242=CARTESIAN_POINT('Ctrl Pts',(-1.0875825448234,-1.67218456124697,32.849430269065));
#19243=CARTESIAN_POINT('Ctrl Pts',(-1.08500613622704,-1.67385742622816,
32.8496269299387));
#19244=CARTESIAN_POINT('Ctrl Pts',(-1.07796794535264,-1.67840425347671,
32.8501622879692));
#19245=CARTESIAN_POINT('Ctrl Pts',(-1.07349850129062,-1.68126639726621,
32.8505002041631));
#19246=CARTESIAN_POINT('Ctrl Pts',(-1.05040334891452,-1.69592643406822,
32.8522360801427));
#19247=CARTESIAN_POINT('Ctrl Pts',(-1.0315935084831,-1.70743333596848,32.8536156240066));
#19248=CARTESIAN_POINT('Ctrl Pts',(-0.976513497681212,-1.73988587053753,
32.8575687182072));
#19249=CARTESIAN_POINT('Ctrl Pts',(-0.939768080325111,-1.7600050828664,
32.8600993798385));
#19250=CARTESIAN_POINT('Ctrl Pts',(-0.785688438822215,-1.83816542656085,
32.870390761747));
#19251=CARTESIAN_POINT('Ctrl Pts',(-0.663413815999872,-1.88574766924444,
32.8778317420061));
#19252=CARTESIAN_POINT('Ctrl Pts',(-0.435704190833042,-1.94944363914821,
32.8916870073637));
#19253=CARTESIAN_POINT('Ctrl Pts',(-0.331972647945805,-1.96976092875029,
32.8979960345232));
#19254=CARTESIAN_POINT('Ctrl Pts',(-0.214358417116515,-1.98324060158836,
32.9053862394449));
#19255=CARTESIAN_POINT('Ctrl Pts',(-0.201573367325775,-1.9845808071326,
32.9061924891071));
#19256=CARTESIAN_POINT('Ctrl Pts',(-0.182588713962379,-1.98638555135478,
32.9073943468194));
#19257=CARTESIAN_POINT('Ctrl Pts',(-0.176398279230839,-1.98694485146446,
32.9077869749619));
#19258=CARTESIAN_POINT('Ctrl Pts',(-0.16538204776158,-1.98788827050524,
32.9084870199819));
#19259=CARTESIAN_POINT('Ctrl Pts',(-0.160557255096413,-1.98828377373377,
32.9087940766024));
#19260=CARTESIAN_POINT('Ctrl Pts',(-0.15040497052267,-1.98907879406862,
32.9094411641322));
#19261=CARTESIAN_POINT('Ctrl Pts',(-0.145077225054335,-1.98947447885776,
32.9097813129042));
#19262=CARTESIAN_POINT('Ctrl Pts',(-0.131033105283022,-1.99046080387404,
32.9106794859957));
#19263=CARTESIAN_POINT('Ctrl Pts',(-0.122314404320698,-1.99101558730885,
32.9112386307938));
#19264=CARTESIAN_POINT('Ctrl Pts',(-0.0827081835528079,-1.99327465749413,
32.9137859005555));
#19265=CARTESIAN_POINT('Ctrl Pts',(-0.0517886577081614,-1.99431749228319,
32.9157946116533));
#19266=CARTESIAN_POINT('Ctrl Pts',(0.0311472345365564,-1.99518478656018,
32.9212399758421));
#19267=CARTESIAN_POINT('Ctrl Pts',(0.0831504487442948,-1.9936944850378,
32.9247153769912));
#19268=CARTESIAN_POINT('Ctrl Pts',(0.236166979560229,-1.98331238039391,
32.935116328932));
#19269=CARTESIAN_POINT('Ctrl Pts',(0.336623421845106,-1.9687519423375,32.9421785250825));
#19270=CARTESIAN_POINT('Ctrl Pts',(0.551925368442719,-1.92058123250234,
32.9575707618174));
#19271=CARTESIAN_POINT('Ctrl Pts',(0.665766651990023,-1.88414855313876,
32.9658755854131));
#19272=CARTESIAN_POINT('Ctrl Pts',(0.782011449260053,-1.83508388634968,
32.9741142567833));
#19273=CARTESIAN_POINT('Ctrl Pts',(0.788328179477207,-1.83237918059498,
32.9745611147245));
#19274=CARTESIAN_POINT('Ctrl Pts',(0.797806947325723,-1.82826246123259,
32.9752302722609));
#19275=CARTESIAN_POINT('Ctrl Pts',(0.800979409278544,-1.82687480104885,
32.9754539984321));
#19276=CARTESIAN_POINT('Ctrl Pts',(0.806465253307859,-1.82445821214568,
32.9758404395068));
#19277=CARTESIAN_POINT('Ctrl Pts',(0.808780306350825,-1.82343313255363,
32.9760033872609));
#19278=CARTESIAN_POINT('Ctrl Pts',(0.813625515008557,-1.8212766855627,32.9763441360387));
#19279=CARTESIAN_POINT('Ctrl Pts',(0.816155269449309,-1.82014445039982,
32.9765218805956));
#19280=CARTESIAN_POINT('Ctrl Pts',(0.822265327090099,-1.81739448932033,
32.9769508013742));
#19281=CARTESIAN_POINT('Ctrl Pts',(0.825843251819519,-1.81577143991545,
32.977201651383));
#19282=CARTESIAN_POINT('Ctrl Pts',(0.838302129444387,-1.81007529197663,
32.978074121406));
#19283=CARTESIAN_POINT('Ctrl Pts',(0.847158112663467,-1.80594744228603,
32.9786924626234));
#19284=CARTESIAN_POINT('Ctrl Pts',(0.971954437423615,-1.74665878507672,
32.9873850497081));
#19285=CARTESIAN_POINT('Ctrl Pts',(1.082354812598,-1.6804853714675,32.994829436277));
#19286=CARTESIAN_POINT('Ctrl Pts',(1.30847245175721,-1.51335965893541,33.0111395156997));
#19287=CARTESIAN_POINT('Ctrl Pts',(1.42045488035223,-1.40877902135488,33.0199821601658));
#19288=CARTESIAN_POINT('Ctrl Pts',(1.53277571921872,-1.27673489673572,33.0307065547587));
#19289=CARTESIAN_POINT('Ctrl Pts',(1.54590114402217,-1.26081045564831,33.0319925812937));
#19290=CARTESIAN_POINT('Ctrl Pts',(1.56386705661483,-1.23831092237548,33.0338009540979));
#19291=CARTESIAN_POINT('Ctrl Pts',(1.56891811486496,-1.23190505190047,33.0343148592367));
#19292=CARTESIAN_POINT('Ctrl Pts',(1.57681267320244,-1.22176568061353,33.0351268626001));
#19293=CARTESIAN_POINT('Ctrl Pts',(1.57968257299581,-1.21805277088309,33.0354239112952));
#19294=CARTESIAN_POINT('Ctrl Pts',(1.58518905875185,-1.21087660647659,33.035997482957));
#19295=CARTESIAN_POINT('Ctrl Pts',(1.58782746607541,-1.20741477777196,33.0362739318546));
#19296=CARTESIAN_POINT('Ctrl Pts',(1.59403663682675,-1.19921223628462,33.0369283935306));
#19297=CARTESIAN_POINT('Ctrl Pts',(1.59759759923401,-1.19446418818849,33.0373067874272));
#19298=CARTESIAN_POINT('Ctrl Pts',(1.60797608647322,-1.18049648383865,33.0384186949414));
#19299=CARTESIAN_POINT('Ctrl Pts',(1.61473527604945,-1.17123397414157,33.0391544663014));
#19300=CARTESIAN_POINT('Ctrl Pts',(1.6683507522509,-1.09641526956613,33.0450859467055));
#19301=CARTESIAN_POINT('Ctrl Pts',(1.71126925058332,-1.028141626131,33.0504312096927));
#19302=CARTESIAN_POINT('Ctrl Pts',(1.79921200468044,-0.867411001127563,
33.0628727337065));
#19303=CARTESIAN_POINT('Ctrl Pts',(1.8414569093389,-0.773691708500714,33.0700331376366));
#19304=CARTESIAN_POINT('Ctrl Pts',(1.9154757533281,-0.568593735928676,33.0852427227486));
#19305=CARTESIAN_POINT('Ctrl Pts',(1.9451628591711,-0.456830838117353,33.0932639219271));
#19306=CARTESIAN_POINT('Ctrl Pts',(1.96634193093139,-0.335538576007945,
33.10130451497));
#19307=CARTESIAN_POINT('Ctrl Pts',(1.96762117118397,-0.327953741719003,
33.101804549577));
#19308=CARTESIAN_POINT('Ctrl Pts',(1.96942287701189,-0.316880938839103,
33.102530304511));
#19309=CARTESIAN_POINT('Ctrl Pts',(1.96997999754359,-0.313398799686563,
33.1027579291361));
#19310=CARTESIAN_POINT('Ctrl Pts',(1.97094952077218,-0.30723429807065,33.1031597993702));
#19311=CARTESIAN_POINT('Ctrl Pts',(1.9713656868668,-0.304552551037628,33.1033342571552));
#19312=CARTESIAN_POINT('Ctrl Pts',(1.97223134247897,-0.298898197296047,
33.1037013114168));
#19313=CARTESIAN_POINT('Ctrl Pts',(1.97267958408598,-0.295925428827723,
33.1038938363791));
#19314=CARTESIAN_POINT('Ctrl Pts',(1.97385735468101,-0.287992774599749,
33.1044063962237));
#19315=CARTESIAN_POINT('Ctrl Pts',(1.97457491551555,-0.283031092250418,
33.1047257588138));
#19316=CARTESIAN_POINT('Ctrl Pts',(1.97786841080351,-0.259635428431879,
33.1062260641627));
#19317=CARTESIAN_POINT('Ctrl Pts',(1.98020506239208,-0.241167944528133,
33.1073940411166));
#19318=CARTESIAN_POINT('Ctrl Pts',(2.001481301371,-0.051759448188537,33.1192315031794));
#19319=CARTESIAN_POINT('Ctrl Pts',(1.9984989766766,0.120941573512309,33.1288939122785));
#19320=CARTESIAN_POINT('Ctrl Pts',(1.97027530242521,0.312246785996703,33.1402053206825));
#19321=CARTESIAN_POINT('Ctrl Pts',(1.96682271312304,0.333303481659332,33.1414579050391));
#19322=CARTESIAN_POINT('Ctrl Pts',(1.94712934879159,0.442416319655802,33.1480000358855));
#19323=CARTESIAN_POINT('Ctrl Pts',(1.92531290325817,0.529350518522361,33.153393457516));
#19324=CARTESIAN_POINT('Ctrl Pts',(1.8938662653826,0.626462894995729,33.1597678837332));
#19325=CARTESIAN_POINT('Ctrl Pts',(1.88988587120405,0.638370247031418,33.160555502763));
#19326=CARTESIAN_POINT('Ctrl Pts',(1.88378658289306,0.656059123548691,33.1617348632326));
#19327=CARTESIAN_POINT('Ctrl Pts',(1.88175284216143,0.661869853608689,33.1621237867165));
#19328=CARTESIAN_POINT('Ctrl Pts',(1.87807427352336,0.672226116991098,33.1628196869793));
#19329=CARTESIAN_POINT('Ctrl Pts',(1.87643975328666,0.676775280906877,33.1631263191619));
#19330=CARTESIAN_POINT('Ctrl Pts',(1.87295292380386,0.686370014223294,33.1637750648105));
#19331=CARTESIAN_POINT('Ctrl Pts',(1.87109672759531,0.691414120668633,33.1641173059152));
#19332=CARTESIAN_POINT('Ctrl Pts',(1.86611916461618,0.704773518840122,33.1650269177741));
#19333=CARTESIAN_POINT('Ctrl Pts',(1.86296263562231,0.713075496317366,33.1655954610281));
#19334=CARTESIAN_POINT('Ctrl Pts',(1.8480195899449,0.751600636541017,33.1682492998371));
#19335=CARTESIAN_POINT('Ctrl Pts',(1.83555294491301,0.781553006588485,33.17035734796));
#19336=CARTESIAN_POINT('Ctrl Pts',(1.79977005299998,0.86194065026131,33.1761415125654));
#19337=CARTESIAN_POINT('Ctrl Pts',(1.77506948850035,0.91172435132921,33.1798625658619));
#19338=CARTESIAN_POINT('Ctrl Pts',(1.65266449039351,1.13455006158867,33.1971522545641));
#19339=CARTESIAN_POINT('Ctrl Pts',(1.53153808410573,1.29340021235381,33.2114296567931));
#19340=CARTESIAN_POINT('Ctrl Pts',(1.37999190204386,1.44041859103112,33.2254683570575));
#19341=CARTESIAN_POINT('Ctrl Pts',(1.37095121313336,1.44902593351077,33.2262932480805));
#19342=CARTESIAN_POINT('Ctrl Pts',(1.35414598180514,1.46472755572686,33.2278025895567));
#19343=CARTESIAN_POINT('Ctrl Pts',(1.34640503328542,1.47184634067332,33.2284886688951));
#19344=CARTESIAN_POINT('Ctrl Pts',(1.33551523015057,1.48170308552749,33.2294406684291));
#19345=CARTESIAN_POINT('Ctrl Pts',(1.33241370588891,1.48449273516436,33.2297103352435));
#19346=CARTESIAN_POINT('Ctrl Pts',(1.327409875849,1.48896508817339,33.2301430061172));
#19347=CARTESIAN_POINT('Ctrl Pts',(1.32551308895486,1.49065390466338,33.230306467194));
#19348=CARTESIAN_POINT('Ctrl Pts',(1.32154473521287,1.49417359054091,33.230647294605));
#19349=CARTESIAN_POINT('Ctrl Pts',(1.31947258461452,1.49600377820404,33.2308246075698));
#19350=CARTESIAN_POINT('Ctrl Pts',(1.31447369662721,1.50040048521432,33.2312508002846));
#19351=CARTESIAN_POINT('Ctrl Pts',(1.31154321806377,1.50296277496545,33.2314993640596));
#19352=CARTESIAN_POINT('Ctrl Pts',(1.30139823581362,1.51178086286986,33.2323555263515));
#19353=CARTESIAN_POINT('Ctrl Pts',(1.29414618326472,1.517993547599,33.2329600078525));
#19354=CARTESIAN_POINT('Ctrl Pts',(1.27652810318094,1.53286856601141,33.2344112318479));
#19355=CARTESIAN_POINT('Ctrl Pts',(1.26611801278809,1.54147826409757,33.2352544762968));
#19356=CARTESIAN_POINT('Ctrl Pts',(1.22655068227239,1.573531265657,33.2384097725086));
#19357=CARTESIAN_POINT('Ctrl Pts',(1.19682173852103,1.5962597868546,33.2406801464849));
#19358=CARTESIAN_POINT('Ctrl Pts',(1.02666615247564,1.71891991245894,33.253233086772));
#19359=CARTESIAN_POINT('Ctrl Pts',(0.874388497338395,1.80116122881976,33.2628931104991));
#19360=CARTESIAN_POINT('Ctrl Pts',(0.705825483401582,1.86571813964814,33.2736446126897));
#19361=CARTESIAN_POINT('Ctrl Pts',(0.698208088731203,1.86858215026189,33.2741304319677));
#19362=CARTESIAN_POINT('Ctrl Pts',(0.670978526763432,1.87863025220074,33.2758672992567));
#19363=CARTESIAN_POINT('Ctrl Pts',(0.651271734543528,1.88555267617871,33.2771247604516));
#19364=CARTESIAN_POINT('Ctrl Pts',(0.588320847355043,1.906560888585,33.2811482278873));
#19365=CARTESIAN_POINT('Ctrl Pts',(0.544704542213219,1.91947709151793,33.2839461965681));
#19366=CARTESIAN_POINT('Ctrl Pts',(0.491586525877133,1.9332507974279,33.287381788232));
#19367=CARTESIAN_POINT('Ctrl Pts',(0.482469173488074,1.93554629238531,33.2879724517339));
#19368=CARTESIAN_POINT('Ctrl Pts',(0.467463384119336,1.93921171951324,33.288946322863));
#19369=CARTESIAN_POINT('Ctrl Pts',(0.461584273448809,1.9406195056699,33.2893283092148));
#19370=CARTESIAN_POINT('Ctrl Pts',(0.451004124934851,1.94310218372557,33.2900165546879));
#19371=CARTESIAN_POINT('Ctrl Pts',(0.446305398270003,1.94418679861605,33.2903224984778));
#19372=CARTESIAN_POINT('Ctrl Pts',(0.436402369265574,1.9464349393303,33.2909679327485));
#19373=CARTESIAN_POINT('Ctrl Pts',(0.431197248903606,1.947594653046,33.291307542953));
#19374=CARTESIAN_POINT('Ctrl Pts',(0.417423181221115,1.95060562497926,33.2922072315598));
#19375=CARTESIAN_POINT('Ctrl Pts',(0.408846647357733,1.9524212740326,33.2927684453925));
#19376=CARTESIAN_POINT('Ctrl Pts',(0.389924990092333,1.95629684007522,33.2940089406523));
#19377=CARTESIAN_POINT('Ctrl Pts',(0.379574987969912,1.95833134218392,33.2946890169339));
#19378=CARTESIAN_POINT('Ctrl Pts',(0.348741620139204,1.96413865095314,33.2967197684674));
#19379=CARTESIAN_POINT('Ctrl Pts',(0.328215290711517,1.96767274371108,33.2980779190363));
#19380=CARTESIAN_POINT('Ctrl Pts',(0.254751819115167,1.97913975476746,33.3029621034731));
#19381=CARTESIAN_POINT('Ctrl Pts',(0.201559130991383,1.9852621294249,33.3065425311369));
#19382=CARTESIAN_POINT('Ctrl Pts',(0.0324375198180166,1.99786085297244,
33.3180576294182));
#19383=CARTESIAN_POINT('Ctrl Pts',(-0.0838370256106724,1.9963634805252,
33.3261838085693));
#19384=CARTESIAN_POINT('Ctrl Pts',(-0.300765603454961,1.9745796666485,33.3413691960147));
#19385=CARTESIAN_POINT('Ctrl Pts',(-0.40130566376226,1.95662566500361,33.3484110605478));
#19386=CARTESIAN_POINT('Ctrl Pts',(-0.50762345945489,1.92909494597857,33.3555846945754));
#19387=CARTESIAN_POINT('Ctrl Pts',(-0.515192952414424,1.92708720972738,
33.3560938717393));
#19388=CARTESIAN_POINT('Ctrl Pts',(-0.526178709605743,1.92410398543749,
33.3568303787301));
#19389=CARTESIAN_POINT('Ctrl Pts',(-0.529604383265513,1.92316389809201,
33.3570596922142));
#19390=CARTESIAN_POINT('Ctrl Pts',(-0.535646358178066,1.92148846650882,
33.3574634985248));
#19391=CARTESIAN_POINT('Ctrl Pts',(-0.538263689682664,1.92075692077004,
33.3576382104472));
#19392=CARTESIAN_POINT('Ctrl Pts',(-0.543760583134392,1.91920841747427,
33.3580046820671));
#19393=CARTESIAN_POINT('Ctrl Pts',(-0.54663979712703,1.91839032888544,33.3581963745166));
#19394=CARTESIAN_POINT('Ctrl Pts',(-0.554279540014072,1.91620100631878,
33.358704345867));
#19395=CARTESIAN_POINT('Ctrl Pts',(-0.559036858850027,1.91481850231584,
33.3590199735593));
#19396=CARTESIAN_POINT('Ctrl Pts',(-0.58104470619389,1.90833388612255,33.3604771157639));
#19397=CARTESIAN_POINT('Ctrl Pts',(-0.598231537895576,1.90301609382746,
33.36160655363));
#19398=CARTESIAN_POINT('Ctrl Pts',(-0.645185362075614,1.88778905588708,
33.3646747281142));
#19399=CARTESIAN_POINT('Ctrl Pts',(-0.674795239872328,1.87740866141502,
33.3665902132715));
#19400=CARTESIAN_POINT('Ctrl Pts',(-0.7833372902581,1.83645679679908,33.3735822018617));
#19401=CARTESIAN_POINT('Ctrl Pts',(-0.860549156370975,1.80156823094579,
33.3784996505042));
#19402=CARTESIAN_POINT('Ctrl Pts',(-1.02295810536666,1.71535132457716,33.3891669631239));
#19403=CARTESIAN_POINT('Ctrl Pts',(-1.10700397635823,1.66235201070424,33.394903154773));
#19404=CARTESIAN_POINT('Ctrl Pts',(-1.19339505781599,1.59840673025072,33.4013154452251));
#19405=CARTESIAN_POINT('Ctrl Pts',(-1.20000593546468,1.59344958873478,33.4018095511411));
#19406=CARTESIAN_POINT('Ctrl Pts',(-1.21702790429884,1.58051972303505,33.4030909713356));
#19407=CARTESIAN_POINT('Ctrl Pts',(-1.22739141687754,1.57248523503708,33.4038801169651));
#19408=CARTESIAN_POINT('Ctrl Pts',(-1.27670318323539,1.53347097376726,33.4076803854793));
#19409=CARTESIAN_POINT('Ctrl Pts',(-1.31455948523975,1.50114521670288,33.4107357169756));
#19410=CARTESIAN_POINT('Ctrl Pts',(-1.3582840453595,1.46088522951964,33.4144554699272));
#19411=CARTESIAN_POINT('Ctrl Pts',(-1.36535485288055,1.45427896984817,33.4150632237763));
#19412=CARTESIAN_POINT('Ctrl Pts',(-1.37682570615761,1.44340434798724,33.4160595609246));
#19413=CARTESIAN_POINT('Ctrl Pts',(-1.38125469374114,1.43916663614045,33.4164468240244));
#19414=CARTESIAN_POINT('Ctrl Pts',(-1.3891391739411,1.43155274313149,33.4171408825983));
#19415=CARTESIAN_POINT('Ctrl Pts',(-1.39260208139003,1.42818428193993,33.4174473405043));
#19416=CARTESIAN_POINT('Ctrl Pts',(-1.39927736757128,1.42164369401301,33.4180412558098));
#19417=CARTESIAN_POINT('Ctrl Pts',(-1.40249128390312,1.41847317286848,33.418328641663));
#19418=CARTESIAN_POINT('Ctrl Pts',(-1.40944616629777,1.41156545304751,33.41895368707));
#19419=CARTESIAN_POINT('Ctrl Pts',(-1.41318308256238,1.40782424265122,33.4192915232835));
#19420=CARTESIAN_POINT('Ctrl Pts',(-1.42795826441165,1.39291397756558,33.4206352652754));
#19421=CARTESIAN_POINT('Ctrl Pts',(-1.43887910753933,1.3816298506566,33.4216463002903));
#19422=CARTESIAN_POINT('Ctrl Pts',(-1.49773489469329,1.31936152531275,33.427194792987));
#19423=CARTESIAN_POINT('Ctrl Pts',(-1.54308949701015,1.26601638188128,33.4318405247866));
#19424=CARTESIAN_POINT('Ctrl Pts',(-1.62125481303149,1.16362532963598,33.4405698861641));
#19425=CARTESIAN_POINT('Ctrl Pts',(-1.65487576150722,1.11529210529216,33.444620758554));
#19426=CARTESIAN_POINT('Ctrl Pts',(-1.76854597423252,0.935400231164669,
33.4593915017521));
#19427=CARTESIAN_POINT('Ctrl Pts',(-1.83544370345407,0.796166084685855,
33.4703016212475));
#19428=CARTESIAN_POINT('Ctrl Pts',(-1.89030717537424,0.637157036486766,
33.4813994658384));
#19429=CARTESIAN_POINT('Ctrl Pts',(-1.89480728568294,0.623647083518871,
33.4823318009305));
#19430=CARTESIAN_POINT('Ctrl Pts',(-1.90060705713279,0.605592837521602,
33.4835626369911));
#19431=CARTESIAN_POINT('Ctrl Pts',(-1.90203565852051,0.601090862772052,
33.4838683124037));
#19432=CARTESIAN_POINT('Ctrl Pts',(-1.90424035255221,0.594056610342024,
33.4843439391325));
#19433=CARTESIAN_POINT('Ctrl Pts',(-1.90502740313454,0.591527826975992,
33.4845145253664));
#19434=CARTESIAN_POINT('Ctrl Pts',(-1.90652867354078,0.586670190991764,
33.4848414342773));
#19435=CARTESIAN_POINT('Ctrl Pts',(-1.90724365556851,0.584341624737796,
33.4849977985661));
#19436=CARTESIAN_POINT('Ctrl Pts',(-1.90894323596698,0.578770049835498,
33.485371118825));
#19437=CARTESIAN_POINT('Ctrl Pts',(-1.90992383544618,0.575525839508009,
33.4855878384601));
#19438=CARTESIAN_POINT('Ctrl Pts',(-1.91284611733557,0.565768053294586,
33.4862377492209));
#19439=CARTESIAN_POINT('Ctrl Pts',(-1.91476280700752,0.559246953363802,
33.4866695039527));
#19440=CARTESIAN_POINT('Ctrl Pts',(-1.91907868441804,0.544280842726817,
33.4876547641027));
#19441=CARTESIAN_POINT('Ctrl Pts',(-1.92145554647378,0.535829471121856,
33.4882070493122));
#19442=CARTESIAN_POINT('Ctrl Pts',(-1.9707256688267,0.356095973906566,33.4998710935859));
#19443=CARTESIAN_POINT('Ctrl Pts',(-1.99459991896134,0.179306582252376,
33.5098330031497));
#19444=CARTESIAN_POINT('Ctrl Pts',(-1.99474929467395,0.0016774676722283,
33.5202191433277));
#19445=CARTESIAN_POINT('',(-1.9947497669637,-0.000964208625222721,34.3209548814384));
#19446=CARTESIAN_POINT('Ctrl Pts',(-1.99474925803387,0.00172048636055072,
33.5209548813952));
#19447=CARTESIAN_POINT('Ctrl Pts',(-1.99480900501761,-0.0675507698475596,
33.525367756855));
#19448=CARTESIAN_POINT('Ctrl Pts',(-1.9912561081305,-0.136886666161832,
33.5297806323149));
#19449=CARTESIAN_POINT('Ctrl Pts',(-1.98409705625583,-0.205879658676962,
33.5341935077747));
#19450=CARTESIAN_POINT('Ctrl Pts',(-1.9769407358986,-0.274846327096992,
33.5386046995135));
#19451=CARTESIAN_POINT('Ctrl Pts',(-1.96618104135419,-0.343469858405761,
33.5430158912523));
#19452=CARTESIAN_POINT('Ctrl Pts',(-1.95187642317062,-0.411346558476753,
33.5474270829911));
#19453=CARTESIAN_POINT('Ctrl Pts',(-1.93757225629807,-0.479221117036381,
33.5518381355567));
#19454=CARTESIAN_POINT('Ctrl Pts',(-1.9197234920193,-0.546348406239829,
33.5562491881224));
#19455=CARTESIAN_POINT('Ctrl Pts',(-1.89843956389977,-0.612335516461396,
33.560660240688));
#19456=CARTESIAN_POINT('Ctrl Pts',(-1.87713382054319,-0.678390261023937,
33.5650758144189));
#19457=CARTESIAN_POINT('Ctrl Pts',(-1.85238603593462,-0.743302020150988,
33.5694913881498));
#19458=CARTESIAN_POINT('Ctrl Pts',(-1.8243550541552,-0.806694613145749,
33.5739069618807));
#19459=CARTESIAN_POINT('Ctrl Pts',(-1.79630923971353,-0.870120750485432,
33.5783248721232));
#19460=CARTESIAN_POINT('Ctrl Pts',(-1.76497699468783,-0.932025678977947,
33.5827427823657));
#19461=CARTESIAN_POINT('Ctrl Pts',(-1.73056342603898,-0.99205735265469,
33.5871606926082));
#19462=CARTESIAN_POINT('Ctrl Pts',(-1.69608655433791,-1.05219945336132,
33.5915867295058));
#19463=CARTESIAN_POINT('Ctrl Pts',(-1.65851731041629,-1.11046100160717,
33.5960127664034));
#19464=CARTESIAN_POINT('Ctrl Pts',(-1.61810405492496,-1.16651910825987,
33.600438803301));
#19465=CARTESIAN_POINT('Ctrl Pts',(-1.58870100730711,-1.20730471583433,
33.6036590084559));
#19466=CARTESIAN_POINT('Ctrl Pts',(-1.55779340507657,-1.24692458229429,
33.6068792136108));
#19467=CARTESIAN_POINT('Ctrl Pts',(-1.52548938349084,-1.28526639392646,
33.6100994187656));
#19468=CARTESIAN_POINT('Ctrl Pts',(-1.48080783377919,-1.33829915821964,
33.6145534696747));
#19469=CARTESIAN_POINT('Ctrl Pts',(-1.43326901986471,-1.38910417913217,
33.6190075205837));
#19470=CARTESIAN_POINT('Ctrl Pts',(-1.383123640052,-1.43735749165936,33.6234615714927));
#19471=CARTESIAN_POINT('Ctrl Pts',(-1.33305363790775,-1.48553827064096,
33.6279089271494));
#19472=CARTESIAN_POINT('Ctrl Pts',(-1.2803851962972,-1.53117461743457,33.632356282806));
#19473=CARTESIAN_POINT('Ctrl Pts',(-1.22540866152179,-1.57397623068691,
33.6368036384627));
#19474=CARTESIAN_POINT('Ctrl Pts',(-1.17049694149409,-1.61672738285116,
33.6412457508963));
#19475=CARTESIAN_POINT('Ctrl Pts',(-1.11328291724205,-1.65665013985083,
33.6456878633299));
#19476=CARTESIAN_POINT('Ctrl Pts',(-1.05409177933541,-1.69349286483218,
33.6501299757635));
#19477=CARTESIAN_POINT('Ctrl Pts',(-0.994937981602122,-1.73031234792655,
33.6545692859322));
#19478=CARTESIAN_POINT('Ctrl Pts',(-0.933809959117067,-1.76405539538836,
33.6590085961009));
#19479=CARTESIAN_POINT('Ctrl Pts',(-0.871062546673523,-1.7945131936775,
33.6634479062696));
#19480=CARTESIAN_POINT('Ctrl Pts',(-0.808333396404629,-1.82496212744762,
33.6678859244097));
#19481=CARTESIAN_POINT('Ctrl Pts',(-0.743986231995407,-1.85212749647973,
33.6723239425497));
#19482=CARTESIAN_POINT('Ctrl Pts',(-0.678399611395581,-1.87584688334585,
33.6767619606897));
#19483=CARTESIAN_POINT('Ctrl Pts',(-0.612809793753564,-1.89956742642156,
33.6812001951624));
#19484=CARTESIAN_POINT('Ctrl Pts',(-0.545980861158996,-1.91984148959226,
33.6856384296351));
#19485=CARTESIAN_POINT('Ctrl Pts',(-0.478308741880752,-1.93655578539335,
33.6900766641078));
#19486=CARTESIAN_POINT('Ctrl Pts',(-0.410564937381926,-1.95328778668371,
33.6945196000118));
#19487=CARTESIAN_POINT('Ctrl Pts',(-0.341976639659408,-1.96645237650665,
33.6989625359158));
#19488=CARTESIAN_POINT('Ctrl Pts',(-0.272951303253476,-1.97598713268893,
33.7034054718197));
#19489=CARTESIAN_POINT('Ctrl Pts',(-0.203885677078493,-1.98552745426422,
33.7078510010448));
#19490=CARTESIAN_POINT('Ctrl Pts',(-0.134382992426301,-1.9914336836673,
33.7122965302699));
#19491=CARTESIAN_POINT('Ctrl Pts',(-0.0648543860996425,-1.99369543087796,
33.716742059495));
#19492=CARTESIAN_POINT('Ctrl Pts',(0.00479554274020294,-1.99596112467794,
33.7211953458549));
#19493=CARTESIAN_POINT('Ctrl Pts',(0.0744709941348924,-1.99456965162631,
33.7256486322149));
#19494=CARTESIAN_POINT('Ctrl Pts',(0.14376307234286,-1.98956270108045,33.7301019185749));
#19495=CARTESIAN_POINT('Ctrl Pts',(0.180865313670245,-1.98688174400323,
33.7324864177774));
#19496=CARTESIAN_POINT('Ctrl Pts',(0.217857760155773,-1.98316510193474,
33.7348709169799));
#19497=CARTESIAN_POINT('Ctrl Pts',(0.25467889410285,-1.97842518771839,33.7372554161824));
#19498=CARTESIAN_POINT('Ctrl Pts',(0.323458272612784,-1.96957134974426,
33.7417094988145));
#19499=CARTESIAN_POINT('Ctrl Pts',(0.391911591312129,-1.95710906248736,
33.7461635814465));
#19500=CARTESIAN_POINT('Ctrl Pts',(0.459630738094927,-1.94107370985708,
33.7506176640786));
#19501=CARTESIAN_POINT('Ctrl Pts',(0.527248098415184,-1.92506245944747,
33.7550650519229));
#19502=CARTESIAN_POINT('Ctrl Pts',(0.594133004519081,-1.90548891478166,
33.7595124397672));
#19503=CARTESIAN_POINT('Ctrl Pts',(0.659884182157403,-1.88244001993117,
33.7639598276115));
#19504=CARTESIAN_POINT('Ctrl Pts',(0.725557850587904,-1.85941829572074,
33.7684019727587));
#19505=CARTESIAN_POINT('Ctrl Pts',(0.790099985192176,-1.83292951932491,
33.7728441179059));
#19506=CARTESIAN_POINT('Ctrl Pts',(0.853122954715086,-1.80311086365709,
33.7772862630531));
#19507=CARTESIAN_POINT('Ctrl Pts',(0.916106171430466,-1.77331101661235,
33.7817256062418));
#19508=CARTESIAN_POINT('Ctrl Pts',(0.977571682500778,-1.7401856658522,33.7861649494306));
#19509=CARTESIAN_POINT('Ctrl Pts',(1.03715181149552,-1.70392009273075,33.7906042926193));
#19510=CARTESIAN_POINT('Ctrl Pts',(1.096714603681,-1.66766507227736,33.7950423440343));
#19511=CARTESIAN_POINT('Ctrl Pts',(1.15439268491689,-1.62827189781196,33.7994803954494));
#19512=CARTESIAN_POINT('Ctrl Pts',(1.20984454305707,-1.58597091528661,33.8039184468644));
#19513=CARTESIAN_POINT('Ctrl Pts',(1.26529910674263,-1.54366786885876,33.8083567148159));
#19514=CARTESIAN_POINT('Ctrl Pts',(1.31852684390637,-1.49845703151792,33.8127949827673));
#19515=CARTESIAN_POINT('Ctrl Pts',(1.36921814456832,-1.45060995277328,33.8172332507188));
#19516=CARTESIAN_POINT('Ctrl Pts',(1.41996314308366,-1.40271218909086,33.8216762201765));
#19517=CARTESIAN_POINT('Ctrl Pts',(1.46816598550494,-1.35217294681108,33.8261191896341));
#19518=CARTESIAN_POINT('Ctrl Pts',(1.51355358694689,-1.29930100513322,33.8305621590917));
#19519=CARTESIAN_POINT('Ctrl Pts',(1.55896768166696,-1.24639820147961,33.835007721963));
#19520=CARTESIAN_POINT('Ctrl Pts',(1.6015629655884,-1.19116037605976,33.8394532848343));
#19521=CARTESIAN_POINT('Ctrl Pts',(1.64110810670013,-1.13392757468152,33.8438988477056));
#19522=CARTESIAN_POINT('Ctrl Pts',(1.68072224881724,-1.07659490968604,33.8483521674921));
#19523=CARTESIAN_POINT('Ctrl Pts',(1.71727536752212,-1.01726073685655,33.8528054872787));
#19524=CARTESIAN_POINT('Ctrl Pts',(1.75058113030047,-0.956291414128532,
33.8572588070652));
#19525=CARTESIAN_POINT('Ctrl Pts',(1.76841224864826,-0.923649879497329,
33.8596430092431));
#19526=CARTESIAN_POINT('Ctrl Pts',(1.78531339333716,-0.890540044050332,
33.8620272114211));
#19527=CARTESIAN_POINT('Ctrl Pts',(1.8012617026036,-0.857020327199758,33.864411413599));
#19528=CARTESIAN_POINT('Ctrl Pts',(1.83105457641699,-0.794402486166849,
33.8688653173606));
#19529=CARTESIAN_POINT('Ctrl Pts',(1.85763737455939,-0.730105192486759,
33.8733192211222));
#19530=CARTESIAN_POINT('Ctrl Pts',(1.88081888573508,-0.664490693360145,
33.8777731248838));
#19531=CARTESIAN_POINT('Ctrl Pts',(1.90396554960781,-0.598974828369706,
33.882220333373));
#19532=CARTESIAN_POINT('Ctrl Pts',(1.92372091264796,-0.5321461457421,33.8866675418621));
#19533=CARTESIAN_POINT('Ctrl Pts',(1.93994081409499,-0.464389061357482,
33.8911147503512));
#19534=CARTESIAN_POINT('Ctrl Pts',(1.95614159485253,-0.396711851821363,
33.8955567162874));
#19535=CARTESIAN_POINT('Ctrl Pts',(1.96881507824126,-0.328108888057713,
33.8999986822235));
#19536=CARTESIAN_POINT('Ctrl Pts',(1.97786671959277,-0.258980312045775,
33.9044406481597));
#19537=CARTESIAN_POINT('Ctrl Pts',(1.98691265161891,-0.189895338902946,
33.9088798123246));
#19538=CARTESIAN_POINT('Ctrl Pts',(1.99234121005921,-0.120285895512519,
33.9133189764894));
#19539=CARTESIAN_POINT('Ctrl Pts',(1.99410910129579,-0.0505613946535523,
33.9177581406543));
#19540=CARTESIAN_POINT('Ctrl Pts',(1.99587647826414,0.0191428237954161,
33.9221960134948));
#19541=CARTESIAN_POINT('Ctrl Pts',(1.99398528954515,0.0889615440849342,
33.9266338863353));
#19542=CARTESIAN_POINT('Ctrl Pts',(1.98844429554399,0.158482951823095,33.9310717591758));
#19543=CARTESIAN_POINT('Ctrl Pts',(1.98290303029309,0.228007762861112,33.9355098492646));
#19544=CARTESIAN_POINT('Ctrl Pts',(1.97371164631804,0.29723474459686,33.9399479393535));
#19545=CARTESIAN_POINT('Ctrl Pts',(1.96093081847343,0.365756596196353,33.9443860294423));
#19546=CARTESIAN_POINT('Ctrl Pts',(1.94813644461477,0.434351072040158,33.9488288233291));
#19547=CARTESIAN_POINT('Ctrl Pts',(1.93174512355498,0.502238443828767,33.9532716172158));
#19548=CARTESIAN_POINT('Ctrl Pts',(1.91186860645616,0.5690219627988,33.9577144111025));
#19549=CARTESIAN_POINT('Ctrl Pts',(1.89198048210503,0.635844481214783,33.9621597994392));
#19550=CARTESIAN_POINT('Ctrl Pts',(1.8686032749491,0.701561402368177,33.9666051877759));
#19551=CARTESIAN_POINT('Ctrl Pts',(1.84189762901384,0.765794154282464,33.9710505761126));
#19552=CARTESIAN_POINT('Ctrl Pts',(1.81514536254822,0.830139038476509,33.9755037248443));
#19553=CARTESIAN_POINT('Ctrl Pts',(1.7850532698749,0.892994139906103,33.9799568735761));
#19554=CARTESIAN_POINT('Ctrl Pts',(1.75182848002257,0.954004475399262,33.9844100223078));
#19555=CARTESIAN_POINT('Ctrl Pts',(1.73402813618776,0.986691061351559,33.9867958185438));
#19556=CARTESIAN_POINT('Ctrl Pts',(1.71532936098203,1.0188486135646,33.9891816147798));
#19557=CARTESIAN_POINT('Ctrl Pts',(1.69576897131637,1.05042617942462,33.9915674110159));
#19558=CARTESIAN_POINT('Ctrl Pts',(1.65925073909999,1.10937985583984,33.9960215687529));
#19559=CARTESIAN_POINT('Ctrl Pts',(1.61958223217014,1.16654365376695,34.0004757264899));
#19560=CARTESIAN_POINT('Ctrl Pts',(1.57696452361047,1.22156066315759,34.0049298842269));
#19561=CARTESIAN_POINT('Ctrl Pts',(1.53441088249247,1.27649496516767,34.0093773460034));
#19562=CARTESIAN_POINT('Ctrl Pts',(1.48891713659827,1.32928850014793,34.01382480778));
#19563=CARTESIAN_POINT('Ctrl Pts',(1.44072846985315,1.37961191595847,34.0182722695565));
#19564=CARTESIAN_POINT('Ctrl Pts',(1.39259663060365,1.4298759868258,34.0227144865705));
#19565=CARTESIAN_POINT('Ctrl Pts',(1.34177651944681,1.47767537213732,34.0271567035845));
#19566=CARTESIAN_POINT('Ctrl Pts',(1.28855340351047,1.52271392218026,34.0315989205985));
#19567=CARTESIAN_POINT('Ctrl Pts',(1.23536387415241,1.56772405053537,34.0360383343405));
#19568=CARTESIAN_POINT('Ctrl Pts',(1.17977472107642,1.60997648432446,34.0404777480826));
#19569=CARTESIAN_POINT('Ctrl Pts',(1.12210675304697,1.64921314488649,34.0449171618246));
#19570=CARTESIAN_POINT('Ctrl Pts',(1.06445558341301,1.68843837600225,34.0493552823872));
#19571=CARTESIAN_POINT('Ctrl Pts',(1.00472720546485,1.72464930257842,34.0537934029498));
#19572=CARTESIAN_POINT('Ctrl Pts',(0.943272629597239,1.75763031060366,34.0582315235125));
#19573=CARTESIAN_POINT('Ctrl Pts',(0.881815076112263,1.79061291663557,34.0626698591124));
#19574=CARTESIAN_POINT('Ctrl Pts',(0.818631591127086,1.82036506402963,34.0671081947123));
#19575=CARTESIAN_POINT('Ctrl Pts',(0.754097497826226,1.84671722964622,34.0715465303122));
#19576=CARTESIAN_POINT('Ctrl Pts',(0.689495083339709,1.87309729386816,34.0759895647052));
#19577=CARTESIAN_POINT('Ctrl Pts',(0.623539660697206,1.8960700064328,34.0804325990982));
#19578=CARTESIAN_POINT('Ctrl Pts',(0.556625335339389,1.91551449969931,34.0848756334912));
#19579=CARTESIAN_POINT('Ctrl Pts',(0.489671973567971,1.93497033647526,34.0893212598572));
#19580=CARTESIAN_POINT('Ctrl Pts',(0.421759072401971,1.95089374536216,34.0937668862232));
#19581=CARTESIAN_POINT('Ctrl Pts',(0.353291928434141,1.96321480633253,34.0982125125893));
#19582=CARTESIAN_POINT('Ctrl Pts',(0.284705364897139,1.97555735754929,34.1026658929634));
#19583=CARTESIAN_POINT('Ctrl Pts',(0.215563114473331,1.98428495719858,34.1071192733375));
#19584=CARTESIAN_POINT('Ctrl Pts',(0.146275810991793,1.98937953885595,34.1115726537115));
#19585=CARTESIAN_POINT('Ctrl Pts',(0.109191134419718,1.99210631423239,34.1139562386185));
#19586=CARTESIAN_POINT('Ctrl Pts',(0.0720649142995155,1.99379322580034,
34.1163398235255));
#19587=CARTESIAN_POINT('Ctrl Pts',(0.0349597448561959,1.9944436263629,34.1187234084326));
#19588=CARTESIAN_POINT('Ctrl Pts',(-0.0343799075217012,1.99565905131826,
34.1231776920632));
#19589=CARTESIAN_POINT('Ctrl Pts',(-0.10392021778134,1.9932565351573,34.1276319756939));
#19590=CARTESIAN_POINT('Ctrl Pts',(-0.17325222182456,1.98721192381005,34.1320862593246));
#19591=CARTESIAN_POINT('Ctrl Pts',(-0.242480051178027,1.98117639478375,
34.1365338501786));
#19592=CARTESIAN_POINT('Ctrl Pts',(-0.311499711845586,1.9715096741866,34.1409814410327));
#19593=CARTESIAN_POINT('Ctrl Pts',(-0.37990153137552,1.95823961479655,34.1454290318868));
#19594=CARTESIAN_POINT('Ctrl Pts',(-0.448222751080454,1.94498519189793,
34.149871382017));
#19595=CARTESIAN_POINT('Ctrl Pts',(-0.515927097368923,1.92813595593716,
34.1543137321473));
#19596=CARTESIAN_POINT('Ctrl Pts',(-0.582611114921541,1.90777143580406,
34.1587560822775));
#19597=CARTESIAN_POINT('Ctrl Pts',(-0.649253088917247,1.8874197552822,34.1631956315537));
#19598=CARTESIAN_POINT('Ctrl Pts',(-0.714875543284826,1.86355732997129,
34.1676351808299));
#19599=CARTESIAN_POINT('Ctrl Pts',(-0.779087791852975,1.83631418201942,
34.1720747301061));
#19600=CARTESIAN_POINT('Ctrl Pts',(-0.843281368037742,1.80907895614651,
34.1765129883986));
#19601=CARTESIAN_POINT('Ctrl Pts',(-0.906065102103133,1.77846515030744,
34.1809512466911));
#19602=CARTESIAN_POINT('Ctrl Pts',(-0.967067661529605,1.74465116872218,
34.1853895049836));
#19603=CARTESIAN_POINT('Ctrl Pts',(-1.02807320373831,1.71083553376787,34.1898279802893));
#19604=CARTESIAN_POINT('Ctrl Pts',(-1.08729697143131,1.67381965180757,34.1942664555949));
#19605=CARTESIAN_POINT('Ctrl Pts',(-1.1443932222072,1.63382732118979,34.1987049309006));
#19606=CARTESIAN_POINT('Ctrl Pts',(-1.20154994366482,1.59379263466487,34.2031481069987));
#19607=CARTESIAN_POINT('Ctrl Pts',(-1.2565742490851,1.5507754889082,34.2075912830969));
#19608=CARTESIAN_POINT('Ctrl Pts',(-1.30915113609228,1.50504181515607,34.2120344591951));
#19609=CARTESIAN_POINT('Ctrl Pts',(-1.36175871028376,1.45928144835013,34.2164802286108));
#19610=CARTESIAN_POINT('Ctrl Pts',(-1.41191567077529,1.41080173799901,34.2209259980265));
#19611=CARTESIAN_POINT('Ctrl Pts',(-1.45934379181443,1.35990560694215,34.2253717674422));
#19612=CARTESIAN_POINT('Ctrl Pts',(-1.50685463944364,1.30892070021216,34.2298252913996));
#19613=CARTESIAN_POINT('Ctrl Pts',(-1.5516268317956,1.25551133426671,34.2342788153571));
#19614=CARTESIAN_POINT('Ctrl Pts',(-1.593422850475,1.20001299246472,34.2387323393145));
#19615=CARTESIAN_POINT('Ctrl Pts',(-1.61578109451182,1.17032486644569,34.2411146948261));
#19616=CARTESIAN_POINT('Ctrl Pts',(-1.63728842812581,1.14003945522088,34.2434970503377));
#19617=CARTESIAN_POINT('Ctrl Pts',(-1.65791382994515,1.10921111379963,34.2458794058494));
#19618=CARTESIAN_POINT('Ctrl Pts',(-1.69713998942199,1.05058062273872,34.2504102585352));
#19619=CARTESIAN_POINT('Ctrl Pts',(-1.733325150733,0.989758288018983,34.254941111221));
#19620=CARTESIAN_POINT('Ctrl Pts',(-1.76622165703498,0.92708609132087,34.2594719639068));
#19621=CARTESIAN_POINT('Ctrl Pts',(-1.79906366234615,0.864517726220709,
34.2639953101432));
#19622=CARTESIAN_POINT('Ctrl Pts',(-1.82862761784535,0.800105995961701,
34.2685186563796));
#19623=CARTESIAN_POINT('Ctrl Pts',(-1.85470920879811,0.734221569622887,
34.273042002616));
#19624=CARTESIAN_POINT('Ctrl Pts',(-1.8807485039618,0.668443986221841,34.2775580134678));
#19625=CARTESIAN_POINT('Ctrl Pts',(-1.90331649425586,0.601198888278888,
34.2820740243197));
#19626=CARTESIAN_POINT('Ctrl Pts',(-1.92225567913312,0.532879598540311,
34.2865900351716));
#19627=CARTESIAN_POINT('Ctrl Pts',(-1.94117680917022,0.464625437996232,
34.2911017408829));
#19628=CARTESIAN_POINT('Ctrl Pts',(-1.95647587983171,0.39529956803751,34.2956134465941));
#19629=CARTESIAN_POINT('Ctrl Pts',(-1.96804458239084,0.325312287228828,
34.3001251523054));
#19630=CARTESIAN_POINT('Ctrl Pts',(-1.97960545955663,0.255372347770581,
34.304633806173));
#19631=CARTESIAN_POINT('Ctrl Pts',(-1.98744090670197,0.184772346772902,
34.3091424600406));
#19632=CARTESIAN_POINT('Ctrl Pts',(-1.99149360991236,0.113933156623746,
34.3136511139081));
#19633=CARTESIAN_POINT('Ctrl Pts',(-1.9936819942071,0.0756813125761565,
34.3160857030705));
#19634=CARTESIAN_POINT('Ctrl Pts',(-1.99476829178972,0.0373598817098916,
34.3185202922328));
#19635=CARTESIAN_POINT('Ctrl Pts',(-1.99474976696403,-0.000964207945006128,
34.3209548813952));
#19636=CARTESIAN_POINT('',(-1.16030843567301,1.62256337213868,34.9999520653248));
#19637=CARTESIAN_POINT('Ctrl Pts',(-1.9947497669637,-0.00096420862522321,
34.3209548814384));
#19638=CARTESIAN_POINT('Ctrl Pts',(-1.99471265556682,-0.0777400726253646,
34.3258321711043));
#19639=CARTESIAN_POINT('Ctrl Pts',(-1.99023883824554,-0.154367005048329,
34.3307094607701));
#19640=CARTESIAN_POINT('Ctrl Pts',(-1.98140456893308,-0.230355153428635,
34.335586750436));
#19641=CARTESIAN_POINT('Ctrl Pts',(-1.97254063423816,-0.30659846920353,
34.3404804179887));
#19642=CARTESIAN_POINT('Ctrl Pts',(-1.95928705017002,-0.38219840303128,
34.3453740855414));
#19643=CARTESIAN_POINT('Ctrl Pts',(-1.94177087878681,-0.456676490303058,
34.3502677530941));
#19644=CARTESIAN_POINT('Ctrl Pts',(-1.92417266464279,-0.531503420239455,
34.3551843417514));
#19645=CARTESIAN_POINT('Ctrl Pts',(-1.90227198517125,-0.605197678237932,
34.3601009304088));
#19646=CARTESIAN_POINT('Ctrl Pts',(-1.87624600475734,-0.677294981623315,
34.3650175190661));
#19647=CARTESIAN_POINT('Ctrl Pts',(-1.8620984381082,-0.71648664274984,34.3676901471327));
#19648=CARTESIAN_POINT('Ctrl Pts',(-1.84673269201964,-0.755206801789487,
34.3703627751993));
#19649=CARTESIAN_POINT('Ctrl Pts',(-1.83018292208798,-0.793383913498066,
34.373035403266));
#19650=CARTESIAN_POINT('Ctrl Pts',(-1.80259560204012,-0.85702251412856,
34.377490489116));
#19651=CARTESIAN_POINT('Ctrl Pts',(-1.77163055517923,-0.91934631967445,
34.3819455749659));
#19652=CARTESIAN_POINT('Ctrl Pts',(-1.73743506938649,-0.97997292930262,
34.3864006608159));
#19653=CARTESIAN_POINT('Ctrl Pts',(-1.70329101030457,-1.0405083623603,34.3908490466467));
#19654=CARTESIAN_POINT('Ctrl Pts',(-1.66592639331255,-1.09935124275348,
34.3952974324775));
#19655=CARTESIAN_POINT('Ctrl Pts',(-1.62553614436603,-1.15614004595448,
34.3997458183083));
#19656=CARTESIAN_POINT('Ctrl Pts',(-1.58519361041228,-1.21286176174194,
34.4041889490415));
#19657=CARTESIAN_POINT('Ctrl Pts',(-1.54183282594229,-1.26753382310107,
34.4086320797747));
#19658=CARTESIAN_POINT('Ctrl Pts',(-1.49569318826118,-1.31982174898322,
34.413075210508));
#19659=CARTESIAN_POINT('Ctrl Pts',(-1.44958273259949,-1.37207660422707,
34.4175155310864));
#19660=CARTESIAN_POINT('Ctrl Pts',(-1.40069723335661,-1.4219499493231,34.4219558516647));
#19661=CARTESIAN_POINT('Ctrl Pts',(-1.34931677363553,-1.46913981869861,
34.4263961722431));
#19662=CARTESIAN_POINT('Ctrl Pts',(-1.29795137218619,-1.51631585795506,
34.4308351914794));
#19663=CARTESIAN_POINT('Ctrl Pts',(-1.24409282204039,-1.56080965193312,
34.4352742107157));
#19664=CARTESIAN_POINT('Ctrl Pts',(-1.18805724768196,-1.60235686996698,
34.439713229952));
#19665=CARTESIAN_POINT('Ctrl Pts',(-1.13201907811547,-1.64390601220124,
34.4441524547752));
#19666=CARTESIAN_POINT('Ctrl Pts',(-1.07380407864231,-1.68250801803604,
34.4485916795984));
#19667=CARTESIAN_POINT('Ctrl Pts',(-1.01375911693235,-1.71794063207567,
34.4530309044215));
#19668=CARTESIAN_POINT('Ctrl Pts',(-0.953650873833102,-1.75341058854967,
34.4574748077441));
#19669=CARTESIAN_POINT('Ctrl Pts',(-0.891709241334137,-1.78570423707937,
34.4619187110666));
#19670=CARTESIAN_POINT('Ctrl Pts',(-0.828306730700667,-1.81464473723536,
34.4663626143891));
#19671=CARTESIAN_POINT('Ctrl Pts',(-0.764867385275751,-1.84360205087833,
34.4708090994746));
#19672=CARTESIAN_POINT('Ctrl Pts',(-0.69996592770663,-1.86920215899221,
34.47525558456));
#19673=CARTESIAN_POINT('Ctrl Pts',(-0.633993340275247,-1.89131700330395,
34.4797020696455));
#19674=CARTESIAN_POINT('Ctrl Pts',(-0.567906077397025,-1.91347028827343,
34.4841562837391));
#19675=CARTESIAN_POINT('Ctrl Pts',(-0.500744439430113,-1.93212608515629,
34.4886104978327));
#19676=CARTESIAN_POINT('Ctrl Pts',(-0.432912218806348,-1.94720686453909,
34.4930647119262));
#19677=CARTESIAN_POINT('Ctrl Pts',(-0.396735307541797,-1.95524988616679,
34.4954402748451));
#19678=CARTESIAN_POINT('Ctrl Pts',(-0.360367794428594,-1.96227690747146,
34.4978158377639));
#19679=CARTESIAN_POINT('Ctrl Pts',(-0.323871455628267,-1.96828220606935,
34.5001914006828));
#19680=CARTESIAN_POINT('Ctrl Pts',(-0.255423773340099,-1.97954494594918,
34.5046466907549));
#19681=CARTESIAN_POINT('Ctrl Pts',(-0.186253044807938,-1.98725518410221,
34.509101980827));
#19682=CARTESIAN_POINT('Ctrl Pts',(-0.116760612552631,-1.99132983753479,
34.513557270899));
#19683=CARTESIAN_POINT('Ctrl Pts',(-0.047372351829141,-1.99539838292256,
34.518005882339));
#19684=CARTESIAN_POINT('Ctrl Pts',(0.0223361710133283,-1.99584213204487,
34.5224544937789));
#19685=CARTESIAN_POINT('Ctrl Pts',(0.0919553937863713,-1.99262936043149,
34.5269031052189));
#19686=CARTESIAN_POINT('Ctrl Pts',(0.161492848290692,-1.98942036224104,
34.5313464917333));
#19687=CARTESIAN_POINT('Ctrl Pts',(0.230940724665639,-1.98256339552903,
34.5357898782477));
#19688=CARTESIAN_POINT('Ctrl Pts',(0.299888137154537,-1.97207876812616,
34.5402332647621));
#19689=CARTESIAN_POINT('Ctrl Pts',(0.368792231432232,-1.96160072799448,
34.5446738595901));
#19690=CARTESIAN_POINT('Ctrl Pts',(0.43719600303466,-1.9474996220327,34.549114454418));
#19691=CARTESIAN_POINT('Ctrl Pts',(0.504693894637496,-1.92984756787049,
34.553555049246));
#19692=CARTESIAN_POINT('Ctrl Pts',(0.572172277537509,-1.91220061562585,
34.5579943606229));
#19693=CARTESIAN_POINT('Ctrl Pts',(0.638744827134744,-1.89100487635706,
34.5624336719997));
#19694=CARTESIAN_POINT('Ctrl Pts',(0.704018131739629,-1.86638314198394,
34.5668729833766));
#19695=CARTESIAN_POINT('Ctrl Pts',(0.769294714033395,-1.84176017123424,
34.5713125176728));
#19696=CARTESIAN_POINT('Ctrl Pts',(0.833271464898335,-1.81371103872464,
34.575752051969));
#19697=CARTESIAN_POINT('Ctrl Pts',(0.895573718238352,-1.78240715822753,
34.5801915862651));
#19698=CARTESIAN_POINT('Ctrl Pts',(0.957941961885542,-1.75107012078057,
34.584635822899));
#19699=CARTESIAN_POINT('Ctrl Pts',(1.01863172991866,-1.71647167455104,34.5890800595328));
#19700=CARTESIAN_POINT('Ctrl Pts',(1.07729266710847,-1.6788293754561,34.5935242961666));
#19701=CARTESIAN_POINT('Ctrl Pts',(1.13598786669948,-1.64116509042613,34.5979711285691));
#19702=CARTESIAN_POINT('Ctrl Pts',(1.19265147936601,-1.60045369941489,34.6024179609715));
#19703=CARTESIAN_POINT('Ctrl Pts',(1.24696417519628,-1.55695469050229,34.606864793374));
#19704=CARTESIAN_POINT('Ctrl Pts',(1.30137148969778,-1.51337990154673,34.611319372646));
#19705=CARTESIAN_POINT('Ctrl Pts',(1.35341934660795,-1.46700812593735,34.6157739519181));
#19706=CARTESIAN_POINT('Ctrl Pts',(1.40282397179528,-1.41813697034402,34.6202285311901));
#19707=CARTESIAN_POINT('Ctrl Pts',(1.42914182958744,-1.39210329195526,34.6226014868266));
#19708=CARTESIAN_POINT('Ctrl Pts',(1.45471028111584,-1.36536095652903,34.624974442463));
#19709=CARTESIAN_POINT('Ctrl Pts',(1.47949120731261,-1.33795864285286,34.6273473980995));
#19710=CARTESIAN_POINT('Ctrl Pts',(1.52593847306427,-1.28659807079754,34.6317950648327));
#19711=CARTESIAN_POINT('Ctrl Pts',(1.56980163759792,-1.23271251372547,34.636242731566));
#19712=CARTESIAN_POINT('Ctrl Pts',(1.61079377487083,-1.17659295312244,34.6406903982992));
#19713=CARTESIAN_POINT('Ctrl Pts',(1.65172406374089,-1.12055806498156,34.6451313544508));
#19714=CARTESIAN_POINT('Ctrl Pts',(1.68979163478545,-1.06229625582543,34.6495723106023));
#19715=CARTESIAN_POINT('Ctrl Pts',(1.72474820872218,-1.00213331399053,34.6540132667539));
#19716=CARTESIAN_POINT('Ctrl Pts',(1.75966357094895,-0.942041300665758,
34.6584489872838));
#19717=CARTESIAN_POINT('Ctrl Pts',(1.79147497428993,-0.880053028291464,
34.6628847078137));
#19718=CARTESIAN_POINT('Ctrl Pts',(1.81997711231644,-0.816523651307357,
34.6673204283436));
#19719=CARTESIAN_POINT('Ctrl Pts',(1.84846129529373,-0.753034294938201,
34.6717533545715));
#19720=CARTESIAN_POINT('Ctrl Pts',(1.87364014748911,-0.688006206665749,
34.6761862807994));
#19721=CARTESIAN_POINT('Ctrl Pts',(1.89535477332313,-0.621818177396922,
34.6806192070273));
#19722=CARTESIAN_POINT('Ctrl Pts',(1.9170631539046,-0.555649184189858,34.6850508583199));
#19723=CARTESIAN_POINT('Ctrl Pts',(1.93530913278304,-0.488321378574417,
34.6894825096125));
#19724=CARTESIAN_POINT('Ctrl Pts',(1.94998297916001,-0.420230821675738,
34.6939141609051));
#19725=CARTESIAN_POINT('Ctrl Pts',(1.96465762871941,-0.352136537796549,
34.6983460547669));
#19726=CARTESIAN_POINT('Ctrl Pts',(1.97575965651884,-0.283279900342223,
34.7027779486288));
#19727=CARTESIAN_POINT('Ctrl Pts',(1.98323035560277,-0.214067557363853,
34.7072098424907));
#19728=CARTESIAN_POINT('Ctrl Pts',(1.99070911917502,-0.144780500877922,
34.7116465205041));
#19729=CARTESIAN_POINT('Ctrl Pts',(1.9945486774022,-0.0751374617397534,
34.7160831985174));
#19730=CARTESIAN_POINT('Ctrl Pts',(1.99474228008966,-0.00554964167354013,
34.7205198765308));
#19731=CARTESIAN_POINT('Ctrl Pts',(1.99493599756775,0.0640794383063369,
34.7249591851332));
#19732=CARTESIAN_POINT('Ctrl Pts',(1.9914794819098,0.133652743457299,34.7293984937355));
#19733=CARTESIAN_POINT('Ctrl Pts',(1.9844180350377,0.202762483504982,34.7338378023379));
#19734=CARTESIAN_POINT('Ctrl Pts',(1.97734405078291,0.271994925779874,34.7382849927967));
#19735=CARTESIAN_POINT('Ctrl Pts',(1.9666524348556,0.340761674904844,34.7427321832556));
#19736=CARTESIAN_POINT('Ctrl Pts',(1.95243978435104,0.408664227677522,34.7471793737144));
#19737=CARTESIAN_POINT('Ctrl Pts',(1.94463757281088,0.445940179877938,34.749620714315));
#19738=CARTESIAN_POINT('Ctrl Pts',(1.9357751503674,0.482955942038886,34.7520620549156));
#19739=CARTESIAN_POINT('Ctrl Pts',(1.92587478566871,0.51964783500513,34.7545033955163));
#19740=CARTESIAN_POINT('Ctrl Pts',(1.90777717078887,0.586719682186929,34.7589661040452));
#19741=CARTESIAN_POINT('Ctrl Pts',(1.88613631026345,0.652975618589625,34.7634288125741));
#19742=CARTESIAN_POINT('Ctrl Pts',(1.86104327560504,0.718014964207053,34.7678915211031));
#19743=CARTESIAN_POINT('Ctrl Pts',(1.8359880405527,0.782956335957365,34.7723475071042));
#19744=CARTESIAN_POINT('Ctrl Pts',(1.80749112789103,0.846684303467218,34.7768034931053));
#19745=CARTESIAN_POINT('Ctrl Pts',(1.77569375150756,0.908812006609178,34.7812594791064));
#19746=CARTESIAN_POINT('Ctrl Pts',(1.7439343727898,0.97086546753483,34.7857101402321));
#19747=CARTESIAN_POINT('Ctrl Pts',(1.70888258594342,1.03132203083621,34.7901608013578));
#19748=CARTESIAN_POINT('Ctrl Pts',(1.6707275031139,1.08981520123312,34.7946114624835));
#19749=CARTESIAN_POINT('Ctrl Pts',(1.6325969197808,1.14827081298483,34.799059265826));
#19750=CARTESIAN_POINT('Ctrl Pts',(1.59136725968048,1.204765125754,34.8035070691685));
#19751=CARTESIAN_POINT('Ctrl Pts',(1.54727259043397,1.25895793948477,34.8079548725109));
#19752=CARTESIAN_POINT('Ctrl Pts',(1.50319140356955,1.31313418322571,34.8124013158935));
#19753=CARTESIAN_POINT('Ctrl Pts',(1.45624725429879,1.36500994711715,34.816847759276));
#19754=CARTESIAN_POINT('Ctrl Pts',(1.40671532481837,1.41427704408336,34.8212942026585));
#19755=CARTESIAN_POINT('Ctrl Pts',(1.35718188120189,1.46354564708998,34.8257407819639));
#19756=CARTESIAN_POINT('Ctrl Pts',(1.30506084762024,1.51020508270624,34.8301873612692));
#19757=CARTESIAN_POINT('Ctrl Pts',(1.25066393995028,1.55398432160947,34.8346339405746));
#19758=CARTESIAN_POINT('Ctrl Pts',(1.19621170013645,1.59780809244015,34.8390850429085));
#19759=CARTESIAN_POINT('Ctrl Pts',(1.13947934586028,1.63874551236705,34.8435361452424));
#19760=CARTESIAN_POINT('Ctrl Pts',(1.08081056994716,1.67656675214275,34.8479872475763));
#19761=CARTESIAN_POINT('Ctrl Pts',(1.02210879094863,1.71440926759,34.8524408537994));
#19762=CARTESIAN_POINT('Ctrl Pts',(0.961468844825503,1.74913187044876,34.8568944600224));
#19763=CARTESIAN_POINT('Ctrl Pts',(0.899259836826005,1.78055028246092,34.8613480662454));
#19764=CARTESIAN_POINT('Ctrl Pts',(0.83694561152002,1.81202183405516,34.8658092050826));
#19765=CARTESIAN_POINT('Ctrl Pts',(0.773057472579082,1.84017784161958,34.8702703439197));
#19766=CARTESIAN_POINT('Ctrl Pts',(0.707984590213472,1.86488213636151,34.8747314827568));
#19767=CARTESIAN_POINT('Ctrl Pts',(0.674299687442788,1.87767028614293,34.8770407861489));
#19768=CARTESIAN_POINT('Ctrl Pts',(0.640297574963375,1.88953433152249,34.8793500895409));
#19769=CARTESIAN_POINT('Ctrl Pts',(0.606033511339024,1.90046071930837,34.8816593929329));
#19770=CARTESIAN_POINT('Ctrl Pts',(0.540549617409981,1.92134272637685,34.8860728267868));
#19771=CARTESIAN_POINT('Ctrl Pts',(0.473845937994771,1.93888046061422,34.8904862606408));
#19772=CARTESIAN_POINT('Ctrl Pts',(0.406300572580434,1.95293302681398,34.8948996944947));
#19773=CARTESIAN_POINT('Ctrl Pts',(0.338868365116361,1.96696205091611,34.8993057345752));
#19774=CARTESIAN_POINT('Ctrl Pts',(0.270597756009901,1.9775173991392,34.9037117746557));
#19775=CARTESIAN_POINT('Ctrl Pts',(0.20188253232988,1.98450774894936,34.9081178147362));
#19776=CARTESIAN_POINT('Ctrl Pts',(0.13323170122176,1.99149154814995,34.9125197259463));
#19777=CARTESIAN_POINT('Ctrl Pts',(0.064137575514188,1.99491692021807,34.9169216371564));
#19778=CARTESIAN_POINT('Ctrl Pts',(-0.00499674790325566,1.99474374168974,
34.9213235483666));
#19779=CARTESIAN_POINT('Ctrl Pts',(-0.0740908315086826,1.99457066396042,
34.9257228974328));
#19780=CARTESIAN_POINT('Ctrl Pts',(-0.143224568111221,1.99080319031719,
34.9301222464991));
#19781=CARTESIAN_POINT('Ctrl Pts',(-0.211992548267063,1.98345323160876,
34.9345215955654));
#19782=CARTESIAN_POINT('Ctrl Pts',(-0.280744914779345,1.97610494169496,
34.9389199457676));
#19783=CARTESIAN_POINT('Ctrl Pts',(-0.349131193400388,1.96517583483292,
34.9433182959697));
#19784=CARTESIAN_POINT('Ctrl Pts',(-0.416750710130754,1.95072971169906,
34.9477166461719));
#19785=CARTESIAN_POINT('Ctrl Pts',(-0.4844246825355,1.93627195474386,34.9521185384746));
#19786=CARTESIAN_POINT('Ctrl Pts',(-0.551330169253238,1.91829162441387,
34.9565204307773));
#19787=CARTESIAN_POINT('Ctrl Pts',(-0.617077406011004,1.89690353932158,
34.96092232308));
#19788=CARTESIAN_POINT('Ctrl Pts',(-0.682848740161482,1.87550761516089,
34.9653258287452));
#19789=CARTESIAN_POINT('Ctrl Pts',(-0.74746051103628,1.85070162583077,34.9697293344104));
#19790=CARTESIAN_POINT('Ctrl Pts',(-0.810541566948271,1.82264915185261,
34.9741328400756));
#19791=CARTESIAN_POINT('Ctrl Pts',(-0.873734734060834,1.79454682143988,
34.9785441718988));
#19792=CARTESIAN_POINT('Ctrl Pts',(-0.935391303863738,1.76318670442566,
34.9829555037219));
#19793=CARTESIAN_POINT('Ctrl Pts',(-0.995164032288082,1.72877879190489,
34.9873668355451));
#19794=CARTESIAN_POINT('Ctrl Pts',(-1.05200654243708,1.69605764685722,34.9915619121383));
#19795=CARTESIAN_POINT('Ctrl Pts',(-1.10714529455824,1.66058077235957,34.9957569887316));
#19796=CARTESIAN_POINT('Ctrl Pts',(-1.16030843567301,1.62256337213868,34.9999520653248));
#19797=CARTESIAN_POINT('',(1.16034898466929,1.62253437445157,35.));
#19798=CARTESIAN_POINT('Origin',(0.,0.,35.));
#19799=CARTESIAN_POINT('',(-1.99474961222923,-0.00124378911175134,34.4790451185704));
#19800=CARTESIAN_POINT('Ctrl Pts',(-1.99474961222889,-0.00124378964630918,
34.4790451186047));
#19801=CARTESIAN_POINT('Ctrl Pts',(-1.99470965583835,-0.0653245566594018,
34.4831554158475));
#19802=CARTESIAN_POINT('Ctrl Pts',(-1.99158209595733,-0.129314909989991,
34.4872657130903));
#19803=CARTESIAN_POINT('Ctrl Pts',(-1.9853913538538,-0.192999312285264,
34.4913760103331));
#19804=CARTESIAN_POINT('Ctrl Pts',(-1.97866982777472,-0.262143909766435,
34.4958387176544));
#19805=CARTESIAN_POINT('Ctrl Pts',(-1.96831880424879,-0.331071626911279,
34.5003014249758));
#19806=CARTESIAN_POINT('Ctrl Pts',(-1.95436163129808,-0.399372228140521,
34.5047641322972));
#19807=CARTESIAN_POINT('Ctrl Pts',(-1.94042548309976,-0.467569942973346,
34.5092201171027));
#19808=CARTESIAN_POINT('Ctrl Pts',(-1.92289406513358,-0.535141943202289,
34.5136761019082));
#19809=CARTESIAN_POINT('Ctrl Pts',(-1.90184246552371,-0.601683304430749,
34.5181320867137));
#19810=CARTESIAN_POINT('Ctrl Pts',(-1.88081602234114,-0.668145149472913,
34.522582746667));
#19811=CARTESIAN_POINT('Ctrl Pts',(-1.85627789992849,-0.733578339405207,
34.5270334066202));
#19812=CARTESIAN_POINT('Ctrl Pts',(-1.8283537991141,-0.797590087554399,
34.5314840665735));
#19813=CARTESIAN_POINT('Ctrl Pts',(-1.80044762836177,-0.861560733767165,
34.5359318687585));
#19814=CARTESIAN_POINT('Ctrl Pts',(-1.76915998727677,-0.924111303249376,
34.5403796709435));
#19815=CARTESIAN_POINT('Ctrl Pts',(-1.73466527106065,-0.984867483408844,
34.5448274731285));
#19816=CARTESIAN_POINT('Ctrl Pts',(-1.70018110182025,-1.04560508698538,
34.5492739153701));
#19817=CARTESIAN_POINT('Ctrl Pts',(-1.66249204486713,-1.10454896679754,
34.5537203576116));
#19818=CARTESIAN_POINT('Ctrl Pts',(-1.62181835050051,-1.16134955998606,
34.5581667998532));
#19819=CARTESIAN_POINT('Ctrl Pts',(-1.58114341261805,-1.21815188973769,
34.5626133780358));
#19820=CARTESIAN_POINT('Ctrl Pts',(-1.53748394189366,-1.27281040775946,
34.5670599562184));
#19821=CARTESIAN_POINT('Ctrl Pts',(-1.49110237966126,-1.32500613427581,
34.5715065344009));
#19822=CARTESIAN_POINT('Ctrl Pts',(-1.44467363806279,-1.37725495433127,
34.5759576356467));
#19823=CARTESIAN_POINT('Ctrl Pts',(-1.39551760247024,-1.42703561726791,
34.5804087368925));
#19824=CARTESIAN_POINT('Ctrl Pts',(-1.34393508215423,-1.47406446855458,
34.5848598381383));
#19825=CARTESIAN_POINT('Ctrl Pts',(-1.2923235447832,-1.52111977529083,34.5893134432915));
#19826=CARTESIAN_POINT('Ctrl Pts',(-1.23828318225281,-1.56541987915142,
34.5937670484446));
#19827=CARTESIAN_POINT('Ctrl Pts',(-1.18214741987205,-1.60672183037073,
34.5982206535977));
#19828=CARTESIAN_POINT('Ctrl Pts',(-1.12591671166209,-1.64809363809219,
34.6026817914041));
#19829=CARTESIAN_POINT('Ctrl Pts',(-1.0675839358362,-1.68645690198636,34.6071429292105));
#19830=CARTESIAN_POINT('Ctrl Pts',(-1.00751028473955,-1.72161278708194,
34.6116040670169));
#19831=CARTESIAN_POINT('Ctrl Pts',(-0.976413083945413,-1.73981127507052,
34.6139133805946));
#19832=CARTESIAN_POINT('Ctrl Pts',(-0.944849779950104,-1.75715106896168,
34.6162226941722));
#19833=CARTESIAN_POINT('Ctrl Pts',(-0.912872618442756,-1.77360963715172,
34.6185320077498));
#19834=CARTESIAN_POINT('Ctrl Pts',(-0.851111131992418,-1.80539812582129,
34.6229922735305));
#19835=CARTESIAN_POINT('Ctrl Pts',(-0.787568603186281,-1.83401781075126,
34.6274525393112));
#19836=CARTESIAN_POINT('Ctrl Pts',(-0.722602739111021,-1.85926674899791,
34.6319128050919));
#19837=CARTESIAN_POINT('Ctrl Pts',(-0.657732762387549,-1.88447842069145,
34.6363664876757));
#19838=CARTESIAN_POINT('Ctrl Pts',(-0.591444071614061,-1.90632904581292,
34.6408201702595));
#19839=CARTESIAN_POINT('Ctrl Pts',(-0.524117845427371,-1.92466309950718,
34.6452738528433));
#19840=CARTESIAN_POINT('Ctrl Pts',(-0.456868876270491,-1.94297611482437,
34.6497224248141));
#19841=CARTESIAN_POINT('Ctrl Pts',(-0.388585205056955,-1.95778044624095,
34.6541709967849));
#19842=CARTESIAN_POINT('Ctrl Pts',(-0.319665143225316,-1.96896972010916,
34.6586195687557));
#19843=CARTESIAN_POINT('Ctrl Pts',(-0.25078728816113,-1.98015214164631,
34.6630654164132));
#19844=CARTESIAN_POINT('Ctrl Pts',(-0.181274296205601,-1.98772381995354,
34.6675112640706));
#19845=CARTESIAN_POINT('Ctrl Pts',(-0.111535216559958,-1.99162934753606,
34.6719571117281));
#19846=CARTESIAN_POINT('Ctrl Pts',(-0.041815350350925,-1.99553379912781,
34.6764017345341));
#19847=CARTESIAN_POINT('Ctrl Pts',(0.0281299930082953,-1.99577407809619,
34.6808463573401));
#19848=CARTESIAN_POINT('Ctrl Pts',(0.0978878467608373,-1.99234673989156,
34.6852909801462));
#19849=CARTESIAN_POINT('Ctrl Pts',(0.16764998223558,-1.98891919131764,34.6897358757622));
#19850=CARTESIAN_POINT('Ctrl Pts',(0.237224118103609,-1.98182360491614,
34.6941807713782));
#19851=CARTESIAN_POINT('Ctrl Pts',(0.306200262956401,-1.97110856156261,
34.6986256669942));
#19852=CARTESIAN_POINT('Ctrl Pts',(0.375249952031826,-1.96038209354139,
34.7030753018776));
#19853=CARTESIAN_POINT('Ctrl Pts',(0.443699894468999,-1.94602854096107,
34.707524936761));
#19854=CARTESIAN_POINT('Ctrl Pts',(0.511149113271741,-1.92814785390061,
34.7119745716444));
#19855=CARTESIAN_POINT('Ctrl Pts',(0.578638115626237,-1.91025662028006,
34.7164268310546));
#19856=CARTESIAN_POINT('Ctrl Pts',(0.645124754911799,-1.88883426064622,
34.7208790904648));
#19857=CARTESIAN_POINT('Ctrl Pts',(0.710224732460111,-1.86403014779857,
34.7253313498749));
#19858=CARTESIAN_POINT('Ctrl Pts',(0.775437769193194,-1.83918295762766,
34.7297913415277));
#19859=CARTESIAN_POINT('Ctrl Pts',(0.839258890766058,-1.81094248763635,
34.7342513331804));
#19860=CARTESIAN_POINT('Ctrl Pts',(0.901325948867879,-1.77950529541146,
34.7387113248332));
#19861=CARTESIAN_POINT('Ctrl Pts',(0.933689389379248,-1.76311309427401,
34.7410368849443));
#19862=CARTESIAN_POINT('Ctrl Pts',(0.965576363354185,-1.74585249339734,
34.7433624450554));
#19863=CARTESIAN_POINT('Ctrl Pts',(0.996938704649294,-1.72775599598791,
34.7456880051665));
#19864=CARTESIAN_POINT('Ctrl Pts',(1.0563508981099,-1.69347435244187,34.7500934998304));
#19865=CARTESIAN_POINT('Ctrl Pts',(1.11412509718853,-1.65604807414781,34.7544989944944));
#19866=CARTESIAN_POINT('Ctrl Pts',(1.16990273560751,-1.61565935509874,34.7589044891584));
#19867=CARTESIAN_POINT('Ctrl Pts',(1.2255952124592,-1.57533230174066,34.7633032574919));
#19868=CARTESIAN_POINT('Ctrl Pts',(1.27929677257618,-1.53205206939976,34.7677020258253));
#19869=CARTESIAN_POINT('Ctrl Pts',(1.3306744502896,-1.48604611969026,34.7721007941588));
#19870=CARTESIAN_POINT('Ctrl Pts',(1.38199285826681,-1.44009324284479,34.7764944880348));
#19871=CARTESIAN_POINT('Ctrl Pts',(1.43099233254781,-1.39142122092301,34.7808881819109));
#19872=CARTESIAN_POINT('Ctrl Pts',(1.47737142017283,-1.34029894029522,34.7852818757869));
#19873=CARTESIAN_POINT('Ctrl Pts',(1.52372217860752,-1.28920788608634,34.7896728859148));
#19874=CARTESIAN_POINT('Ctrl Pts',(1.56745538696022,-1.23566990986244,34.7940638960427));
#19875=CARTESIAN_POINT('Ctrl Pts',(1.60830629585188,-1.17999085641509,34.7984549061706));
#19876=CARTESIAN_POINT('Ctrl Pts',(1.64914684967132,-1.12432591674476,34.8028448032455));
#19877=CARTESIAN_POINT('Ctrl Pts',(1.68710625695501,-1.06652138023251,34.8072347003204));
#19878=CARTESIAN_POINT('Ctrl Pts',(1.72196116123219,-1.00691475394291,34.8116245973952));
#19879=CARTESIAN_POINT('Ctrl Pts',(1.75681968526789,-0.947301937373964,
34.8160149503706));
#19880=CARTESIAN_POINT('Ctrl Pts',(1.78857281587677,-0.885887093569423,
34.820405303346));
#19881=CARTESIAN_POINT('Ctrl Pts',(1.81704249578212,-0.823033493256425,
34.8247956563213));
#19882=CARTESIAN_POINT('Ctrl Pts',(1.84554707497725,-0.760102844447701,
34.8291913911697));
#19883=CARTESIAN_POINT('Ctrl Pts',(1.87075996451608,-0.695730377162034,
34.833587126018));
#19884=CARTESIAN_POINT('Ctrl Pts',(1.89255117354373,-0.63029962558949,34.8379828608663));
#19885=CARTESIAN_POINT('Ctrl Pts',(1.91435672909789,-0.564825796828756,
34.842381489704));
#19886=CARTESIAN_POINT('Ctrl Pts',(1.93273599313613,-0.498292781634358,
34.8467801185417));
#19887=CARTESIAN_POINT('Ctrl Pts',(1.94760963476504,-0.431096593665931,
34.8511787473793));
#19888=CARTESIAN_POINT('Ctrl Pts',(1.96251284200395,-0.363766834085676,
34.8555861197478));
#19889=CARTESIAN_POINT('Ctrl Pts',(1.97389643842135,-0.295771764791792,
34.8599934921164));
#19890=CARTESIAN_POINT('Ctrl Pts',(1.98173280701928,-0.227514052496768,
34.8644008644849));
#19891=CARTESIAN_POINT('Ctrl Pts',(1.98673681218226,-0.183927289001692,
34.867215243851));
#19892=CARTESIAN_POINT('Ctrl Pts',(1.99029545462308,-0.14023349302073,34.8700296232172));
#19893=CARTESIAN_POINT('Ctrl Pts',(1.9924126509726,-0.0965369915853482,
34.8728440025833));
#19894=CARTESIAN_POINT('Ctrl Pts',(1.99585743825963,-0.0254405376988781,
34.8774231424743));
#19895=CARTESIAN_POINT('Ctrl Pts',(1.9954980008896,0.0459551382969561,34.8820022823654));
#19896=CARTESIAN_POINT('Ctrl Pts',(1.99130272330465,0.117222125298427,34.8865814222565));
#19897=CARTESIAN_POINT('Ctrl Pts',(1.98697310365769,0.190771238760697,34.8913071963291));
#19898=CARTESIAN_POINT('Ctrl Pts',(1.97855768336608,0.264182799724639,34.8960329704018));
#19899=CARTESIAN_POINT('Ctrl Pts',(1.96607994072682,0.336982535410391,34.9007587444744));
#19900=CARTESIAN_POINT('Ctrl Pts',(1.95402968050572,0.407288181583975,34.9053226154379));
#19901=CARTESIAN_POINT('Ctrl Pts',(1.93819099945231,0.477022746940168,34.9098864864015));
#19902=CARTESIAN_POINT('Ctrl Pts',(1.91863774874258,0.545762541404237,34.914450357365));
#19903=CARTESIAN_POINT('Ctrl Pts',(1.89910305268284,0.614437106672102,34.9190098975382));
#19904=CARTESIAN_POINT('Ctrl Pts',(1.87586091671168,0.68211833980894,34.9235694377114));
#19905=CARTESIAN_POINT('Ctrl Pts',(1.84903594885902,0.748394028788993,34.9281289778847));
#19906=CARTESIAN_POINT('Ctrl Pts',(1.82222923950999,0.814624607000826,34.9326854145917));
#19907=CARTESIAN_POINT('Ctrl Pts',(1.79184471751014,0.879451120919967,34.9372418512987));
#19908=CARTESIAN_POINT('Ctrl Pts',(1.75805595896161,0.94247907544919,34.9417982880058));
#19909=CARTESIAN_POINT('Ctrl Pts',(1.72428114286142,1.00548102239372,34.9463528445643));
#19910=CARTESIAN_POINT('Ctrl Pts',(1.68710510012319,1.06668548456953,34.9509074011229));
#19911=CARTESIAN_POINT('Ctrl Pts',(1.64674780710277,1.12572164512468,34.9554619576814));
#19912=CARTESIAN_POINT('Ctrl Pts',(1.6063852328958,1.18476553119741,34.9600171102527));
#19913=CARTESIAN_POINT('Ctrl Pts',(1.56284082884428,1.24164016816606,34.9645722628241));
#19914=CARTESIAN_POINT('Ctrl Pts',(1.51637789034378,1.2960037253714,34.9691274153954));
#19915=CARTESIAN_POINT('Ctrl Pts',(1.46991192230367,1.35037082726321,34.973682864978));
#19916=CARTESIAN_POINT('Ctrl Pts',(1.42052734378007,1.40222618176822,34.9782383145605));
#19917=CARTESIAN_POINT('Ctrl Pts',(1.36852654774444,1.45126243340709,34.9827937641431));
#19918=CARTESIAN_POINT('Ctrl Pts',(1.31649062216685,1.50033181186693,34.9873522911951));
#19919=CARTESIAN_POINT('Ctrl Pts',(1.26183528935258,1.54657797917796,34.991910818247));
#19920=CARTESIAN_POINT('Ctrl Pts',(1.20489776833193,1.58973234551252,34.996469345299));
#19921=CARTESIAN_POINT('Ctrl Pts',(1.19019808398469,1.60087360266513,34.9976462301993));
#19922=CARTESIAN_POINT('Ctrl Pts',(1.1753464469573,1.61180899912977,34.9988231150997));
#19923=CARTESIAN_POINT('Ctrl Pts',(1.16034898466929,1.62253437445157,35.));
#19924=CARTESIAN_POINT('',(-1.99474967239366,-0.00114323460825715,33.6790451186519));
#19925=CARTESIAN_POINT('Ctrl Pts',(-1.99474967239366,-0.00114323460825715,
33.6790451186519));
#19926=CARTESIAN_POINT('Ctrl Pts',(-1.99470505520098,-0.0789926365181883,
33.6839926278254));
#19927=CARTESIAN_POINT('Ctrl Pts',(-1.99009895797611,-0.156676925226695,
33.6889401369989));
#19928=CARTESIAN_POINT('Ctrl Pts',(-1.98101371068683,-0.233692619846631,
33.6938876461724));
#19929=CARTESIAN_POINT('Ctrl Pts',(-1.97189090305347,-0.311026713723905,
33.6988556094009));
#19930=CARTESIAN_POINT('Ctrl Pts',(-1.95825197165493,-0.387686411871911,
33.7038235726293));
#19931=CARTESIAN_POINT('Ctrl Pts',(-1.94022999868426,-0.463179354792175,
33.7087915358577));
#19932=CARTESIAN_POINT('Ctrl Pts',(-1.922115047508,-0.539061777731016,33.7137851295932));
#19933=CARTESIAN_POINT('Ctrl Pts',(-1.8995718510703,-0.613765121854765,
33.7187787233288));
#19934=CARTESIAN_POINT('Ctrl Pts',(-1.87278362166587,-0.686810795576234,
33.7237723170643));
#19935=CARTESIAN_POINT('Ctrl Pts',(-1.8644369505841,-0.709570351771406,
33.7253282199871));
#19936=CARTESIAN_POINT('Ctrl Pts',(-1.85567850453098,-0.732169148883617,
33.7268841229099));
#19937=CARTESIAN_POINT('Ctrl Pts',(-1.84651473842679,-0.754593190581943,
33.7284400258326));
#19938=CARTESIAN_POINT('Ctrl Pts',(-1.82028118708606,-0.818787566831978,
33.7328941835165));
#19939=CARTESIAN_POINT('Ctrl Pts',(-1.79064410943348,-0.881739403773629,
33.7373483412003));
#19940=CARTESIAN_POINT('Ctrl Pts',(-1.75774259151952,-0.943063383054522,
33.7418024988842));
#19941=CARTESIAN_POINT('Ctrl Pts',(-1.72489053463828,-1.0042951736603,33.7462499606083));
#19942=CARTESIAN_POINT('Ctrl Pts',(-1.68878400713422,-1.06390353577771,
33.7506974223324));
#19943=CARTESIAN_POINT('Ctrl Pts',(-1.64961016594262,-1.12152301042768,
33.7551448840565));
#19944=CARTESIAN_POINT('Ctrl Pts',(-1.61048252131381,-1.17907453611992,
33.7595871010194));
#19945=CARTESIAN_POINT('Ctrl Pts',(-1.5682950211204,-1.23464142980895,33.7640293179822));
#19946=CARTESIAN_POINT('Ctrl Pts',(-1.52327985760852,-1.28788432629029,
33.7684715349451));
#19947=CARTESIAN_POINT('Ctrl Pts',(-1.47829310101842,-1.34109362372015,
33.7729109486368));
#19948=CARTESIAN_POINT('Ctrl Pts',(-1.43048253628969,-1.39198146031091,
33.7773503623285));
#19949=CARTESIAN_POINT('Ctrl Pts',(-1.38012171989822,-1.44024011913472,
33.7817897760202));
#19950=CARTESIAN_POINT('Ctrl Pts',(-1.32977557335486,-1.48848472045815,
33.7862278965334));
#19951=CARTESIAN_POINT('Ctrl Pts',(-1.27688100314554,-1.53410132585811,
33.7906660170466));
#19952=CARTESIAN_POINT('Ctrl Pts',(-1.22174839272104,-1.57681908517863,
33.7951041375598));
#19953=CARTESIAN_POINT('Ctrl Pts',(-1.16661311098122,-1.61953891428332,
33.7995424731112));
#19954=CARTESIAN_POINT('Ctrl Pts',(-1.10923996216822,-1.65935932051046,
33.8039808086627));
#19955=CARTESIAN_POINT('Ctrl Pts',(-1.049970950935,-1.69605087326196,33.8084191442141));
#19956=CARTESIAN_POINT('Ctrl Pts',(-0.990639192548068,-1.73278127077318,
33.8128621785604));
#19957=CARTESIAN_POINT('Ctrl Pts',(-0.929407982682463,-1.76637594508789,
33.8173052129066));
#19958=CARTESIAN_POINT('Ctrl Pts',(-0.866645918674512,-1.79665033162962,
33.8217482472529));
#19959=CARTESIAN_POINT('Ctrl Pts',(-0.803847240581718,-1.82694237961978,
33.8261938735731));
#19960=CARTESIAN_POINT('Ctrl Pts',(-0.739516382396525,-1.8539100951532,
33.8306394998934));
#19961=CARTESIAN_POINT('Ctrl Pts',(-0.67404142839136,-1.8774172991938,33.8350851262136));
#19962=CARTESIAN_POINT('Ctrl Pts',(-0.608452273729243,-1.90096550422761,
33.8395385065438));
#19963=CARTESIAN_POINT('Ctrl Pts',(-0.541715508565356,-1.92104100824494,
33.843991886874));
#19964=CARTESIAN_POINT('Ctrl Pts',(-0.474233081564563,-1.9375578821934,
33.8484452672042));
#19965=CARTESIAN_POINT('Ctrl Pts',(-0.438114422849897,-1.94639821825853,
33.8508288525526));
#19966=CARTESIAN_POINT('Ctrl Pts',(-0.401782311076133,-1.95421998611483,
33.853212437901));
#19967=CARTESIAN_POINT('Ctrl Pts',(-0.365299029535839,-1.96101610944943,
33.8555960232494));
#19968=CARTESIAN_POINT('Ctrl Pts',(-0.2971215359886,-1.97371624592918,33.860050306632));
#19969=CARTESIAN_POINT('Ctrl Pts',(-0.228146046863805,-1.98288184402868,
33.8645045900147));
#19970=CARTESIAN_POINT('Ctrl Pts',(-0.15877185441207,-1.98842124831399,
33.8689588733973));
#19971=CARTESIAN_POINT('Ctrl Pts',(-0.0895019000726365,-1.99395232937382,
33.8734064640017));
#19972=CARTESIAN_POINT('Ctrl Pts',(-0.0198349153927554,-1.99586799200378,
33.877854054606));
#19973=CARTESIAN_POINT('Ctrl Pts',(0.0498204823198855,-1.9941277496794,
33.8823016452103));
#19974=CARTESIAN_POINT('Ctrl Pts',(0.119393803054987,-1.99238955793307,
33.8867439950895));
#19975=CARTESIAN_POINT('Ctrl Pts',(0.188955076952801,-1.98700402937793,
33.8911863449687));
#19976=CARTESIAN_POINT('Ctrl Pts',(0.258093246057805,-1.97798266899368,
33.8956286948479));
#19977=CARTESIAN_POINT('Ctrl Pts',(0.327187824276703,-1.96896699648195,
33.9000682438724));
#19978=CARTESIAN_POINT('Ctrl Pts',(0.395859342642638,-1.95632010285085,
33.9045077928968));
#19979=CARTESIAN_POINT('Ctrl Pts',(0.463700960007945,-1.94010540491689,
33.9089473419213));
#19980=CARTESIAN_POINT('Ctrl Pts',(0.531522849594134,-1.92389542208246,
33.9133855999617));
#19981=CARTESIAN_POINT('Ctrl Pts',(0.598514841410656,-1.90411980826287,
33.9178238580022));
#19982=CARTESIAN_POINT('Ctrl Pts',(0.664281154596361,-1.88089290235997,
33.9222621160427));
#19983=CARTESIAN_POINT('Ctrl Pts',(0.730050683493869,-1.85766486075352,
33.9267005910963));
#19984=CARTESIAN_POINT('Ctrl Pts',(0.794593954013738,-1.83098535728792,
33.93113906615));
#19985=CARTESIAN_POINT('Ctrl Pts',(0.857532891273935,-1.80101774085748,
33.9355775412037));
#19986=CARTESIAN_POINT('Ctrl Pts',(0.9205384872393,-1.77101838568794,33.9400207170517));
#19987=CARTESIAN_POINT('Ctrl Pts',(0.981935915679973,-1.73772417761029,
33.9444638928997));
#19988=CARTESIAN_POINT('Ctrl Pts',(1.0413704272109,-1.70134511367641,33.9489070687477));
#19989=CARTESIAN_POINT('Ctrl Pts',(1.10083962847878,-1.6649448166218,33.9533528379139));
#19990=CARTESIAN_POINT('Ctrl Pts',(1.15834322883593,-1.62545635715317,33.9577986070802));
#19991=CARTESIAN_POINT('Ctrl Pts',(1.21355661016748,-1.58313231172218,33.9622443762464));
#19992=CARTESIAN_POINT('Ctrl Pts',(1.26886629759555,-1.54073444245526,33.9666978999581));
#19993=CARTESIAN_POINT('Ctrl Pts',(1.32187741951533,-1.49549143189135,33.9711514236697));
#19994=CARTESIAN_POINT('Ctrl Pts',(1.37230010035973,-1.44769471818221,33.9756049473814));
#19995=CARTESIAN_POINT('Ctrl Pts',(1.39927309362224,-1.42212645375722,33.977987305143));
#19996=CARTESIAN_POINT('Ctrl Pts',(1.42550603583875,-1.39582803407515,33.9803696629046));
#19997=CARTESIAN_POINT('Ctrl Pts',(1.45095931925126,-1.36884791572253,33.9827520206661));
#19998=CARTESIAN_POINT('Ctrl Pts',(1.49853658081032,-1.31841669524094,33.9872051223156));
#19999=CARTESIAN_POINT('Ctrl Pts',(1.54357589213584,-1.26540192235272,33.9916582239652));
#20000=CARTESIAN_POINT('Ctrl Pts',(1.58578405289311,-1.21008945954004,33.9961113256147));
#20001=CARTESIAN_POINT('Ctrl Pts',(1.62792873852477,-1.15486017887654,34.0005577304269));
#20002=CARTESIAN_POINT('Ctrl Pts',(1.66725042916285,-1.09734045249745,34.0050041352391));
#20003=CARTESIAN_POINT('Ctrl Pts',(1.70349388381983,-1.03785169956427,34.0094505400512));
#20004=CARTESIAN_POINT('Ctrl Pts',(1.73969461790375,-0.978433066702129,
34.0138917038354));
#20005=CARTESIAN_POINT('Ctrl Pts',(1.77282406866205,-0.917050433091979,
34.0183328676196));
#20006=CARTESIAN_POINT('Ctrl Pts',(1.80266937724758,-0.854055430773574,
34.0227740314037));
#20007=CARTESIAN_POINT('Ctrl Pts',(1.83249586674141,-0.79110015023325,34.0272123947924));
#20008=CARTESIAN_POINT('Ctrl Pts',(1.85904211283213,-0.726534959419857,
34.031650758181));
#20009=CARTESIAN_POINT('Ctrl Pts',(1.88214117995257,-0.660736060183446,
34.0360891215697));
#20010=CARTESIAN_POINT('Ctrl Pts',(1.90523353970721,-0.594956267228886,
34.0405261961735));
#20011=CARTESIAN_POINT('Ctrl Pts',(1.92488054539363,-0.527943938899148,
34.0449632707773));
#20012=CARTESIAN_POINT('Ctrl Pts',(1.94096406042321,-0.460093554231588,
34.0494003453812));
#20013=CARTESIAN_POINT('Ctrl Pts',(1.9570483763665,-0.392239790806103,34.0538376409388));
#20014=CARTESIAN_POINT('Ctrl Pts',(1.96956873870942,-0.323548365321683,
34.0582749364964));
#20015=CARTESIAN_POINT('Ctrl Pts',(1.97845780201861,-0.254425407795087,
34.0627122320541));
#20016=CARTESIAN_POINT('Ctrl Pts',(1.98735631033948,-0.185229004156309,
34.0671542424289));
#20017=CARTESIAN_POINT('Ctrl Pts',(1.99261575586071,-0.115600640050258,
34.0715962528037));
#20018=CARTESIAN_POINT('Ctrl Pts',(1.99422064170287,-0.0459520914235337,
34.0760382631785));
#20019=CARTESIAN_POINT('Ctrl Pts',(1.9958264667438,0.0237372163832464,34.080482873072));
#20020=CARTESIAN_POINT('Ctrl Pts',(1.99377348981726,0.0934462425034592,
34.0849274829655));
#20021=CARTESIAN_POINT('Ctrl Pts',(1.98809832646439,0.162765496372865,34.0893720928589));
#20022=CARTESIAN_POINT('Ctrl Pts',(1.9824132334389,0.232206036177869,34.0938244793605));
#20023=CARTESIAN_POINT('Ctrl Pts',(1.97309336851641,0.301254957072016,34.098276865862));
#20024=CARTESIAN_POINT('Ctrl Pts',(1.96022682995715,0.369510943838119,34.1027292523635));
#20025=CARTESIAN_POINT('Ctrl Pts',(1.95331174700821,0.406194921278941,34.10512217427));
#20026=CARTESIAN_POINT('Ctrl Pts',(1.94537307969884,0.442650080962574,34.1075150961765));
#20027=CARTESIAN_POINT('Ctrl Pts',(1.93643040766279,0.47881608032617,34.1099080180829));
#20028=CARTESIAN_POINT('Ctrl Pts',(1.91978115192599,0.546149084371742,34.114363103612));
#20029=CARTESIAN_POINT('Ctrl Pts',(1.89958287229591,0.612745779472168,34.1188181891411));
#20030=CARTESIAN_POINT('Ctrl Pts',(1.87591738645606,0.678204631134182,34.1232732746701));
#20031=CARTESIAN_POINT('Ctrl Pts',(1.8522874912097,0.743565039037421,34.127721660183));
#20032=CARTESIAN_POINT('Ctrl Pts',(1.82520090407882,0.807790543440501,34.1321700456959));
#20033=CARTESIAN_POINT('Ctrl Pts',(1.79478988370777,0.870492295106765,34.1366184312088));
#20034=CARTESIAN_POINT('Ctrl Pts',(1.76441478933691,0.933119974179799,34.14106156163));
#20035=CARTESIAN_POINT('Ctrl Pts',(1.7307232745168,0.994227037629293,34.1455046920513));
#20036=CARTESIAN_POINT('Ctrl Pts',(1.69389593896112,1.05344392848933,34.1499478224725));
#20037=CARTESIAN_POINT('Ctrl Pts',(1.65709189562652,1.11262336638427,34.1543881427427));
#20038=CARTESIAN_POINT('Ctrl Pts',(1.61715622387695,1.16991458873398,34.1588284630129));
#20039=CARTESIAN_POINT('Ctrl Pts',(1.57431503903815,1.22497335495851,34.1632687832831));
#20040=CARTESIAN_POINT('Ctrl Pts',(1.53148640979262,1.28001598494691,34.1677078022154));
#20041=CARTESIAN_POINT('Ctrl Pts',(1.48575425823248,1.33282707167784,34.1721468211478));
#20042=CARTESIAN_POINT('Ctrl Pts',(1.43738648438939,1.38309350985199,34.1765858400801));
#20043=CARTESIAN_POINT('Ctrl Pts',(1.389016470411,1.43336227609738,34.181025064604));
#20044=CARTESIAN_POINT('Ctrl Pts',(1.33801093279439,1.48108580885929,34.1854642891278));
#20045=CARTESIAN_POINT('Ctrl Pts',(1.28467506801115,1.52598739579675,34.1899035136516));
#20046=CARTESIAN_POINT('Ctrl Pts',(1.23128299244483,1.57093630461366,34.1943474166838));
#20047=CARTESIAN_POINT('Ctrl Pts',(1.17555606281593,1.61305701572653,34.198791319716));
#20048=CARTESIAN_POINT('Ctrl Pts',(1.11783229705301,1.65211334906694,34.2032352227481));
#20049=CARTESIAN_POINT('Ctrl Pts',(1.06007499560169,1.69119237290594,34.2076817075478));
#20050=CARTESIAN_POINT('Ctrl Pts',(1.0003189681262,1.72720322270235,34.2121281923476));
#20051=CARTESIAN_POINT('Ctrl Pts',(0.938928539316298,1.75995476094057,34.2165746771473));
#20052=CARTESIAN_POINT('Ctrl Pts',(0.877431399751455,1.79276322892237,34.2210288909654));
#20053=CARTESIAN_POINT('Ctrl Pts',(0.814294630900114,1.82230086868221,34.2254831047835));
#20054=CARTESIAN_POINT('Ctrl Pts',(0.749903571495696,1.84842424674586,34.2299373186015));
#20055=CARTESIAN_POINT('Ctrl Pts',(0.715561891006039,1.86235662666118,34.2323128842342));
#20056=CARTESIAN_POINT('Ctrl Pts',(0.680863721592592,1.87531869413497,34.2346884498669));
#20057=CARTESIAN_POINT('Ctrl Pts',(0.645869034668112,1.88729455903335,34.2370640154996));
#20058=CARTESIAN_POINT('Ctrl Pts',(0.580237742985919,1.90975486805078,34.2415193044206));
#20059=CARTESIAN_POINT('Ctrl Pts',(0.513304158713682,1.92883182304986,34.2459745933416));
#20060=CARTESIAN_POINT('Ctrl Pts',(0.445450283229097,1.9443769201652,34.2504298822626));
#20061=CARTESIAN_POINT('Ctrl Pts',(0.377698123176603,1.95989871461347,34.2548784925431));
#20062=CARTESIAN_POINT('Ctrl Pts',(0.309028883059356,1.97189905106972,34.2593271028237));
#20063=CARTESIAN_POINT('Ctrl Pts',(0.239841189049589,1.98027870930717,34.2637757131042));
#20064=CARTESIAN_POINT('Ctrl Pts',(0.170734756599664,1.98864852556176,34.2682190984526));
#20065=CARTESIAN_POINT('Ctrl Pts',(0.101111563046058,1.99340605122536,34.2726624838009));
#20066=CARTESIAN_POINT('Ctrl Pts',(0.0313801705448466,1.99450315803124,
34.2771058691493));
#20067=CARTESIAN_POINT('Ctrl Pts',(-0.0383074111212352,1.99559957554691,
34.2815464628077));
#20068=CARTESIAN_POINT('Ctrl Pts',(-0.108102568826947,1.99304012884137,
34.2859870564662));
#20069=CARTESIAN_POINT('Ctrl Pts',(-0.17759340119426,1.98682866557543,34.2904276501246));
#20070=CARTESIAN_POINT('Ctrl Pts',(-0.247064148813438,1.980618997592,34.2948669603303));
#20071=CARTESIAN_POINT('Ctrl Pts',(-0.31623025866382,1.97075945203409,34.2993062705359));
#20072=CARTESIAN_POINT('Ctrl Pts',(-0.384683401264078,1.95730586350011,
34.3037455807416));
#20073=CARTESIAN_POINT('Ctrl Pts',(-0.453139981230015,1.94385159939592,
34.3081851138666));
#20074=CARTESIAN_POINT('Ctrl Pts',(-0.520883043276488,1.92680303069498,
34.3126246469916));
#20075=CARTESIAN_POINT('Ctrl Pts',(-0.587514678796769,1.90626704968069,
34.3170641801166));
#20076=CARTESIAN_POINT('Ctrl Pts',(-0.654216890429641,1.88570931699099,
34.3215084155874));
#20077=CARTESIAN_POINT('Ctrl Pts',(-0.719804857395406,1.86165694359622,
34.3259526510582));
#20078=CARTESIAN_POINT('Ctrl Pts',(-0.783896991458646,1.83426635723444,
34.330396886529));
#20079=CARTESIAN_POINT('Ctrl Pts',(-0.848026560202037,1.80685977268731,
34.3348437177713));
#20080=CARTESIAN_POINT('Ctrl Pts',(-0.910658117742679,1.77611130996026,
34.3392905490136));
#20081=CARTESIAN_POINT('Ctrl Pts',(-0.971433715979074,1.74222389432561,
34.3437373802559));
#20082=CARTESIAN_POINT('Ctrl Pts',(-1.03231519222989,1.70827744295317,34.3481919583846));
#20083=CARTESIAN_POINT('Ctrl Pts',(-1.09133384074268,1.67118138300511,34.3526465365134));
#20084=CARTESIAN_POINT('Ctrl Pts',(-1.14816045382085,1.63118212802308,34.3571011146422));
#20085=CARTESIAN_POINT('Ctrl Pts',(-1.17843214780047,1.60987441424884,34.3594740807336));
#20086=CARTESIAN_POINT('Ctrl Pts',(-1.20808235829674,1.58774354703447,34.361847046825));
#20087=CARTESIAN_POINT('Ctrl Pts',(-1.23706541921401,1.56483120849658,34.3642200129164));
#20088=CARTESIAN_POINT('Ctrl Pts',(-1.29072717782349,1.52240931305536,34.3686135286305));
#20089=CARTESIAN_POINT('Ctrl Pts',(-1.34232494613137,1.47712826218427,34.3730070443447));
#20090=CARTESIAN_POINT('Ctrl Pts',(-1.39153172153462,1.4292190281629,34.3774005600589));
#20091=CARTESIAN_POINT('Ctrl Pts',(-1.44065389242058,1.38139216770868,34.3817865217061));
#20092=CARTESIAN_POINT('Ctrl Pts',(-1.48739287342646,1.3309464427752,34.3861724833533));
#20093=CARTESIAN_POINT('Ctrl Pts',(-1.53145375128017,1.2781537349591,34.3905584450005));
#20094=CARTESIAN_POINT('Ctrl Pts',(-1.57547233404685,1.22541170412177,34.3949401964585));
#20095=CARTESIAN_POINT('Ctrl Pts',(-1.61681758648526,1.17032753936153,34.3993219479166));
#20096=CARTESIAN_POINT('Ctrl Pts',(-1.65523165992728,1.11320964533837,34.4037036993747));
#20097=CARTESIAN_POINT('Ctrl Pts',(-1.69362274757341,1.05612592890003,34.4080828289279));
#20098=CARTESIAN_POINT('Ctrl Pts',(-1.72908585273544,0.997011313104283,
34.4124619584811));
#20099=CARTESIAN_POINT('Ctrl Pts',(-1.76140486097608,0.936205361141371,
34.4168410880343));
#20100=CARTESIAN_POINT('Ctrl Pts',(-1.79371621287798,0.875413814043905,
34.4212191801764));
#20101=CARTESIAN_POINT('Ctrl Pts',(-1.82288471026105,0.81293217122506,34.4255972723185));
#20102=CARTESIAN_POINT('Ctrl Pts',(-1.84873984602636,0.749125185943188,
34.4299753644606));
#20103=CARTESIAN_POINT('Ctrl Pts',(-1.87461425439687,0.685270638473024,
34.4343567200642));
#20104=CARTESIAN_POINT('Ctrl Pts',(-1.89717017614741,0.620089242522898,
34.4387380756679));
#20105=CARTESIAN_POINT('Ctrl Pts',(-1.91628549820525,0.553965208174902,
34.4431194312715));
#20106=CARTESIAN_POINT('Ctrl Pts',(-1.93540791808174,0.487816620936646,
34.4475024137412));
#20107=CARTESIAN_POINT('Ctrl Pts',(-1.95108707835117,0.420725189523249,
34.4518853962108));
#20108=CARTESIAN_POINT('Ctrl Pts',(-1.96325168347044,0.353086943755323,
34.4562683786804));
#20109=CARTESIAN_POINT('Ctrl Pts',(-1.97543605562596,0.285338788323872,
34.4606584833355));
#20110=CARTESIAN_POINT('Ctrl Pts',(-1.98409440487738,0.217042544924583,
34.4650485879906));
#20111=CARTESIAN_POINT('Ctrl Pts',(-1.98920727331645,0.1486000884419,34.4694386926456));
#20112=CARTESIAN_POINT('Ctrl Pts',(-1.9929365991361,0.0986781663031144,
34.4726408346205));
#20113=CARTESIAN_POINT('Ctrl Pts',(-1.99478074038682,0.0486785648499409,
34.4758429765955));
#20114=CARTESIAN_POINT('Ctrl Pts',(-1.99474961222923,-0.00124378911175243,
34.4790451185704));
#20115=CARTESIAN_POINT('',(-1.99475051924689,0.00023157645625902,32.0772022700356));
#20116=CARTESIAN_POINT('Ctrl Pts',(-1.99474972256505,-0.00105205830250181,
33.6805590561774));
#20117=CARTESIAN_POINT('Ctrl Pts',(-1.99477744459478,0.0515101533020236,
33.6773935162611));
#20118=CARTESIAN_POINT('Ctrl Pts',(-1.99272763643631,0.104049715830699,
33.6741765283108));
#20119=CARTESIAN_POINT('Ctrl Pts',(-1.98792330420288,0.165118763130328,
33.6703506018151));
#20120=CARTESIAN_POINT('Ctrl Pts',(-1.98718416512581,0.173788260227377,
33.6698054427645));
#20121=CARTESIAN_POINT('Ctrl Pts',(-1.9858624755907,0.188177693956954,33.6688971215239));
#20122=CARTESIAN_POINT('Ctrl Pts',(-1.98531186732526,0.1939005023272,33.6685349589675));
#20123=CARTESIAN_POINT('Ctrl Pts',(-1.9842751214132,0.2042083833691,33.6678809511091));
#20124=CARTESIAN_POINT('Ctrl Pts',(-1.98379781052901,0.208794319023396,
33.6675893845459));
#20125=CARTESIAN_POINT('Ctrl Pts',(-1.98279099217451,0.218152465343164,
33.6669931625318));
#20126=CARTESIAN_POINT('Ctrl Pts',(-1.98226014540201,0.222924498593705,
33.6666884667989));
#20127=CARTESIAN_POINT('Ctrl Pts',(-1.98107837191606,0.233209922411704,
33.66603029077));
#20128=CARTESIAN_POINT('Ctrl Pts',(-1.98042164846761,0.238722593897857,
33.665676630001));
#20129=CARTESIAN_POINT('Ctrl Pts',(-1.97858703115242,0.253593957082281,
33.6647201072701));
#20130=CARTESIAN_POINT('Ctrl Pts',(-1.97736576597867,0.262947061925106,
33.664115881357));
#20131=CARTESIAN_POINT('Ctrl Pts',(-1.97128706494602,0.307061585743987,
33.6612532805799));
#20132=CARTESIAN_POINT('Ctrl Pts',(-1.96557929425604,0.341697654986037,
33.6589682061771));
#20133=CARTESIAN_POINT('Ctrl Pts',(-1.95340753657661,0.405085004377851,
33.6547139254358));
#20134=CARTESIAN_POINT('Ctrl Pts',(-1.94721439616133,0.43387880220416,33.6527536005671));
#20135=CARTESIAN_POINT('Ctrl Pts',(-1.89984430521305,0.632606481346904,
33.6390309966897));
#20136=CARTESIAN_POINT('Ctrl Pts',(-1.83711577038384,0.796611095484098,
33.6266262800367));
#20137=CARTESIAN_POINT('Ctrl Pts',(-1.72340151515232,1.00647745140216,33.6102138885024));
#20138=CARTESIAN_POINT('Ctrl Pts',(-1.6902786233565,1.06116431148707,33.6058921517241));
#20139=CARTESIAN_POINT('Ctrl Pts',(-1.65071104683783,1.11992351436634,33.6012725129818));
#20140=CARTESIAN_POINT('Ctrl Pts',(-1.64680820314792,1.12565464671479,33.6008222054153));
#20141=CARTESIAN_POINT('Ctrl Pts',(-1.64093775524626,1.13417922668787,33.6001529598754));
#20142=CARTESIAN_POINT('Ctrl Pts',(-1.63899278084729,1.13698808243602,33.5999325326198));
#20143=CARTESIAN_POINT('Ctrl Pts',(-1.63564680361365,1.14179378447927,33.5995555745869));
#20144=CARTESIAN_POINT('Ctrl Pts',(-1.63424934863103,1.14379306659612,33.599398803704));
#20145=CARTESIAN_POINT('Ctrl Pts',(-1.63133409979684,1.14794754482382,33.5990731491221));
#20146=CARTESIAN_POINT('Ctrl Pts',(-1.62981570635026,1.15010228865044,33.5989043083394));
#20147=CARTESIAN_POINT('Ctrl Pts',(-1.62560067784433,1.15605870222888,33.5984377296933));
#20148=CARTESIAN_POINT('Ctrl Pts',(-1.62289496075444,1.159853971078,33.5981406103505));
#20149=CARTESIAN_POINT('Ctrl Pts',(-1.61217610584233,1.17477820385246,33.5969727702889));
#20150=CARTESIAN_POINT('Ctrl Pts',(-1.60406136404328,1.18583421681277,33.5961087897412));
#20151=CARTESIAN_POINT('Ctrl Pts',(-1.59382176705603,1.1994877966176,33.5950420722204));
#20152=CARTESIAN_POINT('Ctrl Pts',(-1.59180378211631,1.20216451409603,33.5948329596662));
#20153=CARTESIAN_POINT('Ctrl Pts',(-1.47626023653814,1.3546240059377,33.5829222915553));
#20154=CARTESIAN_POINT('Ctrl Pts',(-1.34212504646792,1.48764066846578,33.5724530691031));
#20155=CARTESIAN_POINT('Ctrl Pts',(-1.13828185602176,1.6394256350726,33.5575085596647));
#20156=CARTESIAN_POINT('Ctrl Pts',(-1.08330588349975,1.67626048705518,33.5535655745298));
#20157=CARTESIAN_POINT('Ctrl Pts',(-1.00592318294249,1.72270948953602,33.5480533851149));
#20158=CARTESIAN_POINT('Ctrl Pts',(-0.98501821094353,1.73474738341249,33.5465680673452));
#20159=CARTESIAN_POINT('Ctrl Pts',(-0.953627381916452,1.75207307845742,
33.5443404014604));
#20160=CARTESIAN_POINT('Ctrl Pts',(-0.9433043687139,1.7576524441856,33.5436082529417));
#20161=CARTESIAN_POINT('Ctrl Pts',(-0.926732803547868,1.7664209796327,33.5424333154536));
#20162=CARTESIAN_POINT('Ctrl Pts',(-0.920515510308838,1.76966888420559,
33.5419925899868));
#20163=CARTESIAN_POINT('Ctrl Pts',(-0.908656461074274,1.77578462969958,
33.5411520316219));
#20164=CARTESIAN_POINT('Ctrl Pts',(-0.903017924288794,1.778658551337,33.5407524177316));
#20165=CARTESIAN_POINT('Ctrl Pts',(-0.893087696208261,1.78366052709539,
33.5400486719155));
#20166=CARTESIAN_POINT('Ctrl Pts',(-0.888801815917077,1.78580005611039,
33.5397449449549));
#20167=CARTESIAN_POINT('Ctrl Pts',(-0.880410618285732,1.78995128597121,
33.53915028631));
#20168=CARTESIAN_POINT('Ctrl Pts',(-0.87630600708342,1.79196435352844,33.538859404702));
#20169=CARTESIAN_POINT('Ctrl Pts',(-0.86541758377538,1.79725812038888,33.5380877531208));
#20170=CARTESIAN_POINT('Ctrl Pts',(-0.858622090401702,1.80051449561074,
33.5376061412599));
#20171=CARTESIAN_POINT('Ctrl Pts',(-0.834466651921713,1.81192184558229,
33.5358940020932));
#20172=CARTESIAN_POINT('Ctrl Pts',(-0.817008239684935,1.81986067082694,
33.5346561912457));
#20173=CARTESIAN_POINT('Ctrl Pts',(-0.629741348865567,1.90177836237216,
33.5213709377588));
#20174=CARTESIAN_POINT('Ctrl Pts',(-0.450563670174192,1.951998153889,33.5084633464905));
#20175=CARTESIAN_POINT('Ctrl Pts',(-0.168979055491203,1.99004403649769,
33.4886738511223));
#20176=CARTESIAN_POINT('Ctrl Pts',(-0.0700036625092822,1.99597935272083,
33.4818366122368));
#20177=CARTESIAN_POINT('Ctrl Pts',(0.0386265313581515,1.99439915219946,
33.4747191374701));
#20178=CARTESIAN_POINT('Ctrl Pts',(0.0482383909166484,1.99418982392594,
33.4740927468451));
#20179=CARTESIAN_POINT('Ctrl Pts',(0.0617504847671068,1.99379780261482,
33.4732172883785));
#20180=CARTESIAN_POINT('Ctrl Pts',(0.0656520772926734,1.99367314408893,
33.472965099983));
#20181=CARTESIAN_POINT('Ctrl Pts',(0.0723185348898683,1.99344055535584,
33.4725352500913));
#20182=CARTESIAN_POINT('Ctrl Pts',(0.0750835756446354,1.99333832432936,
33.4723572710567));
#20183=CARTESIAN_POINT('Ctrl Pts',(0.0803838998658419,1.9931313126746,33.4720167059737));
#20184=CARTESIAN_POINT('Ctrl Pts',(0.0829191974956272,1.99302744782545,
33.4718540679405));
#20185=CARTESIAN_POINT('Ctrl Pts',(0.0889351760702825,1.99276948884734,
33.4714687580706));
#20186=CARTESIAN_POINT('Ctrl Pts',(0.0924156797124349,1.99261111203722,
33.4712463259399));
#20187=CARTESIAN_POINT('Ctrl Pts',(0.102843931452138,1.99210920304792,33.4705812864893));
#20188=CARTESIAN_POINT('Ctrl Pts',(0.109790405663895,1.99173844199745,33.4701401652594));
#20189=CARTESIAN_POINT('Ctrl Pts',(0.230485166904379,1.9846631286278,33.4625060940494));
#20190=CARTESIAN_POINT('Ctrl Pts',(0.343474136770502,1.96825936722014,33.4558228846101));
#20191=CARTESIAN_POINT('Ctrl Pts',(0.55484888403689,1.918801781447,33.4432020713972));
#20192=CARTESIAN_POINT('Ctrl Pts',(0.653263370067661,1.88756553938182,33.4372710009004));
#20193=CARTESIAN_POINT('Ctrl Pts',(0.799135034822772,1.82848503664878,33.4279402843683));
#20194=CARTESIAN_POINT('Ctrl Pts',(0.848592875706664,1.80606305648148,33.4246776668016));
#20195=CARTESIAN_POINT('Ctrl Pts',(0.915859543650917,1.77219392479813,33.4200601280315));
#20196=CARTESIAN_POINT('Ctrl Pts',(0.934495550001225,1.76243809172148,33.4187610803365));
#20197=CARTESIAN_POINT('Ctrl Pts',(0.962306313961244,1.74731422078209,33.4167906153672));
#20198=CARTESIAN_POINT('Ctrl Pts',(0.971598507394432,1.74216438994554,33.4161267934267));
#20199=CARTESIAN_POINT('Ctrl Pts',(0.988572405275087,1.73257924356251,33.4149039151516));
#20200=CARTESIAN_POINT('Ctrl Pts',(0.996266551343735,1.72816642435796,33.4143456683371));
#20201=CARTESIAN_POINT('Ctrl Pts',(1.00853843242336,1.72101894919219,33.4134488648567));
#20202=CARTESIAN_POINT('Ctrl Pts',(1.01313513746588,1.71831696304417,33.4131114926562));
#20203=CARTESIAN_POINT('Ctrl Pts',(1.01772692389036,1.71559303768039,33.4127730077603));
#20204=CARTESIAN_POINT('Ctrl Pts',(1.01773292994288,1.71558947474582,33.4127725650198));
#20205=CARTESIAN_POINT('Ctrl Pts',(1.01774496011206,1.7155823380752,33.4127716782022));
#20206=CARTESIAN_POINT('Ctrl Pts',(1.01775098428653,1.71557876430459,33.4127712341208));
#20207=CARTESIAN_POINT('Ctrl Pts',(1.0177630509291,1.71557160582496,33.4127703446043));
#20208=CARTESIAN_POINT('Ctrl Pts',(1.01776909334588,1.71556802114614,33.412769899173));
#20209=CARTESIAN_POINT('Ctrl Pts',(1.01778119646431,1.71556084085448,33.4127690069573));
#20210=CARTESIAN_POINT('Ctrl Pts',(1.01778725717637,1.71555724523522,33.4127685601722));
#20211=CARTESIAN_POINT('Ctrl Pts',(1.01779939689641,1.71555004305536,33.412767665248));
#20212=CARTESIAN_POINT('Ctrl Pts',(1.0178054759447,1.71554643647059,33.412767217106));
#20213=CARTESIAN_POINT('Ctrl Pts',(1.01781765245366,1.71553921228982,33.4127663194594));
#20214=CARTESIAN_POINT('Ctrl Pts',(1.01782374991602,1.71553559469256,33.4127658699547));
#20215=CARTESIAN_POINT('Ctrl Pts',(1.01783596328427,1.71552834846753,33.4127649695805));
#20216=CARTESIAN_POINT('Ctrl Pts',(1.01784207919452,1.71552471983692,33.4127645187105));
#20217=CARTESIAN_POINT('Ctrl Pts',(1.01785432967048,1.71551745141865,33.4127636155901));
#20218=CARTESIAN_POINT('Ctrl Pts',(1.0178604641518,1.71551381168079,33.4127631633459));
#20219=CARTESIAN_POINT('Ctrl Pts',(1.01787275173343,1.71550652106886,33.4127622574794));
#20220=CARTESIAN_POINT('Ctrl Pts',(1.0178789048366,1.71550287019282,33.412761803857));
#20221=CARTESIAN_POINT('Ctrl Pts',(1.0178912296432,1.71549555731484,33.4127608952356));
#20222=CARTESIAN_POINT('Ctrl Pts',(1.01789740139469,1.7154918952841,33.4127604402331));
#20223=CARTESIAN_POINT('Ctrl Pts',(1.01790976366184,1.71548455999863,33.4127595288393));
#20224=CARTESIAN_POINT('Ctrl Pts',(1.01791595415525,1.71548088675684,33.4127590724497));
#20225=CARTESIAN_POINT('Ctrl Pts',(1.01792835391224,1.71547352904487,33.4127581582812));
#20226=CARTESIAN_POINT('Ctrl Pts',(1.01793456316834,1.71546984457886,33.4127577005029));
#20227=CARTESIAN_POINT('Ctrl Pts',(1.01794700073147,1.71546246425104,33.4127567835364));
#20228=CARTESIAN_POINT('Ctrl Pts',(1.01795322891158,1.71545876846427,33.4127563243574));
#20229=CARTESIAN_POINT('Ctrl Pts',(1.01796570415503,1.71545136559359,33.412755404602));
#20230=CARTESIAN_POINT('Ctrl Pts',(1.01797195125887,1.71544765848538,33.4127549440224));
#20231=CARTESIAN_POINT('Ctrl Pts',(1.0179844644544,1.71544023290891,33.4127540214579));
#20232=CARTESIAN_POINT('Ctrl Pts',(1.01799073055532,1.71543651443489,33.4127535594723));
#20233=CARTESIAN_POINT('Ctrl Pts',(1.01800328182877,1.71542906607626,33.4127526340894));
#20234=CARTESIAN_POINT('Ctrl Pts',(1.01800956700072,1.7154253361917,33.4127521706921));
#20235=CARTESIAN_POINT('Ctrl Pts',(1.01802215646519,1.71541786498209,33.4127512424823));
#20236=CARTESIAN_POINT('Ctrl Pts',(1.01802846076987,1.71541412364953,33.4127507776689));
#20237=CARTESIAN_POINT('Ctrl Pts',(1.01804108854267,1.7154066295176,33.4127498466235));
#20238=CARTESIAN_POINT('Ctrl Pts',(1.01804741202071,1.71540287671206,33.4127493803908));
#20239=CARTESIAN_POINT('Ctrl Pts',(1.01806007831747,1.71539535952813,33.4127484464937));
#20240=CARTESIAN_POINT('Ctrl Pts',(1.01806642106507,1.71539159519165,33.4127479788347));
#20241=CARTESIAN_POINT('Ctrl Pts',(1.01807912596919,1.71538405490448,33.4127470420798));
#20242=CARTESIAN_POINT('Ctrl Pts',(1.01808548806063,1.71538027899212,33.4127465729888));
#20243=CARTESIAN_POINT('Ctrl Pts',(1.01809823173216,1.71537271550498,33.4127456333641));
#20244=CARTESIAN_POINT('Ctrl Pts',(1.0181046132738,1.71536892795272,33.4127451628333));
#20245=CARTESIAN_POINT('Ctrl Pts',(1.01811739569676,1.71536134127333,33.4127442203399));
#20246=CARTESIAN_POINT('Ctrl Pts',(1.01812379668236,1.71535754208401,33.4127437483697));
#20247=CARTESIAN_POINT('Ctrl Pts',(1.01813661813287,1.71534993204673,33.4127428029872));
#20248=CARTESIAN_POINT('Ctrl Pts',(1.01814303862253,1.71534612118378,33.4127423295731));
#20249=CARTESIAN_POINT('Ctrl Pts',(1.01815589935284,1.71533848763709,33.4127413812827));
#20250=CARTESIAN_POINT('Ctrl Pts',(1.01816233951452,1.71533466499993,33.4127409064122));
#20251=CARTESIAN_POINT('Ctrl Pts',(1.01817523930377,1.71532700807314,33.4127399552302));
#20252=CARTESIAN_POINT('Ctrl Pts',(1.01818169904741,1.71532317371432,33.41273947891));
#20253=CARTESIAN_POINT('Ctrl Pts',(1.01819463850265,1.7153154930453,33.4127385247914));
#20254=CARTESIAN_POINT('Ctrl Pts',(1.01820111804933,1.71531164683269,33.4127380470051));
#20255=CARTESIAN_POINT('Ctrl Pts',(1.01821409694964,1.71530394255075,33.4127370899661));
#20256=CARTESIAN_POINT('Ctrl Pts',(1.01822059631392,1.7153000844748,33.4127366107125));
#20257=CARTESIAN_POINT('Ctrl Pts',(1.01823361487003,1.71529235645303,33.4127356507375));
#20258=CARTESIAN_POINT('Ctrl Pts',(1.0182401340844,1.71528848649353,33.4127351700143));
#20259=CARTESIAN_POINT('Ctrl Pts',(1.01825319251392,1.71528073460091,33.4127342070871));
#20260=CARTESIAN_POINT('Ctrl Pts',(1.01825973165292,1.71527685271269,33.4127337248887));
#20261=CARTESIAN_POINT('Ctrl Pts',(1.02242343109338,1.71280508595897,33.4124266903121));
#20262=CARTESIAN_POINT('Ctrl Pts',(1.02657157532018,1.71032211439959,33.4121195893019));
#20263=CARTESIAN_POINT('Ctrl Pts',(1.03598583272414,1.7046403963131,33.4114198327033));
#20264=CARTESIAN_POINT('Ctrl Pts',(1.04124621408939,1.70143229268289,33.4110268362233));
#20265=CARTESIAN_POINT('Ctrl Pts',(1.05720194315426,1.69159980096969,33.4098286631592));
#20266=CARTESIAN_POINT('Ctrl Pts',(1.06784939839352,1.68489865735168,33.4090206649226));
#20267=CARTESIAN_POINT('Ctrl Pts',(1.2095077617466,1.59386163331758,33.3981553333141));
#20268=CARTESIAN_POINT('Ctrl Pts',(1.33023402222521,1.4945773635237,33.3875002542286));
#20269=CARTESIAN_POINT('Ctrl Pts',(1.50166665670833,1.31621567957269,33.3702572796715));
#20270=CARTESIAN_POINT('Ctrl Pts',(1.56054690280423,1.24584151482424,33.3638357873978));
#20271=CARTESIAN_POINT('Ctrl Pts',(1.63469016378132,1.1436831378983,33.3552210293849));
#20272=CARTESIAN_POINT('Ctrl Pts',(1.65426946535809,1.11517527151357,33.3528871168934));
#20273=CARTESIAN_POINT('Ctrl Pts',(1.68359869238016,1.06999758632369,33.3493123783605));
#20274=CARTESIAN_POINT('Ctrl Pts',(1.69386392221676,1.05367190005601,33.3480449229987));
#20275=CARTESIAN_POINT('Ctrl Pts',(1.70652986906523,1.03286452168446,33.3464624949052));
#20276=CARTESIAN_POINT('Ctrl Pts',(1.70915197081158,1.02851974031135,33.3461338600857));
#20277=CARTESIAN_POINT('Ctrl Pts',(1.71330806750506,1.02157336928759,33.345611353703));
#20278=CARTESIAN_POINT('Ctrl Pts',(1.7148527619035,1.01897825703279,33.3454167938415));
#20279=CARTESIAN_POINT('Ctrl Pts',(1.71777250601847,1.01404759524331,33.3450483703071));
#20280=CARTESIAN_POINT('Ctrl Pts',(1.71914867244162,1.01171278037747,33.3448744367653));
#20281=CARTESIAN_POINT('Ctrl Pts',(1.72229150276901,1.00635570092846,33.3444765500905));
#20282=CARTESIAN_POINT('Ctrl Pts',(1.72405497035828,1.0033315887291,33.3442528058552));
#20283=CARTESIAN_POINT('Ctrl Pts',(1.72959917392851,0.993766240675727,33.343547776046));
#20284=CARTESIAN_POINT('Ctrl Pts',(1.73335076937651,0.987208062286015,33.343068339897));
#20285=CARTESIAN_POINT('Ctrl Pts',(1.79755738574391,0.873473799068034,33.334818955248));
#20286=CARTESIAN_POINT('Ctrl Pts',(1.84801534220148,0.760932552141375,33.3276443188568));
#20287=CARTESIAN_POINT('Ctrl Pts',(1.92011267509742,0.549735737378889,33.3146891774949));
#20288=CARTESIAN_POINT('Ctrl Pts',(1.94526953604433,0.452733166265001,33.30891675559));
#20289=CARTESIAN_POINT('Ctrl Pts',(1.97199914774983,0.304616735853402,33.2999661453416));
#20290=CARTESIAN_POINT('Ctrl Pts',(1.97907073545238,0.25465749357308,33.296926055634));
#20291=CARTESIAN_POINT('Ctrl Pts',(1.98734265408806,0.174390708791092,33.2919718557718));
#20292=CARTESIAN_POINT('Ctrl Pts',(1.98975893930898,0.144229517552331,33.2900947644228));
#20293=CARTESIAN_POINT('Ctrl Pts',(1.99198379146869,0.105372088896581,33.2876521010948));
#20294=CARTESIAN_POINT('Ctrl Pts',(1.99242287859085,0.0967148987408133,
33.2871063456939));
#20295=CARTESIAN_POINT('Ctrl Pts',(1.99304068257595,0.0827331830997572,
33.2862223290833));
#20296=CARTESIAN_POINT('Ctrl Pts',(1.99325452290471,0.077410257784379,33.285885170752));
#20297=CARTESIAN_POINT('Ctrl Pts',(1.99362211027231,0.0672451766690467,
33.2852401199968));
#20298=CARTESIAN_POINT('Ctrl Pts',(1.9937795450106,0.0624031855658031,33.2849323454991));
#20299=CARTESIAN_POINT('Ctrl Pts',(1.99409953337463,0.0513186965914399,
33.284226577485));
#20300=CARTESIAN_POINT('Ctrl Pts',(1.99425041457987,0.045075937114839,33.283828221122));
#20301=CARTESIAN_POINT('Ctrl Pts',(1.99462511796472,0.0258318651389071,
33.2825975019978));
#20302=CARTESIAN_POINT('Ctrl Pts',(1.99475112352556,0.0128291992312109,
33.281762088333));
#20303=CARTESIAN_POINT('Ctrl Pts',(1.99473884836087,-0.128285093767944,
33.2726522640937));
#20304=CARTESIAN_POINT('Ctrl Pts',(1.98238635212579,-0.256072427776669,
33.2639855229705));
#20305=CARTESIAN_POINT('Ctrl Pts',(1.92826998706629,-0.533602193372845,
33.2443853480347));
#20306=CARTESIAN_POINT('Ctrl Pts',(1.88110331019069,-0.681477104812966,
33.2334114257033));
#20307=CARTESIAN_POINT('Ctrl Pts',(1.80985807849128,-0.838909342234719,
33.2219590437263));
#20308=CARTESIAN_POINT('Ctrl Pts',(1.80217145143339,-0.855297179481269,
33.2207705091546));
#20309=CARTESIAN_POINT('Ctrl Pts',(1.79209331013041,-0.876044392180787,
33.2192725155312));
#20310=CARTESIAN_POINT('Ctrl Pts',(1.78990742460605,-0.880501914769513,
33.2189510715677));
#20311=CARTESIAN_POINT('Ctrl Pts',(1.78637599383684,-0.887635817106282,
33.2184373227388));
#20312=CARTESIAN_POINT('Ctrl Pts',(1.78504103981864,-0.890317371290007,
33.2182443686315));
#20313=CARTESIAN_POINT('Ctrl Pts',(1.78248374249767,-0.895425402782863,
33.217877131617));
#20314=CARTESIAN_POINT('Ctrl Pts',(1.78126249717655,-0.897852360050421,
33.2177027865719));
#20315=CARTESIAN_POINT('Ctrl Pts',(1.77843519002581,-0.903442539628952,
33.217301513022));
#20316=CARTESIAN_POINT('Ctrl Pts',(1.77682564629589,-0.906603976758268,
33.2170748057109));
#20317=CARTESIAN_POINT('Ctrl Pts',(1.77248441590704,-0.915074975539426,
33.2164679121709));
#20318=CARTESIAN_POINT('Ctrl Pts',(1.76973728258311,-0.920376644805112,
33.2160886768607));
#20319=CARTESIAN_POINT('Ctrl Pts',(1.74953809025929,-0.958934065932428,
33.2133343820142));
#20320=CARTESIAN_POINT('Ctrl Pts',(1.73117238292781,-0.991705951294523,
33.2110138370989));
#20321=CARTESIAN_POINT('Ctrl Pts',(1.6683061961855,-1.09680959281878,33.2035745629473));
#20322=CARTESIAN_POINT('Ctrl Pts',(1.62010974658528,-1.16682633073641,33.1986211702758));
#20323=CARTESIAN_POINT('Ctrl Pts',(1.50528268958832,-1.31274686747913,33.1878389153347));
#20324=CARTESIAN_POINT('Ctrl Pts',(1.43706279314533,-1.38709398664308,33.1820304617162));
#20325=CARTESIAN_POINT('Ctrl Pts',(1.32607584282458,-1.49103399804107,33.1729940760045));
#20326=CARTESIAN_POINT('Ctrl Pts',(1.28729363047979,-1.52464226216208,33.1699040623753));
#20327=CARTESIAN_POINT('Ctrl Pts',(1.2233577251554,-1.57586852646034,33.1648756462386));
#20328=CARTESIAN_POINT('Ctrl Pts',(1.19901730040011,-1.59446639673979,33.1629757074807));
#20329=CARTESIAN_POINT('Ctrl Pts',(1.16722157163425,-1.61762083375273,33.1605073156984));
#20330=CARTESIAN_POINT('Ctrl Pts',(1.16015041861719,-1.62269971386889,33.159959203521));
#20331=CARTESIAN_POINT('Ctrl Pts',(1.14869231838148,-1.63081635704948,33.159072286093));
#20332=CARTESIAN_POINT('Ctrl Pts',(1.1443259805923,-1.63388312983753,33.1587345969956));
#20333=CARTESIAN_POINT('Ctrl Pts',(1.13597344148884,-1.63969977559077,33.1580891406862));
#20334=CARTESIAN_POINT('Ctrl Pts',(1.13198942221199,-1.64245272722261,33.1577814939705));
#20335=CARTESIAN_POINT('Ctrl Pts',(1.12285832893615,-1.64871329566615,33.1570768804563));
#20336=CARTESIAN_POINT('Ctrl Pts',(1.11770479147461,-1.65221135325588,33.1566795550742));
#20337=CARTESIAN_POINT('Ctrl Pts',(1.10181041759449,-1.6628915522836,33.1554551664207));
#20338=CARTESIAN_POINT('Ctrl Pts',(1.09101628313562,-1.66999340353429,33.1546250977026));
#20339=CARTESIAN_POINT('Ctrl Pts',(0.987393041226757,-1.7367374440694,33.1466687513528));
#20340=CARTESIAN_POINT('Ctrl Pts',(0.889851116694343,-1.78867534926581,
33.1392561987932));
#20341=CARTESIAN_POINT('Ctrl Pts',(0.630523295646565,-1.90027851872453,
33.1198022465785));
#20342=CARTESIAN_POINT('Ctrl Pts',(0.464387611604262,-1.94755311909873,
33.1075297798434));
#20343=CARTESIAN_POINT('Ctrl Pts',(0.275845110346863,-1.97567285512926,
33.0948884234622));
#20344=CARTESIAN_POINT('Ctrl Pts',(0.257404064695539,-1.97815999464585,
33.093666102252));
#20345=CARTESIAN_POINT('Ctrl Pts',(0.233953560237233,-1.98098925307041,
33.0921318847084));
#20346=CARTESIAN_POINT('Ctrl Pts',(0.228974690553975,-1.9815709125686,33.091807298754));
#20347=CARTESIAN_POINT('Ctrl Pts',(0.221006379669319,-1.9824713819332,33.0912897187511));
#20348=CARTESIAN_POINT('Ctrl Pts',(0.218018359687984,-1.98280220777863,
33.0910960585455));
#20349=CARTESIAN_POINT('Ctrl Pts',(0.212331477932492,-1.9834188340631,33.0907283042487));
#20350=CARTESIAN_POINT('Ctrl Pts',(0.209632814205677,-1.98370587818016,
33.0905541446227));
#20351=CARTESIAN_POINT('Ctrl Pts',(0.203425877133432,-1.98435327310112,
33.0901543813182));
#20352=CARTESIAN_POINT('Ctrl Pts',(0.199917230597112,-1.98470982799306,
33.089928993345));
#20353=CARTESIAN_POINT('Ctrl Pts',(0.188751728729845,-1.98581457692724,
33.0892135677565));
#20354=CARTESIAN_POINT('Ctrl Pts',(0.181091365915955,-1.98652779261813,
33.0887254578701));
#20355=CARTESIAN_POINT('Ctrl Pts',(0.0585593169347576,-1.99722142751281,
33.0809586496903));
#20356=CARTESIAN_POINT('Ctrl Pts',(-0.0569807634925121,-1.99726922053672,
33.0742017001674));
#20357=CARTESIAN_POINT('Ctrl Pts',(-0.274165003128792,-1.97848400321454,
33.0615312511667));
#20358=CARTESIAN_POINT('Ctrl Pts',(-0.375597679286987,-1.96175708664239,
33.0556237233778));
#20359=CARTESIAN_POINT('Ctrl Pts',(-0.546182901653154,-1.91990624639383,
33.0452056662972));
#20360=CARTESIAN_POINT('Ctrl Pts',(-0.616059833683593,-1.89863747394457,
33.0407949207249));
#20361=CARTESIAN_POINT('Ctrl Pts',(-0.700139848137715,-1.867914655736,33.0352290054685));
#20362=CARTESIAN_POINT('Ctrl Pts',(-0.715598954283094,-1.86204701302309,
33.0341947579378));
#20363=CARTESIAN_POINT('Ctrl Pts',(-0.737388080139877,-1.85346534119487,
33.0327208134592));
#20364=CARTESIAN_POINT('Ctrl Pts',(-0.743780022144838,-1.85090956788171,
33.0322864331287));
#20365=CARTESIAN_POINT('Ctrl Pts',(-0.754743667402192,-1.84645986834215,
33.0315378869697));
#20366=CARTESIAN_POINT('Ctrl Pts',(-0.759321817808162,-1.84458191066711,
33.0312242627497));
#20367=CARTESIAN_POINT('Ctrl Pts',(-0.768043386627528,-1.8409663510682,
33.030624769392));
#20368=CARTESIAN_POINT('Ctrl Pts',(-0.772188020319,-1.83923174457155,33.0303390034384));
#20369=CARTESIAN_POINT('Ctrl Pts',(-0.781844329174488,-1.83515200613445,
33.0296711503143));
#20370=CARTESIAN_POINT('Ctrl Pts',(-0.787351349343896,-1.83279603122462,
33.0292886957648));
#20371=CARTESIAN_POINT('Ctrl Pts',(-0.806243294211036,-1.82461295192599,
33.0279711950233));
#20372=CARTESIAN_POINT('Ctrl Pts',(-0.819574557554777,-1.81866385007215,
33.0270319917061));
#20373=CARTESIAN_POINT('Ctrl Pts',(-0.930510146111242,-1.76769117875129,
33.0191350537582));
#20374=CARTESIAN_POINT('Ctrl Pts',(-1.02437750385509,-1.71500003253068,
33.0119080925686));
#20375=CARTESIAN_POINT('Ctrl Pts',(-1.25623940790153,-1.55899796107296,
32.9926516570401));
#20376=CARTESIAN_POINT('Ctrl Pts',(-1.38592539259276,-1.4449303859441,32.9803804325206));
#20377=CARTESIAN_POINT('Ctrl Pts',(-1.5116644111489,-1.30163192733901,32.967737579238));
#20378=CARTESIAN_POINT('Ctrl Pts',(-1.52376124321964,-1.28744968900497,
32.966513089845));
#20379=CARTESIAN_POINT('Ctrl Pts',(-1.53885912343535,-1.26923808528586,
32.9649765561209));
#20380=CARTESIAN_POINT('Ctrl Pts',(-1.54204568383865,-1.26536470205288,
32.9646517759629));
#20381=CARTESIAN_POINT('Ctrl Pts',(-1.54711919047461,-1.25915003644248,
32.964133961802));
#20382=CARTESIAN_POINT('Ctrl Pts',(-1.54901548484136,-1.2568164670404,32.9639402605663));
#20383=CARTESIAN_POINT('Ctrl Pts',(-1.55261313179297,-1.25236871154936,
32.9635724785503));
#20384=CARTESIAN_POINT('Ctrl Pts',(-1.55431542565144,-1.25025536765374,
32.9633983320262));
#20385=CARTESIAN_POINT('Ctrl Pts',(-1.55821928052618,-1.24538855958788,
32.9629986664412));
#20386=CARTESIAN_POINT('Ctrl Pts',(-1.56041785696802,-1.24263273040667,
32.9627733627421));
#20387=CARTESIAN_POINT('Ctrl Pts',(-1.56738663284991,-1.23384998419723,
32.9620584693532));
#20388=CARTESIAN_POINT('Ctrl Pts',(-1.57212938151753,-1.22780122687483,
32.9615708033596));
#20389=CARTESIAN_POINT('Ctrl Pts',(-1.64775108555624,-1.13019898179613,
32.9537740741147));
#20390=CARTESIAN_POINT('Ctrl Pts',(-1.71057358246486,-1.03265677191458,
32.9469911646702));
#20391=CARTESIAN_POINT('Ctrl Pts',(-1.8123791974174,-0.839532200720969,
32.9343032637359));
#20392=CARTESIAN_POINT('Ctrl Pts',(-1.85311395055486,-0.745319007747131,
32.928404114423));
#20393=CARTESIAN_POINT('Ctrl Pts',(-1.90382017196381,-0.597795197695983,
32.9191500416256));
#20394=CARTESIAN_POINT('Ctrl Pts',(-1.91916796895547,-0.546519878407456,
32.9159324753358));
#20395=CARTESIAN_POINT('Ctrl Pts',(-1.94026606718953,-0.46410359594143,
32.9107149965564));
#20396=CARTESIAN_POINT('Ctrl Pts',(-1.94736887885266,-0.433334552911715,
32.9087573845429));
#20397=CARTESIAN_POINT('Ctrl Pts',(-1.95551325182578,-0.393792977147572,
32.9062241641222));
#20398=CARTESIAN_POINT('Ctrl Pts',(-1.95723127557921,-0.38516323398768,
32.9056702534992));
#20399=CARTESIAN_POINT('Ctrl Pts',(-1.95990318285128,-0.371262397022951,
32.9047762170149));
#20400=CARTESIAN_POINT('Ctrl Pts',(-1.96089304139973,-0.365998268945315,
32.9044372404049));
#20401=CARTESIAN_POINT('Ctrl Pts',(-1.96273654638875,-0.355972212920441,
32.9037908144142));
#20402=CARTESIAN_POINT('Ctrl Pts',(-1.96359409644646,-0.351211034315027,
32.9034834918385));
#20403=CARTESIAN_POINT('Ctrl Pts',(-1.96550931689918,-0.340351287357326,
32.9027817082168));
#20404=CARTESIAN_POINT('Ctrl Pts',(-1.96655593494064,-0.334250844345427,
32.9023868988679));
#20405=CARTESIAN_POINT('Ctrl Pts',(-1.96966706831472,-0.315596369129538,
32.9011777783363));
#20406=CARTESIAN_POINT('Ctrl Pts',(-1.97163985306709,-0.303027565644676,
32.9003605694334));
#20407=CARTESIAN_POINT('Ctrl Pts',(-1.98772906237007,-0.193704395418772,
32.893229323918));
#20408=CARTESIAN_POINT('Ctrl Pts',(-1.99483182175871,-0.0960674129391705,
32.8866928485967));
#20409=CARTESIAN_POINT('Ctrl Pts',(-1.99458667018612,0.194289775018152,
32.8667909497128));
#20410=CARTESIAN_POINT('Ctrl Pts',(-1.96653159115058,0.385843755610208,
32.8529671470688));
#20411=CARTESIAN_POINT('Ctrl Pts',(-1.90798583281888,0.582035260828337,
32.8394982905035));
#20412=CARTESIAN_POINT('Ctrl Pts',(-1.90440764546011,0.593638375404131,
32.8387048483445));
#20413=CARTESIAN_POINT('Ctrl Pts',(-1.89938014515719,0.609427792754021,
32.837630105199));
#20414=CARTESIAN_POINT('Ctrl Pts',(-1.89802260094675,0.613642711691862,
32.8373436924451));
#20415=CARTESIAN_POINT('Ctrl Pts',(-1.89584893659287,0.62031530513678,32.8368910845672));
#20416=CARTESIAN_POINT('Ctrl Pts',(-1.89504205704351,0.622775939156343,
32.8367243523832));
#20417=CARTESIAN_POINT('Ctrl Pts',(-1.89337435154761,0.627828468777678,
32.8363823632579));
#20418=CARTESIAN_POINT('Ctrl Pts',(-1.89251299590091,0.630420162850252,
32.8362071418891));
#20419=CARTESIAN_POINT('Ctrl Pts',(-1.89047158115592,0.636520594285752,
32.8357951599984));
#20420=CARTESIAN_POINT('Ctrl Pts',(-1.88928706551676,0.640027851517573,
32.8355586626359));
#20421=CARTESIAN_POINT('Ctrl Pts',(-1.88537086325206,0.651517808867437,
32.8347850007987));
#20422=CARTESIAN_POINT('Ctrl Pts',(-1.88259824742113,0.659486612548083,
32.8342502006518));
#20423=CARTESIAN_POINT('Ctrl Pts',(-1.84700088268742,0.759743212325898,
32.8275413083106));
#20424=CARTESIAN_POINT('Ctrl Pts',(-1.8074671327058,0.849523501464951,32.8217394379467));
#20425=CARTESIAN_POINT('Ctrl Pts',(-1.72508397598899,1.00455551351148,32.8114912688448));
#20426=CARTESIAN_POINT('Ctrl Pts',(-1.68471245572965,1.07088310121653,32.8070230681841));
#20427=CARTESIAN_POINT('Ctrl Pts',(-1.57257865582955,1.23301048307141,32.7955259223322));
#20428=CARTESIAN_POINT('Ctrl Pts',(-1.49588715298001,1.32500338217681,32.7884298300651));
#20429=CARTESIAN_POINT('Ctrl Pts',(-1.40224362705978,1.41877037674333,32.78015860791));
#20430=CARTESIAN_POINT('Ctrl Pts',(-1.39296752325565,1.42787885969652,32.779343339137));
#20431=CARTESIAN_POINT('Ctrl Pts',(-1.37910533809226,1.44122691412289,32.7781306050252));
#20432=CARTESIAN_POINT('Ctrl Pts',(-1.37458718618475,1.44553679222747,32.7777361995507));
#20433=CARTESIAN_POINT('Ctrl Pts',(-1.36652776763516,1.45315274242654,32.7770341533305));
#20434=CARTESIAN_POINT('Ctrl Pts',(-1.36299453657825,1.45646727567738,32.7767268803675));
#20435=CARTESIAN_POINT('Ctrl Pts',(-1.35555047957879,1.46339975529426,32.7760805270823));
#20436=CARTESIAN_POINT('Ctrl Pts',(-1.35163716863083,1.4670149658232,32.7757413334263));
#20437=CARTESIAN_POINT('Ctrl Pts',(-1.34131761441829,1.47647207470504,32.7748483833606));
#20438=CARTESIAN_POINT('Ctrl Pts',(-1.33488774007418,1.48228790981908,32.7742935299177));
#20439=CARTESIAN_POINT('Ctrl Pts',(-1.30583916977515,1.50822010881898,32.771793432694));
#20440=CARTESIAN_POINT('Ctrl Pts',(-1.28280327728808,1.52786105985651,32.7698285247641));
#20441=CARTESIAN_POINT('Ctrl Pts',(-1.22018509572006,1.57883619908952,32.7645303250658));
#20442=CARTESIAN_POINT('Ctrl Pts',(-1.179847362089,1.60920318525719,32.7611608117992));
#20443=CARTESIAN_POINT('Ctrl Pts',(-1.05616984104671,1.69515831966415,32.7509595429295));
#20444=CARTESIAN_POINT('Ctrl Pts',(-0.969754995040446,1.74603218611233,
32.7439905885029));
#20445=CARTESIAN_POINT('Ctrl Pts',(-0.7695630574671,1.84442785149107,32.728426890033));
#20446=CARTESIAN_POINT('Ctrl Pts',(-0.654440341313981,1.88834760546612,
32.7198526623489));
#20447=CARTESIAN_POINT('Ctrl Pts',(-0.528717321011424,1.92341951470695,
32.7113311858702));
#20448=CARTESIAN_POINT('Ctrl Pts',(-0.521428900464774,1.925408149272,32.7108401491055));
#20449=CARTESIAN_POINT('Ctrl Pts',(-0.510746862472833,1.92825762266546,
32.7101249951532));
#20450=CARTESIAN_POINT('Ctrl Pts',(-0.507362106133707,1.92915098180841,
32.7098990503031));
#20451=CARTESIAN_POINT('Ctrl Pts',(-0.501352670570711,1.9307201784862,32.7094990936864));
#20452=CARTESIAN_POINT('Ctrl Pts',(-0.498728947774156,1.93139958188479,
32.709324876637));
#20453=CARTESIAN_POINT('Ctrl Pts',(-0.493178535587645,1.93282477630955,
32.7089571862852));
#20454=CARTESIAN_POINT('Ctrl Pts',(-0.490251542820833,1.93356926665156,
32.7087637888908));
#20455=CARTESIAN_POINT('Ctrl Pts',(-0.48240154988334,1.93554696754502,32.7082464299893));
#20456=CARTESIAN_POINT('Ctrl Pts',(-0.4774754742771,1.93676805315669,32.7079231630801));
#20457=CARTESIAN_POINT('Ctrl Pts',(-0.453806412464664,1.94253939553305,
32.706376339927));
#20458=CARTESIAN_POINT('Ctrl Pts',(-0.43500196949418,1.94683664355593,32.7051667452116));
#20459=CARTESIAN_POINT('Ctrl Pts',(-0.382311365505976,1.95807605560406,
32.7018236448342));
#20460=CARTESIAN_POINT('Ctrl Pts',(-0.348301354570823,1.96441092437159,
32.6997187896802));
#20461=CARTESIAN_POINT('Ctrl Pts',(-0.22353765502545,1.98430752801679,32.6921337820842));
#20462=CARTESIAN_POINT('Ctrl Pts',(-0.132038332065827,1.99248929803095,
32.6868291011406));
#20463=CARTESIAN_POINT('Ctrl Pts',(0.115341341372458,1.99748759438773,32.6724787583385));
#20464=CARTESIAN_POINT('Ctrl Pts',(0.27078595941242,1.98240409883719,32.6634088465011));
#20465=CARTESIAN_POINT('Ctrl Pts',(0.435177502552042,1.94674247501077,32.6529045297855));
#20466=CARTESIAN_POINT('Ctrl Pts',(0.447442099548372,1.94396020503084,32.6521155942448));
#20467=CARTESIAN_POINT('Ctrl Pts',(0.465674137452995,1.93964252200997,32.650934642161));
#20468=CARTESIAN_POINT('Ctrl Pts',(0.471662262436206,1.93819509448655,32.6505454548668));
#20469=CARTESIAN_POINT('Ctrl Pts',(0.482337302224436,1.93556236295809,32.649849260063));
#20470=CARTESIAN_POINT('Ctrl Pts',(0.487026814217527,1.93438771076944,32.6495425982607));
#20471=CARTESIAN_POINT('Ctrl Pts',(0.496918656268179,1.93187170249911,32.6488939746429));
#20472=CARTESIAN_POINT('Ctrl Pts',(0.50211992237897,1.93052635529357,32.6485518858979));
#20473=CARTESIAN_POINT('Ctrl Pts',(0.515895153053796,1.92690385119931,32.6476431092774));
#20474=CARTESIAN_POINT('Ctrl Pts',(0.52445939413496,1.92459050200217,32.6470752527393));
#20475=CARTESIAN_POINT('Ctrl Pts',(0.564159881649405,1.91358204912988,32.6444293660656));
#20476=CARTESIAN_POINT('Ctrl Pts',(0.595095737681122,1.90418840715719,32.6423287491064));
#20477=CARTESIAN_POINT('Ctrl Pts',(0.678283490822216,1.87670339781152,32.6365701791737));
#20478=CARTESIAN_POINT('Ctrl Pts',(0.730030544361641,1.85718566867715,32.6328677753725));
#20479=CARTESIAN_POINT('Ctrl Pts',(0.876530592845854,1.79486012382992,32.6220428058596));
#20480=CARTESIAN_POINT('Ctrl Pts',(0.968832036150822,1.74676558141627,32.6147854299863));
#20481=CARTESIAN_POINT('Ctrl Pts',(1.11743098731727,1.65392260325258,32.6025666605976));
#20482=CARTESIAN_POINT('Ctrl Pts',(1.17583772599546,1.61292245347771,32.5976111544589));
#20483=CARTESIAN_POINT('Ctrl Pts',(1.23891312196393,1.56339398567318,32.5921716413475));
#20484=CARTESIAN_POINT('Ctrl Pts',(1.24586338088172,1.55786100768995,32.5915710314367));
#20485=CARTESIAN_POINT('Ctrl Pts',(1.2788294097961,1.53125561253455,32.5887172118988));
#20486=CARTESIAN_POINT('Ctrl Pts',(1.30435075208309,1.50957538813166,32.5864927027896));
#20487=CARTESIAN_POINT('Ctrl Pts',(1.33361554271825,1.4834184849008,32.5839356860324));
#20488=CARTESIAN_POINT('Ctrl Pts',(1.33789849084449,1.47955684152574,32.5835613035209));
#20489=CARTESIAN_POINT('Ctrl Pts',(1.3447446610922,1.47333007891937,32.5829626941665));
#20490=CARTESIAN_POINT('Ctrl Pts',(1.34731849238037,1.47097675220543,32.5827376069981));
#20491=CARTESIAN_POINT('Ctrl Pts',(1.35188025158438,1.46678378901041,32.5823386234782));
#20492=CARTESIAN_POINT('Ctrl Pts',(1.35387061739581,1.46494684204821,32.5821645253628));
#20493=CARTESIAN_POINT('Ctrl Pts',(1.35807784778132,1.46104800995269,32.5817964907846));
#20494=CARTESIAN_POINT('Ctrl Pts',(1.36029375531232,1.45898513617468,32.5816026325279));
#20495=CARTESIAN_POINT('Ctrl Pts',(1.3662355842654,1.45342835404187,32.5810827361116));
#20496=CARTESIAN_POINT('Ctrl Pts',(1.36995282803574,1.44992513682281,32.5807574044685));
#20497=CARTESIAN_POINT('Ctrl Pts',(1.38790776916931,1.43287328833316,32.5791853558575));
#20498=CARTESIAN_POINT('Ctrl Pts',(1.40195876406899,1.41912844051604,32.5779531568966));
#20499=CARTESIAN_POINT('Ctrl Pts',(1.44082602122802,1.37996722900344,32.5745310831829));
#20500=CARTESIAN_POINT('Ctrl Pts',(1.4651708705644,1.35409150782168,32.5723715256103));
#20501=CARTESIAN_POINT('Ctrl Pts',(1.55245743144667,1.25620393370509,32.5645060913675));
#20502=CARTESIAN_POINT('Ctrl Pts',(1.61089109904218,1.18034092413618,32.5589883840596));
#20503=CARTESIAN_POINT('Ctrl Pts',(1.67373258218342,1.08534791939415,32.5523810193259));
#20504=CARTESIAN_POINT('Ctrl Pts',(1.68359579711485,1.06998413503928,32.5513213420575));
#20505=CARTESIAN_POINT('Ctrl Pts',(1.72135376153569,1.00935414501893,32.5471675815331));
#20506=CARTESIAN_POINT('Ctrl Pts',(1.74764413641418,0.963116904149641,32.5440594635375));
#20507=CARTESIAN_POINT('Ctrl Pts',(1.78387497986418,0.893017527110549,32.5393790417136));
#20508=CARTESIAN_POINT('Ctrl Pts',(1.79525056135997,0.869922755341378,32.5378420817085));
#20509=CARTESIAN_POINT('Ctrl Pts',(1.82971069945764,0.796405190612958,32.5329545304335));
#20510=CARTESIAN_POINT('Ctrl Pts',(1.85113988549463,0.745240043788715,32.5295595614446));
#20511=CARTESIAN_POINT('Ctrl Pts',(1.8738882410722,0.683864501366626,32.5254650148722));
#20512=CARTESIAN_POINT('Ctrl Pts',(1.87729690813832,0.674450968649196,32.5248364416027));
#20513=CARTESIAN_POINT('Ctrl Pts',(1.88271206133806,0.659137080657604,32.5238127913894));
#20514=CARTESIAN_POINT('Ctrl Pts',(1.88476204197238,0.653252202992117,32.5234191598557));
#20515=CARTESIAN_POINT('Ctrl Pts',(1.88835609893276,0.642776991517115,32.5227179862672));
#20516=CARTESIAN_POINT('Ctrl Pts',(1.88991110405571,0.638190438105606,32.5224108087179));
#20517=CARTESIAN_POINT('Ctrl Pts',(1.89314364395616,0.628540498092129,32.5217641411323));
#20518=CARTESIAN_POINT('Ctrl Pts',(1.89481760043134,0.623475961507653,32.5214245358033));
#20519=CARTESIAN_POINT('Ctrl Pts',(1.89916790981712,0.610134803183753,32.5205293334488));
#20520=CARTESIAN_POINT('Ctrl Pts',(1.9018104495278,0.601847354257184,32.5199726293005));
#20521=CARTESIAN_POINT('Ctrl Pts',(1.91349034862977,0.564372083747713,32.5174522962384));
#20522=CARTESIAN_POINT('Ctrl Pts',(1.92191014147969,0.534997569171342,32.5154686104084));
#20523=CARTESIAN_POINT('Ctrl Pts',(1.94260750810645,0.455980269522685,32.5101074872791));
#20524=CARTESIAN_POINT('Ctrl Pts',(1.9536558206389,0.40604202030779,32.5066927600023));
#20525=CARTESIAN_POINT('Ctrl Pts',(1.98072617445345,0.256682179002209,32.4964060180972));
#20526=CARTESIAN_POINT('Ctrl Pts',(1.99115348333106,0.15641743303547,32.4893970135368));
#20527=CARTESIAN_POINT('Ctrl Pts',(1.99736456050232,-0.0655156899101971,
32.4739066187066));
#20528=CARTESIAN_POINT('Ctrl Pts',(1.98968098453288,-0.18690740954904,32.46544801048));
#20529=CARTESIAN_POINT('Ctrl Pts',(1.96983898546714,-0.314355673926472,
32.457026571927));
#20530=CARTESIAN_POINT('Ctrl Pts',(1.96862913945504,-0.321845357539484,
32.4565334404044));
#20531=CARTESIAN_POINT('Ctrl Pts',(1.96679763103281,-0.332786624761421,
32.4558158170144));
#20532=CARTESIAN_POINT('Ctrl Pts',(1.96620956877452,-0.336243648531386,
32.4555894797688));
#20533=CARTESIAN_POINT('Ctrl Pts',(1.9651507038387,-0.342370593862699,32.4551890773148));
#20534=CARTESIAN_POINT('Ctrl Pts',(1.96468357112867,-0.345041125126671,
32.4550148052127));
#20535=CARTESIAN_POINT('Ctrl Pts',(1.96368510715721,-0.350681428011536,
32.4546472685231));
#20536=CARTESIAN_POINT('Ctrl Pts',(1.96315248420269,-0.353650941025623,
32.4544540788045));
#20537=CARTESIAN_POINT('Ctrl Pts',(1.96170843947949,-0.36159807527564,32.4539378628263));
#20538=CARTESIAN_POINT('Ctrl Pts',(1.96078480258814,-0.366573497211493,
32.4536155258246));
#20539=CARTESIAN_POINT('Ctrl Pts',(1.95628006668931,-0.390335253572446,
32.4520799206508));
#20540=CARTESIAN_POINT('Ctrl Pts',(1.9524477086605,-0.409073733944282,32.4508803702721));
#20541=CARTESIAN_POINT('Ctrl Pts',(1.9410174927103,-0.461136287084059,32.4475721556635));
#20542=CARTESIAN_POINT('Ctrl Pts',(1.93283157793759,-0.494325761173943,
32.4454914222752));
#20543=CARTESIAN_POINT('Ctrl Pts',(1.89987849515198,-0.614553661226869,
32.4380035581232));
#20544=CARTESIAN_POINT('Ctrl Pts',(1.87004930999941,-0.700094498784596,
32.4327682761755));
#20545=CARTESIAN_POINT('Ctrl Pts',(1.77261486071114,-0.928283444794056,
32.4183783679804));
#20546=CARTESIAN_POINT('Ctrl Pts',(1.69376389168123,-1.06537698320112,32.4092040329626));
#20547=CARTESIAN_POINT('Ctrl Pts',(1.59212644424844,-1.20179772962198,32.3985801178017));
#20548=CARTESIAN_POINT('Ctrl Pts',(1.58455013849633,-1.211769468417,32.3977944612093));
#20549=CARTESIAN_POINT('Ctrl Pts',(1.5731139943908,-1.22653077697972,32.396617472141));
#20550=CARTESIAN_POINT('Ctrl Pts',(1.56932498464801,-1.23137503523889,32.3962289408024));
#20551=CARTESIAN_POINT('Ctrl Pts',(1.56251839258574,-1.23999483679082,32.3955334762726));
#20552=CARTESIAN_POINT('Ctrl Pts',(1.55950936336184,-1.24377709713176,32.3952268860175));
#20553=CARTESIAN_POINT('Ctrl Pts',(1.55312289836002,-1.25174508281412,32.3945779517426));
#20554=CARTESIAN_POINT('Ctrl Pts',(1.54974222519764,-1.255928152509,32.3942354790177));
#20555=CARTESIAN_POINT('Ctrl Pts',(1.54072384522464,-1.26699517270886,32.3933246037741));
#20556=CARTESIAN_POINT('Ctrl Pts',(1.53505697500883,-1.27385509934689,32.392755022962));
#20557=CARTESIAN_POINT('Ctrl Pts',(1.50840775381711,-1.30567877213289,32.390089146776));
#20558=CARTESIAN_POINT('Ctrl Pts',(1.48686218613045,-1.33016226002758,32.3879698469219));
#20559=CARTESIAN_POINT('Ctrl Pts',(1.42673759741959,-1.39519864078846,32.3821468587206));
#20560=CARTESIAN_POINT('Ctrl Pts',(1.38703875512352,-1.43467137173626,32.3783974910547));
#20561=CARTESIAN_POINT('Ctrl Pts',(1.26863394464928,-1.54288886120904,32.3674851580711));
#20562=CARTESIAN_POINT('Ctrl Pts',(1.18612097049716,-1.60718759128474,32.3601878530912));
#20563=CARTESIAN_POINT('Ctrl Pts',(1.00713807874719,-1.7253424130091,32.3452343891684));
#20564=CARTESIAN_POINT('Ctrl Pts',(0.91044412816499,-1.77826637002954,32.3376063418241));
#20565=CARTESIAN_POINT('Ctrl Pts',(0.80347504740806,-1.8257886886864,32.3299616370584));
#20566=CARTESIAN_POINT('Ctrl Pts',(0.79706782121218,-1.82859491944787,32.3295066736343));
#20567=CARTESIAN_POINT('Ctrl Pts',(0.787438329915628,-1.8327522049802,32.3288274446735));
#20568=CARTESIAN_POINT('Ctrl Pts',(0.784227144523292,-1.83412855452577,
32.3286016931392));
#20569=CARTESIAN_POINT('Ctrl Pts',(0.77867523675752,-1.83649091723438,32.3282127060926));
#20570=CARTESIAN_POINT('Ctrl Pts',(0.776336230200448,-1.83748090365047,
32.3280492305237));
#20571=CARTESIAN_POINT('Ctrl Pts',(0.771501824193918,-1.8395161910968,32.3277121918679));
#20572=CARTESIAN_POINT('Ctrl Pts',(0.769006186141714,-1.84056088402972,
32.3275386681908));
#20573=CARTESIAN_POINT('Ctrl Pts',(0.763025081623626,-1.84305033109771,
32.3271238903255));
#20574=CARTESIAN_POINT('Ctrl Pts',(0.759537602938234,-1.84449028960265,
32.3268829272453));
#20575=CARTESIAN_POINT('Ctrl Pts',(0.75209367916114,-1.84753914756337,32.3263704435451));
#20576=CARTESIAN_POINT('Ctrl Pts',(0.748136101459601,-1.84914525619373,
32.3260990881553));
#20577=CARTESIAN_POINT('Ctrl Pts',(0.737253603402887,-1.85352105772802,
32.3253558757013));
#20578=CARTESIAN_POINT('Ctrl Pts',(0.73031817850206,-1.85626467653479,32.3248855050298));
#20579=CARTESIAN_POINT('Ctrl Pts',(0.669533444691139,-1.87991740342202,
32.3207902417237));
#20580=CARTESIAN_POINT('Ctrl Pts',(0.614809294862489,-1.89851925552571,
32.3172895199227));
#20581=CARTESIAN_POINT('Ctrl Pts',(0.457864477697418,-1.94436772459396,
32.3075665543522));
#20582=CARTESIAN_POINT('Ctrl Pts',(0.354178327847693,-1.96590073236273,
32.3015058179901));
#20583=CARTESIAN_POINT('Ctrl Pts',(0.122283269115748,-1.99510794679716,
32.2879034992953));
#20584=CARTESIAN_POINT('Ctrl Pts',(-0.0059277955016167,-1.99884135601865,
32.2803384516671));
#20585=CARTESIAN_POINT('Ctrl Pts',(-0.146593543900511,-1.98939875770172,
32.2715392050502));
#20586=CARTESIAN_POINT('Ctrl Pts',(-0.159575257583097,-1.9883995596025,
32.2707227133513));
#20587=CARTESIAN_POINT('Ctrl Pts',(-0.178770558302684,-1.98673291787286,
32.269508505695));
#20588=CARTESIAN_POINT('Ctrl Pts',(-0.184992465790764,-1.98616323237375,
32.2691138605299));
#20589=CARTESIAN_POINT('Ctrl Pts',(-0.1960343002,-1.98509989430986,32.2684115443737));
#20590=CARTESIAN_POINT('Ctrl Pts',(-0.20085531983028,-1.98461789195329,
32.2681042421835));
#20591=CARTESIAN_POINT('Ctrl Pts',(-0.210971802636704,-1.98356921329467,
32.267457986733));
#20592=CARTESIAN_POINT('Ctrl Pts',(-0.216266841089597,-1.98299888501643,
32.2671189207444));
#20593=CARTESIAN_POINT('Ctrl Pts',(-0.230166976232471,-1.98144536634449,
32.2662266669185));
#20594=CARTESIAN_POINT('Ctrl Pts',(-0.238767990847383,-1.98042733251649,
32.2656723851528));
#20595=CARTESIAN_POINT('Ctrl Pts',(-0.277311643169661,-1.97561048932814,
32.2631784968194));
#20596=CARTESIAN_POINT('Ctrl Pts',(-0.30717102911427,-1.97118856169952,
32.2612193457107));
#20597=CARTESIAN_POINT('Ctrl Pts',(-0.386471177699078,-1.95759936866033,
32.2559403858176));
#20598=CARTESIAN_POINT('Ctrl Pts',(-0.435682453834954,-1.94723787575538,
32.2525846785828));
#20599=CARTESIAN_POINT('Ctrl Pts',(-0.588928634873387,-1.90887174965014,
32.2418865279852));
#20600=CARTESIAN_POINT('Ctrl Pts',(-0.691111943997745,-1.87429682493267,
32.2343758941744));
#20601=CARTESIAN_POINT('Ctrl Pts',(-0.896020780072597,-1.78591908084901,
32.2188098426077));
#20602=CARTESIAN_POINT('Ctrl Pts',(-0.997889855101148,-1.73106406845087,
32.210784181256));
#20603=CARTESIAN_POINT('Ctrl Pts',(-1.10088223226489,-1.66347379643079,
32.2027394434066));
#20604=CARTESIAN_POINT('Ctrl Pts',(-1.10729042317245,-1.65921508073954,
32.2022392577582));
#20605=CARTESIAN_POINT('Ctrl Pts',(-1.11659991485968,-1.65295028087775,
32.2015133251425));
#20606=CARTESIAN_POINT('Ctrl Pts',(-1.11952069255584,-1.65097347656691,
32.201285672576));
#20607=CARTESIAN_POINT('Ctrl Pts',(-1.12461832191774,-1.64750361459868,
32.2008885528908));
#20608=CARTESIAN_POINT('Ctrl Pts',(-1.12679747047572,-1.64601397046622,
32.2007188564654));
#20609=CARTESIAN_POINT('Ctrl Pts',(-1.12898097269192,-1.64451498195596,
32.2005488901526));
#20610=CARTESIAN_POINT('Ctrl Pts',(-1.12898825439329,-1.64450998294956,
32.2005483233375));
#20611=CARTESIAN_POINT('Ctrl Pts',(-1.12900278842142,-1.64450000496019,
32.2005471919951));
#20612=CARTESIAN_POINT('Ctrl Pts',(-1.1290100235002,-1.64449503781967,32.2005466288105));
#20613=CARTESIAN_POINT('Ctrl Pts',(-1.12902444250486,-1.64448513851689,
32.2005455064246));
#20614=CARTESIAN_POINT('Ctrl Pts',(-1.12903162588245,-1.64448020673208,
32.200544947266));
#20615=CARTESIAN_POINT('Ctrl Pts',(-1.12904594255831,-1.64447037740662,
32.2005438328484));
#20616=CARTESIAN_POINT('Ctrl Pts',(-1.12905307499812,-1.64446548045636,
32.2005432776562));
#20617=CARTESIAN_POINT('Ctrl Pts',(-1.12906729000837,-1.64445572065878,
32.2005421711552));
#20618=CARTESIAN_POINT('Ctrl Pts',(-1.12907437195736,-1.64445085823911,
32.2005416198947));
#20619=CARTESIAN_POINT('Ctrl Pts',(-1.12908848677094,-1.64444116696661,
32.2005405211958));
#20620=CARTESIAN_POINT('Ctrl Pts',(-1.12909551887482,-1.64443633863705,
32.2005399738167));
#20621=CARTESIAN_POINT('Ctrl Pts',(-1.1291095343607,-1.64442671529867,32.2005388828523));
#20622=CARTESIAN_POINT('Ctrl Pts',(-1.12911651708822,-1.64442192074018,
32.200538339318));
#20623=CARTESIAN_POINT('Ctrl Pts',(-1.1291304345631,-1.64441236443739,32.2005372559856));
#20624=CARTESIAN_POINT('Ctrl Pts',(-1.12913736850178,-1.64440760324931,
32.2005367162504));
#20625=CARTESIAN_POINT('Ctrl Pts',(-1.12915118900127,-1.64439811327649,
32.2005356404692));
#20626=CARTESIAN_POINT('Ctrl Pts',(-1.12915807471961,-1.64439338507116,
32.2005351044888));
#20627=CARTESIAN_POINT('Ctrl Pts',(-1.12917179923596,-1.64438396075233,
32.2005340361815));
#20628=CARTESIAN_POINT('Ctrl Pts',(-1.12917863724504,-1.64437926518148,
32.2005335039161));
#20629=CARTESIAN_POINT('Ctrl Pts',(-1.12919226686039,-1.64436990577884,
32.2005324429986));
#20630=CARTESIAN_POINT('Ctrl Pts',(-1.12919905767014,-1.6443652424949,32.2005319144084));
#20631=CARTESIAN_POINT('Ctrl Pts',(-1.12921259344222,-1.64435594728726,
32.2005308607981));
#20632=CARTESIAN_POINT('Ctrl Pts',(-1.12921933755909,-1.64435131594502,
32.2005303358438));
#20633=CARTESIAN_POINT('Ctrl Pts',(-1.12923278057776,-1.64434208418906,
32.2005292894559));
#20634=CARTESIAN_POINT('Ctrl Pts',(-1.12923947855604,-1.64433748441039,
32.2005287680943));
#20635=CARTESIAN_POINT('Ctrl Pts',(-1.12925282977169,-1.64432831545842,
32.2005277288548));
#20636=CARTESIAN_POINT('Ctrl Pts',(-1.12925948214429,-1.64432374687984,
32.2005272110442));
#20637=CARTESIAN_POINT('Ctrl Pts',(-1.12927274232323,-1.64431464021051,
32.2005261788934));
#20638=CARTESIAN_POINT('Ctrl Pts',(-1.12927934941847,-1.64431010260896,
32.2005256646084));
#20639=CARTESIAN_POINT('Ctrl Pts',(-1.12929252005907,-1.64430105719805,
32.2005246394296));
#20640=CARTESIAN_POINT('Ctrl Pts',(-1.12929908254952,-1.64429655011401,
32.2005241286178));
#20641=CARTESIAN_POINT('Ctrl Pts',(-1.12931216417362,-1.64428756560787,
32.2005231103702));
#20642=CARTESIAN_POINT('Ctrl Pts',(-1.12931868246514,-1.64428308876495,
32.200522603));
#20643=CARTESIAN_POINT('Ctrl Pts',(-1.12933167610801,-1.6442741644572,32.2005215916031));
#20644=CARTESIAN_POINT('Ctrl Pts',(-1.12933815060729,-1.64426971757838,
32.2005210876428));
#20645=CARTESIAN_POINT('Ctrl Pts',(-1.1293510574228,-1.64426085268109,32.2005200830067));
#20646=CARTESIAN_POINT('Ctrl Pts',(-1.12935748867744,-1.64425643539254,
32.2005195824136));
#20647=CARTESIAN_POINT('Ctrl Pts',(-1.12937030945367,-1.64424762936891,
32.200518584477));
#20648=CARTESIAN_POINT('Ctrl Pts',(-1.12937669794717,-1.64424324134075,
32.2005180872135));
#20649=CARTESIAN_POINT('Ctrl Pts',(-1.12938943349152,-1.64423449364064,
32.2005170959134));
#20650=CARTESIAN_POINT('Ctrl Pts',(-1.12939577961846,-1.64423013460404,
32.2005166019487));
#20651=CARTESIAN_POINT('Ctrl Pts',(-1.12940843097335,-1.64422144451578,
32.200515617204));
#20652=CARTESIAN_POINT('Ctrl Pts',(-1.12941473520491,-1.64421711414925,
32.2005151265015));
#20653=CARTESIAN_POINT('Ctrl Pts',(-1.12942730314356,-1.64420848114597,
32.2005141482518));
#20654=CARTESIAN_POINT('Ctrl Pts',(-1.12943356585409,-1.64420417919449,
32.2005136607823));
#20655=CARTESIAN_POINT('Ctrl Pts',(-1.12944605151944,-1.6441956024953,32.2005126889388));
#20656=CARTESIAN_POINT('Ctrl Pts',(-1.1294522732779,-1.64419132857012,32.2005122046579));
#20657=CARTESIAN_POINT('Ctrl Pts',(-1.12946467714457,-1.64418280785311,
32.2005112391835));
#20658=CARTESIAN_POINT('Ctrl Pts',(-1.12947085825948,-1.64417856174433,
32.2005107580673));
#20659=CARTESIAN_POINT('Ctrl Pts',(-1.12948318152058,-1.64417009619397,
32.2005097988691));
#20660=CARTESIAN_POINT('Ctrl Pts',(-1.12948932251604,-1.64416587754357,
32.2005093208767));
#20661=CARTESIAN_POINT('Ctrl Pts',(-1.12950156574171,-1.64415746677216,
32.2005083679103));
#20662=CARTESIAN_POINT('Ctrl Pts',(-1.12950766696792,-1.64415327534155,
32.2005078930144));
#20663=CARTESIAN_POINT('Ctrl Pts',(-1.12951983107695,-1.64414491872184,
32.2005069462082));
#20664=CARTESIAN_POINT('Ctrl Pts',(-1.12952589290254,-1.64414075425971,
32.2005064743802));
#20665=CARTESIAN_POINT('Ctrl Pts',(-1.12953797887576,-1.64413245112173,
32.2005055336579));
#20666=CARTESIAN_POINT('Ctrl Pts',(-1.1295440017855,-1.64412831329696,32.2005050648599));
#20667=CARTESIAN_POINT('Ctrl Pts',(-1.12955601025092,-1.64412006321304,
32.2005041301725));
#20668=CARTESIAN_POINT('Ctrl Pts',(-1.12956199462572,-1.64411595176581,
32.200503664375));
#20669=CARTESIAN_POINT('Ctrl Pts',(-1.12957394363968,-1.64410774233429,
32.2005027343171));
#20670=CARTESIAN_POINT('Ctrl Pts',(-1.12957990721702,-1.64410364507931,
32.2005022701392));
#20671=CARTESIAN_POINT('Ctrl Pts',(-1.1295917289717,-1.64409552289097,32.2005013499885));
#20672=CARTESIAN_POINT('Ctrl Pts',(-1.12959763785162,-1.64409146312224,
32.2005008900692));
#20673=CARTESIAN_POINT('Ctrl Pts',(-1.12960941827893,-1.64408336914108,
32.2004999731372));
#20674=CARTESIAN_POINT('Ctrl Pts',(-1.1296152898331,-1.64407933492457,32.2004995161241));
#20675=CARTESIAN_POINT('Ctrl Pts',(-1.1321009175131,-1.64237149488527,32.200306047197));
#20676=CARTESIAN_POINT('Ctrl Pts',(-1.13457683593976,-1.64066206705954,
32.2001134205673));
#20677=CARTESIAN_POINT('Ctrl Pts',(-1.13967419220664,-1.63712568472626,
32.199717003506));
#20678=CARTESIAN_POINT('Ctrl Pts',(-1.14229512909805,-1.63529801881902,
32.199513261818));
#20679=CARTESIAN_POINT('Ctrl Pts',(-1.14887271143428,-1.63068772397597,
32.199002132005));
#20680=CARTESIAN_POINT('Ctrl Pts',(-1.15282367462965,-1.62789696742885,
32.1986952814134));
#20681=CARTESIAN_POINT('Ctrl Pts',(-1.16401445556548,-1.61993120340002,
32.1978265156498));
#20682=CARTESIAN_POINT('Ctrl Pts',(-1.17122995375882,-1.614722006613,32.1972667944543));
#20683=CARTESIAN_POINT('Ctrl Pts',(-1.24446582675881,-1.56110049638963,
32.1915874758735));
#20684=CARTESIAN_POINT('Ctrl Pts',(-1.30748957121274,-1.50870946941751,
32.1867131744928));
#20685=CARTESIAN_POINT('Ctrl Pts',(-1.44765094977023,-1.37679474645003,
32.1754366363088));
#20686=CARTESIAN_POINT('Ctrl Pts',(-1.52173848995551,-1.29443790360402,
32.1691098508864));
#20687=CARTESIAN_POINT('Ctrl Pts',(-1.64701158555818,-1.12947014584585,
32.1569270686873));
#20688=CARTESIAN_POINT('Ctrl Pts',(-1.69973627328369,-1.04844779328467,
32.151130689616));
#20689=CARTESIAN_POINT('Ctrl Pts',(-1.75252351357761,-0.952811781841404,
32.1443103111423));
#20690=CARTESIAN_POINT('Ctrl Pts',(-1.75855608767532,-0.941631261088707,
32.1435134312328));
#20691=CARTESIAN_POINT('Ctrl Pts',(-1.76736660344698,-0.924922222399464,
32.1423228823436));
#20692=CARTESIAN_POINT('Ctrl Pts',(-1.77022636685033,-0.919437021864666,
32.1419321112741));
#20693=CARTESIAN_POINT('Ctrl Pts',(-1.77527689745009,-0.909638884477386,
32.1412341480227));
#20694=CARTESIAN_POINT('Ctrl Pts',(-1.77747758669201,-0.905331094630736,
32.1409273082408));
#20695=CARTESIAN_POINT('Ctrl Pts',(-1.78208293023251,-0.896234737610973,
32.1402794100404));
#20696=CARTESIAN_POINT('Ctrl Pts',(-1.78448399889495,-0.891444407627698,
32.1399382289148));
#20697=CARTESIAN_POINT('Ctrl Pts',(-1.79078082460493,-0.878754336242574,
32.139034413736));
#20698=CARTESIAN_POINT('Ctrl Pts',(-1.79464357499126,-0.870838434987936,
32.1384706336672));
#20699=CARTESIAN_POINT('Ctrl Pts',(-1.81215283604656,-0.834345569413666,
32.1358713832743));
#20700=CARTESIAN_POINT('Ctrl Pts',(-1.82516939072008,-0.805473111825947,
32.133814284664));
#20701=CARTESIAN_POINT('Ctrl Pts',(-1.85840050842208,-0.726815907048204,
32.1282047784031));
#20702=CARTESIAN_POINT('Ctrl Pts',(-1.87729889687107,-0.676507060522405,
32.1246106897333));
#20703=CARTESIAN_POINT('Ctrl Pts',(-1.92407777126974,-0.534851104395849,
32.114479852037));
#20704=CARTESIAN_POINT('Ctrl Pts',(-1.94746455250535,-0.442176494784212,
32.1078338879887));
#20705=CARTESIAN_POINT('Ctrl Pts',(-1.98451431995775,-0.233181474814436,
32.093024626058));
#20706=CARTESIAN_POINT('Ctrl Pts',(-1.99476346756107,-0.11659257845761,
32.0848797877451));
#20707=CARTESIAN_POINT('Ctrl Pts',(-1.99474998671879,0.000230185530924812,
32.0772014385531));
#20708=CARTESIAN_POINT('',(-1.99474934552561,0.000704641662985501,30.4808452152674));
#20709=CARTESIAN_POINT('Ctrl Pts',(-1.99474998656482,0.000231515990512227,
32.0772013511067));
#20710=CARTESIAN_POINT('Ctrl Pts',(-1.99474932987922,0.00588954239274279,
32.0768294691232));
#20711=CARTESIAN_POINT('Ctrl Pts',(-1.994724600045,0.0115476292319622,32.0764587444995));
#20712=CARTESIAN_POINT('Ctrl Pts',(-1.99462718926037,0.0228406201405742,
32.0757212328955));
#20713=CARTESIAN_POINT('Ctrl Pts',(-1.99455470408963,0.0284754680534856,
32.0753544397563));
#20714=CARTESIAN_POINT('Ctrl Pts',(-1.99440133338182,0.0374432595348793,
32.0747726862233));
#20715=CARTESIAN_POINT('Ctrl Pts',(-1.99433597042751,0.0407763869072901,
32.0745568997712));
#20716=CARTESIAN_POINT('Ctrl Pts',(-1.99420454227825,0.0467184856729034,
32.0741730088618));
#20717=CARTESIAN_POINT('Ctrl Pts',(-1.99414171269055,0.049327510029208,
32.0740047271924));
#20718=CARTESIAN_POINT('Ctrl Pts',(-1.99400421729553,0.0546065791285882,
32.073664794882));
#20719=CARTESIAN_POINT('Ctrl Pts',(-1.99392930885807,0.0572765976941349,
32.0734931603565));
#20720=CARTESIAN_POINT('Ctrl Pts',(-1.99375553841236,0.0630562843716036,
32.0731222703868));
#20721=CARTESIAN_POINT('Ctrl Pts',(-1.99365476469498,0.066165863417449,
32.0729231237206));
#20722=CARTESIAN_POINT('Ctrl Pts',(-1.99336115179429,0.0746152199705355,
32.0723830554699));
#20723=CARTESIAN_POINT('Ctrl Pts',(-1.9931541304564,0.0799545268342738,
32.0720429198772));
#20724=CARTESIAN_POINT('Ctrl Pts',(-1.99217525128507,0.102826663548703,
32.0705905258563));
#20725=CARTESIAN_POINT('Ctrl Pts',(-1.99119345952562,0.120350371331074,
32.0694894798816));
#20726=CARTESIAN_POINT('Ctrl Pts',(-1.97561090389686,0.345282062007617,
32.0554811198056));
#20727=CARTESIAN_POINT('Ctrl Pts',(-1.92889957127704,0.549212799457698,
32.0440269275762));
#20728=CARTESIAN_POINT('Ctrl Pts',(-1.83237428774714,0.78998399887494,32.0286128687338));
#20729=CARTESIAN_POINT('Ctrl Pts',(-1.81140904770275,0.836939007320726,
32.0255168011908));
#20730=CARTESIAN_POINT('Ctrl Pts',(-1.77507594953448,0.91053494018854,32.0204793993337));
#20731=CARTESIAN_POINT('Ctrl Pts',(-1.76086491394984,0.937722292929969,
32.0185767066792));
#20732=CARTESIAN_POINT('Ctrl Pts',(-1.74182122376156,0.972194559216066,
32.0161052199152));
#20733=CARTESIAN_POINT('Ctrl Pts',(-1.73755934879876,0.979791274731646,
32.0155568306202));
#20734=CARTESIAN_POINT('Ctrl Pts',(-1.73060635186003,0.991996823480004,
32.0146695752303));
#20735=CARTESIAN_POINT('Ctrl Pts',(-1.72794621815228,0.996623253372562,
32.014331826881));
#20736=CARTESIAN_POINT('Ctrl Pts',(-1.72283701144074,1.00542709480778,32.0136863307224));
#20737=CARTESIAN_POINT('Ctrl Pts',(-1.72039122622048,1.00960637826224,32.0133787037177));
#20738=CARTESIAN_POINT('Ctrl Pts',(-1.71476576295487,1.01913920116737,32.0126742388898));
#20739=CARTESIAN_POINT('Ctrl Pts',(-1.71157619948137,1.02448682035149,32.0122770429992));
#20740=CARTESIAN_POINT('Ctrl Pts',(-1.70169628416991,1.04087655746113,32.0110534303641));
#20741=CARTESIAN_POINT('Ctrl Pts',(-1.69492382970594,1.0518685516234,32.0102240136365));
#20742=CARTESIAN_POINT('Ctrl Pts',(-1.61418203494577,1.1801114931882,32.0004419309435));
#20743=CARTESIAN_POINT('Ctrl Pts',(-1.52830547945784,1.28938546386611,31.9910249156142));
#20744=CARTESIAN_POINT('Ctrl Pts',(-1.36087498114351,1.46199469660722,31.9743119575535));
#20745=CARTESIAN_POINT('Ctrl Pts',(-1.28443323552939,1.52958856444278,31.9671500677009));
#20746=CARTESIAN_POINT('Ctrl Pts',(-1.17207749735467,1.61455275352589,31.9574998582312));
#20747=CARTESIAN_POINT('Ctrl Pts',(-1.14030973197873,1.63714396882882,31.9548598208094));
#20748=CARTESIAN_POINT('Ctrl Pts',(-1.09634345469721,1.66650882697449,31.9513441312956));
#20749=CARTESIAN_POINT('Ctrl Pts',(-1.0847077501933,1.67410566041631,31.9504264001781));
#20750=CARTESIAN_POINT('Ctrl Pts',(-1.06737772965087,1.68516370659574,31.9490792947103));
#20751=CARTESIAN_POINT('Ctrl Pts',(-1.06174420241356,1.68871880056284,31.9486444337705));
#20752=CARTESIAN_POINT('Ctrl Pts',(-1.0527423915626,1.6943366304862,31.9479545399262));
#20753=CARTESIAN_POINT('Ctrl Pts',(-1.04938566701543,1.69641766169301,31.9476983757351));
#20754=CARTESIAN_POINT('Ctrl Pts',(-1.04300600898862,1.7003466058827,31.9472136235588));
#20755=CARTESIAN_POINT('Ctrl Pts',(-1.03998429523219,1.70219645783603,31.9469849121348));
#20756=CARTESIAN_POINT('Ctrl Pts',(-1.03467837933972,1.70542526444898,31.9465848919186));
#20757=CARTESIAN_POINT('Ctrl Pts',(-1.03239631937592,1.70680769900328,31.9464133553995));
#20758=CARTESIAN_POINT('Ctrl Pts',(-1.02756386012961,1.70972188567511,31.9460511995249));
#20759=CARTESIAN_POINT('Ctrl Pts',(-1.0250128102914,1.71125250972027,31.9458606541848));
#20760=CARTESIAN_POINT('Ctrl Pts',(-1.01827427440553,1.71527514102252,31.9453589835437));
#20761=CARTESIAN_POINT('Ctrl Pts',(-1.01408103210372,1.71775754076702,31.9450484810027));
#20762=CARTESIAN_POINT('Ctrl Pts',(-0.998711409218007,1.72678046409516,
31.9439163434955));
#20763=CARTESIAN_POINT('Ctrl Pts',(-0.987480213083196,1.73322765377137,
31.9431005227049));
#20764=CARTESIAN_POINT('Ctrl Pts',(-0.819987389136426,1.82721910786742,
31.9310911721451));
#20765=CARTESIAN_POINT('Ctrl Pts',(-0.652667827218758,1.89345083260286,
31.9210544744051));
#20766=CARTESIAN_POINT('Ctrl Pts',(-0.452517921620162,1.94293183270706,
31.9089894693175));
#20767=CARTESIAN_POINT('Ctrl Pts',(-0.426178454825232,1.94887876559413,
31.9074021201945));
#20768=CARTESIAN_POINT('Ctrl Pts',(-0.344629904279162,1.96555856505706,
31.9024745610374));
#20769=CARTESIAN_POINT('Ctrl Pts',(-0.289084820663625,1.97449219896898,
31.8990991878472));
#20770=CARTESIAN_POINT('Ctrl Pts',(-0.200738904723304,1.98489354711158,
31.8936488041727));
#20771=CARTESIAN_POINT('Ctrl Pts',(-0.168150524710556,1.98791944227067,
31.8916211236522));
#20772=CARTESIAN_POINT('Ctrl Pts',(-0.126615798296741,1.99074743904478,
31.8890092960904));
#20773=CARTESIAN_POINT('Ctrl Pts',(-0.11772389657387,1.99129304886842,31.8884485562656));
#20774=CARTESIAN_POINT('Ctrl Pts',(-0.10345596619214,1.99207263386072,31.8875461302064));
#20775=CARTESIAN_POINT('Ctrl Pts',(-0.0980820570298916,1.99234445432535,
31.8872056326682));
#20776=CARTESIAN_POINT('Ctrl Pts',(-0.0878796428655608,1.99281913032875,
31.8865580190796));
#20777=CARTESIAN_POINT('Ctrl Pts',(-0.0830513642794613,1.99302618850091,
31.8862510371584));
#20778=CARTESIAN_POINT('Ctrl Pts',(-0.0720812443907305,1.99345670351143,
31.8855524005117));
#20779=CARTESIAN_POINT('Ctrl Pts',(-0.065939049774496,1.99366932435777,
31.8851604090009));
#20780=CARTESIAN_POINT('Ctrl Pts',(-0.0500708889735416,1.99414521335601,
31.8841455393411));
#20781=CARTESIAN_POINT('Ctrl Pts',(-0.0403438936627081,1.99436571133372,
31.883521328235));
#20782=CARTESIAN_POINT('Ctrl Pts',(0.0200043326713027,1.99529205690601,
31.8796351459475));
#20783=CARTESIAN_POINT('Ctrl Pts',(0.0706314838680484,1.99414166668733,
31.8763155430744));
#20784=CARTESIAN_POINT('Ctrl Pts',(0.13409283830146,1.99028004094122,31.8720756688003));
#20785=CARTESIAN_POINT('Ctrl Pts',(0.147020947832433,1.98936682378843,31.8712078650238));
#20786=CARTESIAN_POINT('Ctrl Pts',(0.3242919908657,1.97510732536553,31.8592530943559));
#20787=CARTESIAN_POINT('Ctrl Pts',(0.486360859213983,1.94155965709629,31.8475927555112));
#20788=CARTESIAN_POINT('Ctrl Pts',(0.704559251501132,1.86733280074355,31.8316820308599));
#20789=CARTESIAN_POINT('Ctrl Pts',(0.765623194195359,1.84313821951995,31.827214800699));
#20790=CARTESIAN_POINT('Ctrl Pts',(0.832633692061753,1.81268089633509,31.8223765657941));
#20791=CARTESIAN_POINT('Ctrl Pts',(0.83985911683253,1.80934451277659,31.8218557556634));
#20792=CARTESIAN_POINT('Ctrl Pts',(0.851111242574038,1.80406684850361,31.8210462878835));
#20793=CARTESIAN_POINT('Ctrl Pts',(0.855151620779874,1.80215516743265,31.8207559483549));
#20794=CARTESIAN_POINT('Ctrl Pts',(0.861932017097704,1.79891912586887,31.8202692962759));
#20795=CARTESIAN_POINT('Ctrl Pts',(0.864675467753168,1.79760205809845,31.820072550747));
#20796=CARTESIAN_POINT('Ctrl Pts',(0.870027459364532,1.79501760241953,31.8196890655342));
#20797=CARTESIAN_POINT('Ctrl Pts',(0.872636270319368,1.79375079457314,31.8195022909254));
#20798=CARTESIAN_POINT('Ctrl Pts',(0.877614082183783,1.79132019796685,31.8191462183624));
#20799=CARTESIAN_POINT('Ctrl Pts',(0.879983531011061,1.79015739925545,31.8189768622947));
#20800=CARTESIAN_POINT('Ctrl Pts',(0.88554676306466,1.78741354832691,31.8185795362488));
#20801=CARTESIAN_POINT('Ctrl Pts',(0.888738647033779,1.78582862561535,31.8183518081015));
#20802=CARTESIAN_POINT('Ctrl Pts',(0.898726561545294,1.78083573908963,31.8176398980057));
#20803=CARTESIAN_POINT('Ctrl Pts',(0.905507467644321,1.77739742110228,31.8171575744244));
#20804=CARTESIAN_POINT('Ctrl Pts',(1.01453463699822,1.72132834689195,31.8094160083485));
#20805=CARTESIAN_POINT('Ctrl Pts',(1.1120785330888,1.65998241239724,31.8026757435883));
#20806=CARTESIAN_POINT('Ctrl Pts',(1.28573768120921,1.52854991539803,31.7900165540472));
#20807=CARTESIAN_POINT('Ctrl Pts',(1.36275497706805,1.46030277563428,31.7841037038883));
#20808=CARTESIAN_POINT('Ctrl Pts',(1.47159155681531,1.34771828524721,31.7748167041358));
#20809=CARTESIAN_POINT('Ctrl Pts',(1.50742722730279,1.30751243014434,31.7715797750089));
#20810=CARTESIAN_POINT('Ctrl Pts',(1.561719604958,1.24139656868197,31.7663336591272));
#20811=CARTESIAN_POINT('Ctrl Pts',(1.58125975683932,1.21640904722309,31.764367372882));
#20812=CARTESIAN_POINT('Ctrl Pts',(1.60545683242319,1.18389762598168,31.7618244111468));
#20813=CARTESIAN_POINT('Ctrl Pts',(1.61067159959475,1.17679319501088,31.7612696413601));
#20814=CARTESIAN_POINT('Ctrl Pts',(1.61898167184888,1.16531310503677,31.7603745490021));
#20815=CARTESIAN_POINT('Ctrl Pts',(1.6221067578795,1.16095906546276,31.7600353806108));
#20816=CARTESIAN_POINT('Ctrl Pts',(1.62801890286672,1.15265147049618,31.7593888060741));
#20817=CARTESIAN_POINT('Ctrl Pts',(1.63080920635282,1.14870026217724,31.7590815276597));
#20818=CARTESIAN_POINT('Ctrl Pts',(1.63713393948355,1.13967463275887,31.7583801476378));
#20819=CARTESIAN_POINT('Ctrl Pts',(1.64065918552692,1.13459386561254,31.7579856992061));
#20820=CARTESIAN_POINT('Ctrl Pts',(1.65134865273557,1.11903366082132,31.7567787651803));
#20821=CARTESIAN_POINT('Ctrl Pts',(1.65843640410259,1.10850231759122,31.7559633971537));
#20822=CARTESIAN_POINT('Ctrl Pts',(1.7489937813781,0.971134835711256,31.7453456141375));
#20823=CARTESIAN_POINT('Ctrl Pts',(1.81779951396931,0.835265570101009,31.7349781352055));
#20824=CARTESIAN_POINT('Ctrl Pts',(1.90336458059826,0.604291428588858,31.7178187847069));
#20825=CARTESIAN_POINT('Ctrl Pts',(1.92986256383391,0.513416539776491,31.7111890253457));
#20826=CARTESIAN_POINT('Ctrl Pts',(1.95724109497874,0.386616581873011,31.7023309743702));
#20827=CARTESIAN_POINT('Ctrl Pts',(1.96375525272594,0.352037931230871,31.6999551804326));
#20828=CARTESIAN_POINT('Ctrl Pts',(1.97245684607242,0.298031201910524,31.6963236815515));
#20829=CARTESIAN_POINT('Ctrl Pts',(1.97527902302628,0.278713937229114,31.6950403770361));
#20830=CARTESIAN_POINT('Ctrl Pts',(1.97847987220997,0.254304790513559,31.6934410545095));
#20831=CARTESIAN_POINT('Ctrl Pts',(1.97912309243677,0.249249508709049,31.6931110254362));
#20832=CARTESIAN_POINT('Ctrl Pts',(1.98011723139521,0.241189680478594,31.6925868190158));
#20833=CARTESIAN_POINT('Ctrl Pts',(1.98048069557435,0.238186747730455,31.6923919457197));
#20834=CARTESIAN_POINT('Ctrl Pts',(1.98115674019984,0.232492736804073,31.6920232772764));
#20835=CARTESIAN_POINT('Ctrl Pts',(1.9814706652022,0.229801881924157,31.691849410787));
#20836=CARTESIAN_POINT('Ctrl Pts',(1.98217671359029,0.223640859504411,31.6914521303368));
#20837=CARTESIAN_POINT('Ctrl Pts',(1.98256520631736,0.220170300206956,31.6912289230298));
#20838=CARTESIAN_POINT('Ctrl Pts',(1.98357278248761,0.210950274180009,31.6906374504553));
#20839=CARTESIAN_POINT('Ctrl Pts',(1.98417598827319,0.205199052488333,31.690270061884));
#20840=CARTESIAN_POINT('Ctrl Pts',(1.98813200801416,0.165831213238705,31.687765391635));
#20841=CARTESIAN_POINT('Ctrl Pts',(1.99065559639091,0.132134391251426,31.6856721203616));
#20842=CARTESIAN_POINT('Ctrl Pts',(1.99562692760634,0.031466058776295,31.6795259671994));
#20843=CARTESIAN_POINT('Ctrl Pts',(1.99555809048951,-0.035584830233128,
31.6755729127611));
#20844=CARTESIAN_POINT('Ctrl Pts',(1.99107210310318,-0.122762840000178,
31.6704768439513));
#20845=CARTESIAN_POINT('Ctrl Pts',(1.98972112004744,-0.142998997611173,
31.6692970713786));
#20846=CARTESIAN_POINT('Ctrl Pts',(1.97976899638068,-0.264224974468188,
31.6622321539425));
#20847=CARTESIAN_POINT('Ctrl Pts',(1.9637895730272,-0.364457916836624,31.6563926683583));
#20848=CARTESIAN_POINT('Ctrl Pts',(1.92818124007526,-0.513667176439659,
31.6472820783049));
#20849=CARTESIAN_POINT('Ctrl Pts',(1.91412251887782,-0.563800688808152,
31.6441486884623));
#20850=CARTESIAN_POINT('Ctrl Pts',(1.88860327018468,-0.642777820640292,
31.639055897928));
#20851=CARTESIAN_POINT('Ctrl Pts',(1.87840241391484,-0.672004349617054,
31.6371362431469));
#20852=CARTESIAN_POINT('Ctrl Pts',(1.86445542762859,-0.709161389761481,
31.6346456773719));
#20853=CARTESIAN_POINT('Ctrl Pts',(1.86133103675602,-0.717321884537835,
31.6340955661206));
#20854=CARTESIAN_POINT('Ctrl Pts',(1.85621005210657,-0.730438464894457,
31.6332061958353));
#20855=CARTESIAN_POINT('Ctrl Pts',(1.8542469632508,-0.735407578766996,31.6328680643335));
#20856=CARTESIAN_POINT('Ctrl Pts',(1.85046720699997,-0.744863821553946,
31.6322222805818));
#20857=CARTESIAN_POINT('Ctrl Pts',(1.84865411983734,-0.749352347945748,
31.631914751015));
#20858=CARTESIAN_POINT('Ctrl Pts',(1.84447605377035,-0.759588227052796,
31.6312111348816));
#20859=CARTESIAN_POINT('Ctrl Pts',(1.84210052650984,-0.76533119392625,31.6308146933366));
#20860=CARTESIAN_POINT('Ctrl Pts',(1.83473065726099,-0.782915148664882,
31.6295956728241));
#20861=CARTESIAN_POINT('Ctrl Pts',(1.82964877136552,-0.794718865569783,
31.6287701264769));
#20862=CARTESIAN_POINT('Ctrl Pts',(1.78188328349275,-0.902776993825045,
31.6211444719937));
#20863=CARTESIAN_POINT('Ctrl Pts',(1.73176238653417,-0.995543496451416,
31.6140847890614));
#20864=CARTESIAN_POINT('Ctrl Pts',(1.60324587333483,-1.19409242715677,31.5978204037459));
#20865=CARTESIAN_POINT('Ctrl Pts',(1.52123133386611,-1.29696072433048,31.5885470917199));
#20866=CARTESIAN_POINT('Ctrl Pts',(1.40054849237707,-1.42099976620114,31.5766648428988));
#20867=CARTESIAN_POINT('Ctrl Pts',(1.37044861020676,-1.45005086325532,31.5738255520883));
#20868=CARTESIAN_POINT('Ctrl Pts',(1.32313420684551,-1.49292617800254,31.5695747720104));
#20869=CARTESIAN_POINT('Ctrl Pts',(1.3065680269435,-1.50744578453689,31.5681239517869));
#20870=CARTESIAN_POINT('Ctrl Pts',(1.28571660851249,-1.52511918017284,31.5663473636237));
#20871=CARTESIAN_POINT('Ctrl Pts',(1.28165557607537,-1.52853351190485,31.5660036373573));
#20872=CARTESIAN_POINT('Ctrl Pts',(1.27522208916417,-1.53389882967076,31.5654627654761));
#20873=CARTESIAN_POINT('Ctrl Pts',(1.27285870498995,-1.53586057759228,31.5652648466817));
#20874=CARTESIAN_POINT('Ctrl Pts',(1.26840950490099,-1.53953635185446,31.5648937209171));
#20875=CARTESIAN_POINT('Ctrl Pts',(1.26632476502626,-1.54125158244618,31.5647204283514));
#20876=CARTESIAN_POINT('Ctrl Pts',(1.2615515846922,-1.54516251899288,31.5643250302089));
#20877=CARTESIAN_POINT('Ctrl Pts',(1.25886089618895,-1.54735543926808,31.5641031273757));
#20878=CARTESIAN_POINT('Ctrl Pts',(1.25056586835105,-1.55407995765512,31.5634220123758));
#20879=CARTESIAN_POINT('Ctrl Pts',(1.24494260511389,-1.5585882777907,31.562964448366));
#20880=CARTESIAN_POINT('Ctrl Pts',(1.19884777812114,-1.59513509121953,31.5592464479872));
#20881=CARTESIAN_POINT('Ctrl Pts',(1.15716698768159,-1.6256252873362,31.5560891392314));
#20882=CARTESIAN_POINT('Ctrl Pts',(1.05664667721089,-1.69332953472336,31.5488208749054));
#20883=CARTESIAN_POINT('Ctrl Pts',(0.996950117854174,-1.72914970939522,
31.5447640587105));
#20884=CARTESIAN_POINT('Ctrl Pts',(0.846401056888334,-1.80909092962046,
31.5348654168885));
#20885=CARTESIAN_POINT('Ctrl Pts',(0.753842344734532,-1.84957437193072,
31.5290506260312));
#20886=CARTESIAN_POINT('Ctrl Pts',(0.610053791048967,-1.89987092979403,
31.5199991077975));
#20887=CARTESIAN_POINT('Ctrl Pts',(0.560848489754028,-1.91497350872426,
31.5169002616554));
#20888=CARTESIAN_POINT('Ctrl Pts',(0.481446276305041,-1.93602150297413,
31.5118587339682));
#20889=CARTESIAN_POINT('Ctrl Pts',(0.451599283421843,-1.94320037663654,
31.5099547756967));
#20890=CARTESIAN_POINT('Ctrl Pts',(0.413083940313299,-1.95152892133551,
31.5074818649995));
#20891=CARTESIAN_POINT('Ctrl Pts',(0.404556263970177,-1.95331454147972,
31.506933346721));
#20892=CARTESIAN_POINT('Ctrl Pts',(0.390786345207502,-1.95610380097916,
31.5060459329258));
#20893=CARTESIAN_POINT('Ctrl Pts',(0.38555122999224,-1.95714238009246,31.5057081558867));
#20894=CARTESIAN_POINT('Ctrl Pts',(0.375558622648085,-1.95908313525623,
31.5050626382961));
#20895=CARTESIAN_POINT('Ctrl Pts',(0.370801883327998,-1.95998902357429,
31.5047550186901));
#20896=CARTESIAN_POINT('Ctrl Pts',(0.359921917649469,-1.96202001400915,
31.5040506178922));
#20897=CARTESIAN_POINT('Ctrl Pts',(0.353796651658854,-1.96313378301105,
31.5036534788658));
#20898=CARTESIAN_POINT('Ctrl Pts',(0.334957564206822,-1.9664682975837,31.502430212694));
#20899=CARTESIAN_POINT('Ctrl Pts',(0.322227523103384,-1.96859430700155,
31.5016010880314));
#20900=CARTESIAN_POINT('Ctrl Pts',(0.170028513222552,-1.9924968368546,31.4916563390715));
#20901=CARTESIAN_POINT('Ctrl Pts',(0.0286774136200812,-1.99952892784342,
31.4820580445661));
#20902=CARTESIAN_POINT('Ctrl Pts',(-0.210491895795797,-1.98605432024905,
31.4654002604322));
#20903=CARTESIAN_POINT('Ctrl Pts',(-0.308235481518195,-1.9732486449967,
31.4584850060521));
#20904=CARTESIAN_POINT('Ctrl Pts',(-0.46157151644206,-1.9414839997497,31.4477517363439));
#20905=CARTESIAN_POINT('Ctrl Pts',(-0.517971100143095,-1.92720414045988,
31.4438316777563));
#20906=CARTESIAN_POINT('Ctrl Pts',(-0.580203089146887,-1.90851734176708,
31.4395952660623));
#20907=CARTESIAN_POINT('Ctrl Pts',(-0.58672453187955,-1.90652259243112,
31.4391524400644));
#20908=CARTESIAN_POINT('Ctrl Pts',(-0.59647594995493,-1.9034850987971,31.4384920996695));
#20909=CARTESIAN_POINT('Ctrl Pts',(-0.599713618008486,-1.90246751799136,
31.4382731532227));
#20910=CARTESIAN_POINT('Ctrl Pts',(-0.605271195297765,-1.90070520570508,
31.4378978582564));
#20911=CARTESIAN_POINT('Ctrl Pts',(-0.607592345539976,-1.899964484072,31.4377412756485));
#20912=CARTESIAN_POINT('Ctrl Pts',(-0.612431723787028,-1.89841037424143,
31.4374151559839));
#20913=CARTESIAN_POINT('Ctrl Pts',(-0.614949681751742,-1.89759623061437,
31.4372456647642));
#20914=CARTESIAN_POINT('Ctrl Pts',(-0.621947166007032,-1.89531830935224,
31.436775154913));
#20915=CARTESIAN_POINT('Ctrl Pts',(-0.62642317359611,-1.89384365240303,
31.4364747725742));
#20916=CARTESIAN_POINT('Ctrl Pts',(-0.644326673098439,-1.8878747823889,
31.4352754612713));
#20917=CARTESIAN_POINT('Ctrl Pts',(-0.657711771778033,-1.88325338396664,
31.4343837518552));
#20918=CARTESIAN_POINT('Ctrl Pts',(-0.787200198933685,-1.83699663954138,
31.4257948963618));
#20919=CARTESIAN_POINT('Ctrl Pts',(-0.89927260918478,-1.78481330801568,
31.4186463048127));
#20920=CARTESIAN_POINT('Ctrl Pts',(-1.07591327940762,-1.68167375565586,
31.4067818551141));
#20921=CARTESIAN_POINT('Ctrl Pts',(-1.14344308049151,-1.63650639793599,
31.4020835874523));
#20922=CARTESIAN_POINT('Ctrl Pts',(-1.25308478655208,-1.55306520834449,
31.3939293295779));
#20923=CARTESIAN_POINT('Ctrl Pts',(-1.29665512215616,-1.51687762805256,
31.3905321066451));
#20924=CARTESIAN_POINT('Ctrl Pts',(-1.3630040696393,-1.45682145119373,31.3850495607634));
#20925=CARTESIAN_POINT('Ctrl Pts',(-1.38683242177852,-1.43415636259705,
31.3830122891388));
#20926=CARTESIAN_POINT('Ctrl Pts',(-1.41640029398225,-1.40460577948084,
31.3803897148444));
#20927=CARTESIAN_POINT('Ctrl Pts',(-1.42266941292446,-1.39825567258185,
31.3798280586367));
#20928=CARTESIAN_POINT('Ctrl Pts',(-1.43265244285895,-1.38800703482086,
31.3789245068296));
#20929=CARTESIAN_POINT('Ctrl Pts',(-1.43639359200502,-1.38413510852872,
31.3785838052613));
#20930=CARTESIAN_POINT('Ctrl Pts',(-1.44346251219736,-1.37675956053643,
31.3779360297551));
#20931=CARTESIAN_POINT('Ctrl Pts',(-1.44679332282461,-1.37325889474734,
31.377629090922));
#20932=CARTESIAN_POINT('Ctrl Pts',(-1.45432767863913,-1.36528248638433,
31.3769308636938));
#20933=CARTESIAN_POINT('Ctrl Pts',(-1.45852332814274,-1.36079938431561,
31.3765392400153));
#20934=CARTESIAN_POINT('Ctrl Pts',(-1.46930089936719,-1.34917631541821,
31.3755259408891));
#20935=CARTESIAN_POINT('Ctrl Pts',(-1.47585144033371,-1.34200759442334,
31.374902939348));
#20936=CARTESIAN_POINT('Ctrl Pts',(-1.51602220034926,-1.29739605753985,
31.3710376558577));
#20937=CARTESIAN_POINT('Ctrl Pts',(-1.5482652143614,-1.25874298781197,31.3677384518195));
#20938=CARTESIAN_POINT('Ctrl Pts',(-1.581718129923,-1.21540732136719,31.3640884223525));
#20939=CARTESIAN_POINT('Ctrl Pts',(-1.58441424422324,-1.21189054851352,
31.3637925590055));
#20940=CARTESIAN_POINT('Ctrl Pts',(-1.70256778802969,-1.05670453392889,
31.3507520080083));
#20941=CARTESIAN_POINT('Ctrl Pts',(-1.79569444202854,-0.889281258320573,
31.3371804596772));
#20942=CARTESIAN_POINT('Ctrl Pts',(-1.88362453382085,-0.658883659700334,
31.3202981224338));
#20943=CARTESIAN_POINT('Ctrl Pts',(-1.90139569462875,-0.605693662426969,
31.3165239749815));
#20944=CARTESIAN_POINT('Ctrl Pts',(-1.91877776054363,-0.545312145725606,
31.3124276778312));
#20945=CARTESIAN_POINT('Ctrl Pts',(-1.92061818384855,-0.538794233186789,
31.3119879274492));
#20946=CARTESIAN_POINT('Ctrl Pts',(-1.92332844373332,-0.529005400046055,
31.3113312597949));
#20947=CARTESIAN_POINT('Ctrl Pts',(-1.92422318698944,-0.525741517116593,
31.3111129335879));
#20948=CARTESIAN_POINT('Ctrl Pts',(-1.92574748754049,-0.520125088124526,
31.3107383365297));
#20949=CARTESIAN_POINT('Ctrl Pts',(-1.92638104533116,-0.517773658554759,
31.3105818341014));
#20950=CARTESIAN_POINT('Ctrl Pts',(-1.92769521510163,-0.512860357549892,
31.3102555155233));
#20951=CARTESIAN_POINT('Ctrl Pts',(-1.92837502452724,-0.510298298696599,
31.3100857464631));
#20952=CARTESIAN_POINT('Ctrl Pts',(-1.93025483769002,-0.503156277813248,
31.3096135656816));
#20953=CARTESIAN_POINT('Ctrl Pts',(-1.93144365571775,-0.498573348893381,
31.3093117978475));
#20954=CARTESIAN_POINT('Ctrl Pts',(-1.93616370941818,-0.480107139642457,
31.3081006307306));
#20955=CARTESIAN_POINT('Ctrl Pts',(-1.93956177019594,-0.466189814395688,
31.3071986315439));
#20956=CARTESIAN_POINT('Ctrl Pts',(-1.97718139378684,-0.304575809792007,
31.2968363213099));
#20957=CARTESIAN_POINT('Ctrl Pts',(-1.99461257580312,-0.153453721871375,
31.2882019858445));
#20958=CARTESIAN_POINT('Ctrl Pts',(-1.99487121963617,0.133668057474652,
31.2715168899994));
#20959=CARTESIAN_POINT('Ctrl Pts',(-1.98119470743788,0.268771501879354,
31.2635403645652));
#20960=CARTESIAN_POINT('Ctrl Pts',(-1.95133019524141,0.414132853595452,
31.2542776850415));
#20961=CARTESIAN_POINT('Ctrl Pts',(-1.94859819998239,0.426802757355567,
31.2534648555655));
#20962=CARTESIAN_POINT('Ctrl Pts',(-1.94436908622295,0.445528127312583,
31.2522550623641));
#20963=CARTESIAN_POINT('Ctrl Pts',(-1.94296668611304,0.45160481718661,31.2518611367817));
#20964=CARTESIAN_POINT('Ctrl Pts',(-1.94042451122363,0.46238916426216,31.2511596319364));
#20965=CARTESIAN_POINT('Ctrl Pts',(-1.93929603746011,0.467099455574493,
31.2508524184245));
#20966=CARTESIAN_POINT('Ctrl Pts',(-1.93688937859238,0.476985873508292,
31.2502058714525));
#20967=CARTESIAN_POINT('Ctrl Pts',(-1.93560757595444,0.48216107207886,31.2498664234468));
#20968=CARTESIAN_POINT('Ctrl Pts',(-1.93218260267122,0.495755410904218,
31.2489720813532));
#20969=CARTESIAN_POINT('Ctrl Pts',(-1.9300051697685,0.504165724948014,31.2484160839992));
#20970=CARTESIAN_POINT('Ctrl Pts',(-1.91994968956288,0.541984961347442,
31.2459034973414));
#20971=CARTESIAN_POINT('Ctrl Pts',(-1.9114542615777,0.571224075328402,31.2439270019532));
#20972=CARTESIAN_POINT('Ctrl Pts',(-1.88698276339085,0.648777597626214,
31.2385900023989));
#20973=CARTESIAN_POINT('Ctrl Pts',(-1.86982248342857,0.69669179870545,31.2351926199528));
#20974=CARTESIAN_POINT('Ctrl Pts',(-1.81338337256306,0.837115439473,31.2249386276497));
#20975=CARTESIAN_POINT('Ctrl Pts',(-1.76892972803691,0.927364986613652,
31.217944942651));
#20976=CARTESIAN_POINT('Ctrl Pts',(-1.65588155766603,1.11890984876398,31.2024266984386));
#20977=CARTESIAN_POINT('Ctrl Pts',(-1.58437974691568,1.21805219834673,31.1939240981901));
#20978=CARTESIAN_POINT('Ctrl Pts',(-1.49928348244099,1.31576366149377,31.1854643857727));
#20979=CARTESIAN_POINT('Ctrl Pts',(-1.49427467463566,1.32144927062638,31.1849718807926));
#20980=CARTESIAN_POINT('Ctrl Pts',(-1.48690172279494,1.32972294602694,31.1842549959714));
#20981=CARTESIAN_POINT('Ctrl Pts',(-1.48456303651856,1.33233345582291,31.1840287760579));
#20982=CARTESIAN_POINT('Ctrl Pts',(-1.48040331528074,1.33695210651232,31.1836285070402));
#20983=CARTESIAN_POINT('Ctrl Pts',(-1.47858505458397,1.33896271333984,31.1834542515238));
#20984=CARTESIAN_POINT('Ctrl Pts',(-1.47473392016223,1.34320383212994,31.1830866693572));
#20985=CARTESIAN_POINT('Ctrl Pts',(-1.47270008725653,1.34543343321652,31.1828934178857));
#20986=CARTESIAN_POINT('Ctrl Pts',(-1.46723944392326,1.3513924774604,31.1823768619727));
#20987=CARTESIAN_POINT('Ctrl Pts',(-1.46380344807836,1.35511353055324,31.1820542483759));
#20988=CARTESIAN_POINT('Ctrl Pts',(-1.44729278073818,1.37285788253193,31.1805153151586));
#20989=CARTESIAN_POINT('Ctrl Pts',(-1.43403001288442,1.38670586166615,31.1793127854054));
#20990=CARTESIAN_POINT('Ctrl Pts',(-1.39649113896128,1.42478644227771,31.1759942359655));
#20991=CARTESIAN_POINT('Ctrl Pts',(-1.37178577288711,1.44858827409231,31.1739063592736));
#20992=CARTESIAN_POINT('Ctrl Pts',(-1.27943566401587,1.53307814529466,31.1663891734738));
#20993=CARTESIAN_POINT('Ctrl Pts',(-1.20827658467783,1.58976544085981,31.1611328268029));
#20994=CARTESIAN_POINT('Ctrl Pts',(-1.00427663326607,1.73064046305574,31.1467547390443));
#20995=CARTESIAN_POINT('Ctrl Pts',(-0.864994056850914,1.80429041889654,
31.1376118454133));
#20996=CARTESIAN_POINT('Ctrl Pts',(-0.706829202964467,1.86536250699166,
31.1270239583355));
#20997=CARTESIAN_POINT('Ctrl Pts',(-0.695089231941632,1.86976890359345,
31.1262372926929));
#20998=CARTESIAN_POINT('Ctrl Pts',(-0.677527660102893,1.87617208587096,
31.125059083945));
#20999=CARTESIAN_POINT('Ctrl Pts',(-0.671736945297046,1.87825315145487,
31.124670350614));
#21000=CARTESIAN_POINT('Ctrl Pts',(-0.661380479736466,1.88192103633594,
31.1239746613554));
#21001=CARTESIAN_POINT('Ctrl Pts',(-0.65681839603707,1.88351812307009,31.1236680492174));
#21002=CARTESIAN_POINT('Ctrl Pts',(-0.647169566926578,1.88685665105511,
31.1230192112892));
#21003=CARTESIAN_POINT('Ctrl Pts',(-0.642081502978429,1.88859413654348,
31.1226768573425));
#21004=CARTESIAN_POINT('Ctrl Pts',(-0.628562317584801,1.89314975662326,
31.1217666312155));
#21005=CARTESIAN_POINT('Ctrl Pts',(-0.620119350879211,1.89593211231607,
31.1211975837239));
#21006=CARTESIAN_POINT('Ctrl Pts',(-0.580702160949729,1.90863047499537,
31.118537907081));
#21007=CARTESIAN_POINT('Ctrl Pts',(-0.549508511316975,1.91784396608568,
31.1164244034177));
#21008=CARTESIAN_POINT('Ctrl Pts',(-0.464265799246307,1.9407712876464,31.1106214276322));
#21009=CARTESIAN_POINT('Ctrl Pts',(-0.409847701835213,1.95298741129955,
31.1068866598826));
#21010=CARTESIAN_POINT('Ctrl Pts',(-0.252367685644169,1.98146779719222,
31.0960014792073));
#21011=CARTESIAN_POINT('Ctrl Pts',(-0.148451425910998,1.99194955617663,
31.0887165774201));
#21012=CARTESIAN_POINT('Ctrl Pts',(0.032268284277143,1.99595513123105,31.0761123235167));
#21013=CARTESIAN_POINT('Ctrl Pts',(0.108778141130885,1.99325037343932,31.0707999761076));
#21014=CARTESIAN_POINT('Ctrl Pts',(0.220692408511845,1.98282907905133,31.0632120929522));
#21015=CARTESIAN_POINT('Ctrl Pts',(0.256343178529391,1.97853604150312,31.0608229424961));
#21016=CARTESIAN_POINT('Ctrl Pts',(0.297688003581043,1.97242087520728,31.0580994640606));
#21017=CARTESIAN_POINT('Ctrl Pts',(0.303511012869209,1.97153324182182,31.0577169879956));
#21018=CARTESIAN_POINT('Ctrl Pts',(0.312811317087408,1.97007336409897,31.0571079603871));
#21019=CARTESIAN_POINT('Ctrl Pts',(0.31629112000322,1.9695176840805,31.056880501021));
#21020=CARTESIAN_POINT('Ctrl Pts',(0.322447836978754,1.96851779718032,31.056478819528));
#21021=CARTESIAN_POINT('Ctrl Pts',(0.325125337342351,1.96807734623456,31.0563043859038));
#21022=CARTESIAN_POINT('Ctrl Pts',(0.330768766717762,1.96713716644237,31.0559372710552));
#21023=CARTESIAN_POINT('Ctrl Pts',(0.333734459130286,1.9666361940424,31.0557446617724));
#21024=CARTESIAN_POINT('Ctrl Pts',(0.341646190442853,1.96528131197251,31.0552316393335));
#21025=CARTESIAN_POINT('Ctrl Pts',(0.346590199238606,1.9644154320669,31.0549119006035));
#21026=CARTESIAN_POINT('Ctrl Pts',(0.369915499791155,1.96023950331184,31.0534071835543));
#21027=CARTESIAN_POINT('Ctrl Pts',(0.388253722277744,1.95668993340963,31.052235263747));
#21028=CARTESIAN_POINT('Ctrl Pts',(0.574894127910444,1.91783618901617,31.040396187309));
#21029=CARTESIAN_POINT('Ctrl Pts',(0.738034696196257,1.86116153261909,31.030735067415));
#21030=CARTESIAN_POINT('Ctrl Pts',(0.990544070261842,1.73493869467138,31.0142218044359));
#21031=CARTESIAN_POINT('Ctrl Pts',(1.0849157119771,1.67754062608221,31.0076452878914));
#21032=CARTESIAN_POINT('Ctrl Pts',(1.18449948506942,1.6050406427909,30.9999563093416));
#21033=CARTESIAN_POINT('Ctrl Pts',(1.19487045530749,1.59733499231193,30.9991460128382));
#21034=CARTESIAN_POINT('Ctrl Pts',(1.21012883259697,1.58576623898341,30.9979392738313));
#21035=CARTESIAN_POINT('Ctrl Pts',(1.21507432037646,1.58198000958115,30.9975458469874));
#21036=CARTESIAN_POINT('Ctrl Pts',(1.22383322617909,1.57520895366687,30.9968449037336));
#21037=CARTESIAN_POINT('Ctrl Pts',(1.22765367697921,1.57223327211136,30.9965377509617));
#21038=CARTESIAN_POINT('Ctrl Pts',(1.2356607821859,1.56594970033123,30.995890998397));
#21039=CARTESIAN_POINT('Ctrl Pts',(1.23984506976345,1.56263886892361,30.9955512827896));
#21040=CARTESIAN_POINT('Ctrl Pts',(1.25082172300252,1.55388171311349,30.9946554779236));
#21041=CARTESIAN_POINT('Ctrl Pts',(1.25759174484254,1.54840768546309,30.9940982788395));
#21042=CARTESIAN_POINT('Ctrl Pts',(1.28801830622811,1.52347454594009,30.9915725084775));
#21043=CARTESIAN_POINT('Ctrl Pts',(1.31125946526838,1.50351730634742,30.9895837740622));
#21044=CARTESIAN_POINT('Ctrl Pts',(1.37217644151777,1.44872076027496,30.9842056921162));
#21045=CARTESIAN_POINT('Ctrl Pts',(1.408980924493,1.41295152995392,30.9807787636526));
#21046=CARTESIAN_POINT('Ctrl Pts',(1.51389366465317,1.30281091363879,30.9704690127331));
#21047=CARTESIAN_POINT('Ctrl Pts',(1.5777848604126,1.22465584098359,30.9634492639706));
#21048=CARTESIAN_POINT('Ctrl Pts',(1.68418416071839,1.07228040907223,30.9504827827202));
#21049=CARTESIAN_POINT('Ctrl Pts',(1.72837114410311,0.999498183239119,30.9445554114429));
#21050=CARTESIAN_POINT('Ctrl Pts',(1.78509501797916,0.890988459725063,30.9362791772635));
#21051=CARTESIAN_POINT('Ctrl Pts',(1.80147806444191,0.857380828877979,30.9337891843463));
#21052=CARTESIAN_POINT('Ctrl Pts',(1.81936909496831,0.817899265772309,30.930964167749));
#21053=CARTESIAN_POINT('Ctrl Pts',(1.82180574160099,0.812457355640775,30.9305769553645));
#21054=CARTESIAN_POINT('Ctrl Pts',(1.82565217337184,0.803762571578491,30.9299618398451));
#21055=CARTESIAN_POINT('Ctrl Pts',(1.82707772717558,0.800516776178691,30.9297330005675));
#21056=CARTESIAN_POINT('Ctrl Pts',(1.82958038317483,0.794777052715037,30.9293297395611));
#21057=CARTESIAN_POINT('Ctrl Pts',(1.83066105254867,0.792284704548647,30.9291551006747));
#21058=CARTESIAN_POINT('Ctrl Pts',(1.83292316594254,0.78703825245408,30.9287884733284));
#21059=CARTESIAN_POINT('Ctrl Pts',(1.83410349336,0.784283698039193,30.9285965532947));
#21060=CARTESIAN_POINT('Ctrl Pts',(1.83722494496853,0.776953517322683,30.9280873220005));
#21061=CARTESIAN_POINT('Ctrl Pts',(1.83915519845539,0.772373241231321,30.9277706677287));
#21062=CARTESIAN_POINT('Ctrl Pts',(1.84805774962005,0.751025872773029,30.9263017705579));
#21063=CARTESIAN_POINT('Ctrl Pts',(1.85481827948457,0.73417062994929,30.9251618433078));
#21064=CARTESIAN_POINT('Ctrl Pts',(1.91739337045346,0.57177519373274,30.9143467231604));
#21065=CARTESIAN_POINT('Ctrl Pts',(1.95620574354421,0.420235728504764,30.9055066279835));
#21066=CARTESIAN_POINT('Ctrl Pts',(1.99386810558418,0.140008305319292,30.8890469952164));
#21067=CARTESIAN_POINT('Ctrl Pts',(1.9987336623906,0.0130076470548837,30.8815461973256));
#21068=CARTESIAN_POINT('Ctrl Pts',(1.99077283241317,-0.126571232251853,
30.8728202581421));
#21069=CARTESIAN_POINT('Ctrl Pts',(1.9899051972352,-0.139549419073874,30.8720045704407));
#21070=CARTESIAN_POINT('Ctrl Pts',(1.98843319239388,-0.158745101669556,
30.8707913317783));
#21071=CARTESIAN_POINT('Ctrl Pts',(1.98792643058039,-0.164969915671555,
30.8703968444273));
#21072=CARTESIAN_POINT('Ctrl Pts',(1.98697466582404,-0.176019065659548,
30.8696947062967));
#21073=CARTESIAN_POINT('Ctrl Pts',(1.98654130222136,-0.180844375064161,
30.8693874236488));
#21074=CARTESIAN_POINT('Ctrl Pts',(1.98559454126165,-0.190971874618354,
30.8687411047432));
#21075=CARTESIAN_POINT('Ctrl Pts',(1.98507747519386,-0.196273675651231,
30.8684019553599));
#21076=CARTESIAN_POINT('Ctrl Pts',(1.98366337838926,-0.210195809776485,
30.8675092456928));
#21077=CARTESIAN_POINT('Ctrl Pts',(1.98273140001984,-0.218812405163402,
30.8669545894451));
#21078=CARTESIAN_POINT('Ctrl Pts',(1.97829564619371,-0.257465237872614,
30.8644566319803));
#21079=CARTESIAN_POINT('Ctrl Pts',(1.97416543968721,-0.287424185108046,
30.8624937078472));
#21080=CARTESIAN_POINT('Ctrl Pts',(1.9613384907093,-0.367041932504719,30.8572021400294));
#21081=CARTESIAN_POINT('Ctrl Pts',(1.95143808899274,-0.416481837387152,
30.8538373863261));
#21082=CARTESIAN_POINT('Ctrl Pts',(1.91632034008428,-0.562815839647878,
30.8436451402717));
#21083=CARTESIAN_POINT('Ctrl Pts',(1.88567379545211,-0.658237294143165,
30.836680429423));
#21084=CARTESIAN_POINT('Ctrl Pts',(1.80165789901835,-0.864991354912337,
30.8211092979026));
#21085=CARTESIAN_POINT('Ctrl Pts',(1.74485211177816,-0.9745151567217,30.8125231318297));
#21086=CARTESIAN_POINT('Ctrl Pts',(1.6742202599273,-1.08446814209581,30.8039911124005));
#21087=CARTESIAN_POINT('Ctrl Pts',(1.67010119751613,-1.09080090963307,30.8035000978645));
#21088=CARTESIAN_POINT('Ctrl Pts',(1.6640208755196,-1.10003379141174,30.8027849704285));
#21089=CARTESIAN_POINT('Ctrl Pts',(1.66208786158366,-1.10295229146523,30.802559030048));
#21090=CARTESIAN_POINT('Ctrl Pts',(1.65864463900939,-1.10812132427727,30.8021590787325));
#21091=CARTESIAN_POINT('Ctrl Pts',(1.65713751623782,-1.1103738831854,30.8019848625321));
#21092=CARTESIAN_POINT('Ctrl Pts',(1.65394118904495,-1.11513013915709,30.8016171709741));
#21093=CARTESIAN_POINT('Ctrl Pts',(1.65225089273359,-1.1176330667237,30.8014237715359));
#21094=CARTESIAN_POINT('Ctrl Pts',(1.64770496279773,-1.12433165746063,30.8009064012472));
#21095=CARTESIAN_POINT('Ctrl Pts',(1.64483896661605,-1.12852031247112,30.8005831250485));
#21096=CARTESIAN_POINT('Ctrl Pts',(1.63100394090725,-1.1485755400944,30.7990361888016));
#21097=CARTESIAN_POINT('Ctrl Pts',(1.61982068588802,-1.16429405182188,30.7978264927564));
#21098=CARTESIAN_POINT('Ctrl Pts',(1.58795084166033,-1.20774013418534,30.7944830396632));
#21099=CARTESIAN_POINT('Ctrl Pts',(1.56676767591454,-1.23509653497835,30.7923779404633));
#21100=CARTESIAN_POINT('Ctrl Pts',(1.48682514277101,-1.33296706467308,30.7847911657475));
#21101=CARTESIAN_POINT('Ctrl Pts',(1.42392781617646,-1.39995787477465,30.77948505607));
#21102=CARTESIAN_POINT('Ctrl Pts',(1.24254851037312,-1.56822154143298,30.7651359416259));
#21103=CARTESIAN_POINT('Ctrl Pts',(1.11648618569916,-1.66032976765912,30.7560686331889));
#21104=CARTESIAN_POINT('Ctrl Pts',(0.970052269822594,-1.7430388865462,30.7455667809738));
#21105=CARTESIAN_POINT('Ctrl Pts',(0.959035509866836,-1.74912459403028,
30.7447772446136));
#21106=CARTESIAN_POINT('Ctrl Pts',(0.942539923947373,-1.75803413816186,
30.7435955664146));
#21107=CARTESIAN_POINT('Ctrl Pts',(0.937104260467197,-1.76093757493176,
30.7432062589891));
#21108=CARTESIAN_POINT('Ctrl Pts',(0.927493176188584,-1.76601419214855,
30.7425180091939));
#21109=CARTESIAN_POINT('Ctrl Pts',(0.923323334104867,-1.76819787886469,
30.7422194415545));
#21110=CARTESIAN_POINT('Ctrl Pts',(0.914513090343158,-1.77277201511575,
30.7415886675316));
#21111=CARTESIAN_POINT('Ctrl Pts',(0.909870963007115,-1.77515904634179,
30.7412563434684));
#21112=CARTESIAN_POINT('Ctrl Pts',(0.900362678696656,-1.78000121243852,
30.7405756982464));
#21113=CARTESIAN_POINT('Ctrl Pts',(0.895495724887295,-1.78245467690037,
30.7402273218416));
#21114=CARTESIAN_POINT('Ctrl Pts',(0.883475391576953,-1.78845255136964,
30.7393669311408));
#21115=CARTESIAN_POINT('Ctrl Pts',(0.876310720792331,-1.79197399913212,
30.7388541197062));
#21116=CARTESIAN_POINT('Ctrl Pts',(0.856413061815055,-1.80160586549991,
30.737429912066));
#21117=CARTESIAN_POINT('Ctrl Pts',(0.843636220407204,-1.80762411402532,
30.73651534913));
#21118=CARTESIAN_POINT('Ctrl Pts',(0.727691293483214,-1.86074038350987,
30.7282144376432));
#21119=CARTESIAN_POINT('Ctrl Pts',(0.620763014543473,-1.89908792487588,
30.7205294409812));
#21120=CARTESIAN_POINT('Ctrl Pts',(0.378262314537477,-1.96337770096241,
30.7031559857211));
#21121=CARTESIAN_POINT('Ctrl Pts',(0.24206481084392,-1.98477715771986,30.6934277198737));
#21122=CARTESIAN_POINT('Ctrl Pts',(0.0689977362471238,-1.99387774352911,
30.6817290272623));
#21123=CARTESIAN_POINT('Ctrl Pts',(0.0332009877801101,-1.99479503505999,
30.6793466729204));
#21124=CARTESIAN_POINT('Ctrl Pts',(-0.00848886137459782,-1.99474061907471,
30.6766300481064));
#21125=CARTESIAN_POINT('Ctrl Pts',(-0.0143740897827916,-1.99470689220335,
30.6762478964795));
#21126=CARTESIAN_POINT('Ctrl Pts',(-0.0237813886347323,-1.99461134443465,
30.6756392861305));
#21127=CARTESIAN_POINT('Ctrl Pts',(-0.0273035380444403,-1.99456624033171,
30.6754119215116));
#21128=CARTESIAN_POINT('Ctrl Pts',(-0.0335385166585083,-1.99446987747866,
30.6750103482055));
#21129=CARTESIAN_POINT('Ctrl Pts',(-0.0362513810617108,-1.99442241313016,
30.6748359284097));
#21130=CARTESIAN_POINT('Ctrl Pts',(-0.0419720574307192,-1.99431064772598,
30.6744687788403));
#21131=CARTESIAN_POINT('Ctrl Pts',(-0.044979815531504,-1.99424507764888,
30.6742761212528));
#21132=CARTESIAN_POINT('Ctrl Pts',(-0.0530085863773872,-1.99405187465097,
30.6737628330784));
#21133=CARTESIAN_POINT('Ctrl Pts',(-0.0580293260474644,-1.99391208122831,
30.6734428781467));
#21134=CARTESIAN_POINT('Ctrl Pts',(-0.0817539013258678,-1.99316182603325,
30.6719356161514));
#21135=CARTESIAN_POINT('Ctrl Pts',(-0.100449825557757,-1.99230711966565,
30.6707614212645));
#21136=CARTESIAN_POINT('Ctrl Pts',(-0.290777119355789,-1.98091994285634,
30.6589213061435));
#21137=CARTESIAN_POINT('Ctrl Pts',(-0.460399861992667,-1.94849830957342,
30.6492608441593));
#21138=CARTESIAN_POINT('Ctrl Pts',(-0.728479717704918,-1.86024060531193,
30.632751225846));
#21139=CARTESIAN_POINT('Ctrl Pts',(-0.830127548660997,-1.81715736612486,
30.6261778860915));
#21140=CARTESIAN_POINT('Ctrl Pts',(-0.939139613169537,-1.75988966870218,
30.6184915545002));
#21141=CARTESIAN_POINT('Ctrl Pts',(-0.95053105845854,-1.75376325465686,
30.6176803843634));
#21142=CARTESIAN_POINT('Ctrl Pts',(-0.9673208429311,-1.74452193375066,30.6164725918652));
#21143=CARTESIAN_POINT('Ctrl Pts',(-0.972765617208123,-1.74149172925181,
30.6160789929091));
#21144=CARTESIAN_POINT('Ctrl Pts',(-0.982303783523599,-1.73612472340922,
30.6153860594975));
#21145=CARTESIAN_POINT('Ctrl Pts',(-0.986403278291313,-1.73379882059854,
30.6150871184092));
#21146=CARTESIAN_POINT('Ctrl Pts',(-0.99499212705771,-1.72888550185399,
30.6144584342802));
#21147=CARTESIAN_POINT('Ctrl Pts',(-0.999479713997759,-1.72629508251038,
30.614128584336));
#21148=CARTESIAN_POINT('Ctrl Pts',(-1.00862206488894,-1.72097014411957,
30.6134537725302));
#21149=CARTESIAN_POINT('Ctrl Pts',(-1.01327591955092,-1.71823415652256,
30.6131087592285));
#21150=CARTESIAN_POINT('Ctrl Pts',(-1.024676310235,-1.71146947612557,30.6122598599228));
#21151=CARTESIAN_POINT('Ctrl Pts',(-1.03141021294671,-1.70741977209982,
30.6117552101457));
#21152=CARTESIAN_POINT('Ctrl Pts',(-1.04991210181841,-1.69614352220084,
30.6103596302375));
#21153=CARTESIAN_POINT('Ctrl Pts',(-1.06162906584482,-1.68883450345156,
30.6094656904831));
#21154=CARTESIAN_POINT('Ctrl Pts',(-1.09871067489991,-1.66516468560231,
30.6066036430285));
#21155=CARTESIAN_POINT('Ctrl Pts',(-1.12377931177294,-1.648350227588,30.6046190089808));
#21156=CARTESIAN_POINT('Ctrl Pts',(-1.22435195382162,-1.57753167824948,
30.5964487928782));
#21157=CARTESIAN_POINT('Ctrl Pts',(-1.29641617636026,-1.51886314082391,
30.5900965347656));
#21158=CARTESIAN_POINT('Ctrl Pts',(-1.47601651483654,-1.35052590813613,
30.5730074456338));
#21159=CARTESIAN_POINT('Ctrl Pts',(-1.57544416212508,-1.23309622233248,
30.5621420012456));
#21160=CARTESIAN_POINT('Ctrl Pts',(-1.66832844720924,-1.09357691558635,
30.5510836096127));
#21161=CARTESIAN_POINT('Ctrl Pts',(-1.67609176887542,-1.08164073916261,
30.5501513403544));
#21162=CARTESIAN_POINT('Ctrl Pts',(-1.68625943840324,-1.06563547965153,
30.5489205786209));
#21163=CARTESIAN_POINT('Ctrl Pts',(-1.68877785640327,-1.06163987393523,
30.5486149127207));
#21164=CARTESIAN_POINT('Ctrl Pts',(-1.69268628263736,-1.05538984500868,
30.5481392979288));
#21165=CARTESIAN_POINT('Ctrl Pts',(-1.69408601153855,-1.05314156792276,
30.5479687141645));
#21166=CARTESIAN_POINT('Ctrl Pts',(-1.69676457817262,-1.04882003339374,
30.5476418056303));
#21167=CARTESIAN_POINT('Ctrl Pts',(-1.6980440809281,-1.04674724527474,30.5474854392649));
#21168=CARTESIAN_POINT('Ctrl Pts',(-1.70109479113365,-1.04178479595711,
30.547112109566));
#21169=CARTESIAN_POINT('Ctrl Pts',(-1.70286243200226,-1.0388929625332,30.5468953825897));
#21170=CARTESIAN_POINT('Ctrl Pts',(-1.70815290045356,-1.03018805697164,
30.546245439563));
#21171=CARTESIAN_POINT('Ctrl Pts',(-1.71165344012901,-1.02436139529044,
30.5458136600655));
#21172=CARTESIAN_POINT('Ctrl Pts',(-1.74429482901721,-0.969395161345221,
30.5417699113467));
#21173=CARTESIAN_POINT('Ctrl Pts',(-1.77134493247479,-0.919037520493393,
30.5382857105938));
#21174=CARTESIAN_POINT('Ctrl Pts',(-1.89070397722454,-0.67192278166108,
30.5218885323362));
#21175=CARTESIAN_POINT('Ctrl Pts',(-1.9526085886087,-0.462140684089348,
30.5098589377122));
#21176=CARTESIAN_POINT('Ctrl Pts',(-1.98309007347306,-0.217355163286339,
30.4947211034775));
#21177=CARTESIAN_POINT('Ctrl Pts',(-1.9860741285533,-0.188146013438282,
30.492901088329));
#21178=CARTESIAN_POINT('Ctrl Pts',(-1.98916000561039,-0.149526372181063,
30.4904724526059));
#21179=CARTESIAN_POINT('Ctrl Pts',(-1.98984156439777,-0.140164930181504,
30.4898820354191));
#21180=CARTESIAN_POINT('Ctrl Pts',(-1.99082037799331,-0.12526967788181,
30.488939749249));
#21181=CARTESIAN_POINT('Ctrl Pts',(-1.99116069125404,-0.119738758240396,
30.4885892329797));
#21182=CARTESIAN_POINT('Ctrl Pts',(-1.9917525402028,-0.109418384663465,
30.4879339941431));
#21183=CARTESIAN_POINT('Ctrl Pts',(-1.99200985814323,-0.104629291822345,
30.4876294553304));
#21184=CARTESIAN_POINT('Ctrl Pts',(-1.99248084347473,-0.095230988806741,
30.4870308563351));
#21185=CARTESIAN_POINT('Ctrl Pts',(-1.99269579434065,-0.0906218708114643,
30.4867368384174));
#21186=CARTESIAN_POINT('Ctrl Pts',(-1.99314311831427,-0.0802574011244163,
30.4860746484356));
#21187=CARTESIAN_POINT('Ctrl Pts',(-1.99336655748497,-0.0745017239083139,
30.4857061984316));
#21188=CARTESIAN_POINT('Ctrl Pts',(-1.9939167460376,-0.0585466240891084,
30.4846828054902));
#21189=CARTESIAN_POINT('Ctrl Pts',(-1.99419015864603,-0.0483456517303464,
30.4840261989168));
#21190=CARTESIAN_POINT('Ctrl Pts',(-1.99463292928769,-0.0251945900154945,
30.482530679838));
#21191=CARTESIAN_POINT('Ctrl Pts',(-1.99475445956689,-0.0122441981611814,
30.4816903058683));
#21192=CARTESIAN_POINT('Ctrl Pts',(-1.99474987500568,0.00070616204988155,
30.4808460358741));
#21193=CARTESIAN_POINT('',(-1.99474947325114,-0.00144964281222297,28.8790451185423));
#21194=CARTESIAN_POINT('Ctrl Pts',(-1.99474987552217,0.000704701547650649,
30.4808461310883));
#21195=CARTESIAN_POINT('Ctrl Pts',(-1.99466568051133,0.239029688859807,
30.4653090678252));
#21196=CARTESIAN_POINT('Ctrl Pts',(-1.95186213000554,0.475413415424764,
30.4482388704665));
#21197=CARTESIAN_POINT('Ctrl Pts',(-1.85744162136749,0.727958154770136,
30.4298945696681));
#21198=CARTESIAN_POINT('Ctrl Pts',(-1.84575844615724,0.757092096227795,
30.4277820813544));
#21199=CARTESIAN_POINT('Ctrl Pts',(-1.82630218246401,0.802478468634954,
30.4245098135911));
#21200=CARTESIAN_POINT('Ctrl Pts',(-1.8189886130018,0.818921141463728,30.4233282834959));
#21201=CARTESIAN_POINT('Ctrl Pts',(-1.80937863218933,0.839762510989474,
30.4218378076276));
#21202=CARTESIAN_POINT('Ctrl Pts',(-1.80728725145465,0.844254050328181,
30.4215170209616));
#21203=CARTESIAN_POINT('Ctrl Pts',(-1.80390555593749,0.851446573282073,
30.4210040706918));
#21204=CARTESIAN_POINT('Ctrl Pts',(-1.8026258754975,0.854152489414659,30.4208112613892));
#21205=CARTESIAN_POINT('Ctrl Pts',(-1.80017273746489,0.859309643353357,
30.42044412703));
#21206=CARTESIAN_POINT('Ctrl Pts',(-1.79900037577071,0.861761333506452,
30.4202697405456));
#21207=CARTESIAN_POINT('Ctrl Pts',(-1.79628409260997,0.867412034805799,
30.4198681396871));
#21208=CARTESIAN_POINT('Ctrl Pts',(-1.79473663470469,0.870609322265508,
30.4196411476917));
#21209=CARTESIAN_POINT('Ctrl Pts',(-1.79055825375805,0.879184019487755,
30.4190329917603));
#21210=CARTESIAN_POINT('Ctrl Pts',(-1.78791162481773,0.884553799526985,
30.4186527849619));
#21211=CARTESIAN_POINT('Ctrl Pts',(-1.76834119322049,0.92381380110481,30.4158771060142));
#21212=CARTESIAN_POINT('Ctrl Pts',(-1.75047792899269,0.957230372849213,
30.4135371024245));
#21213=CARTESIAN_POINT('Ctrl Pts',(-1.68968699356754,1.06355075706345,30.4061000826566));
#21214=CARTESIAN_POINT('Ctrl Pts',(-1.64306980890241,1.13424263085786,30.4011655783765));
#21215=CARTESIAN_POINT('Ctrl Pts',(-1.49632628831981,1.32864867189428,30.3870218590609));
#21216=CARTESIAN_POINT('Ctrl Pts',(-1.38574046017786,1.44361234050747,30.3778726511871));
#21217=CARTESIAN_POINT('Ctrl Pts',(-1.24979288024212,1.55477419618601,30.3670421843246));
#21218=CARTESIAN_POINT('Ctrl Pts',(-1.236766032734,1.56515647753784,30.3660087802714));
#21219=CARTESIAN_POINT('Ctrl Pts',(-1.21651986280806,1.58088190739906,30.3644084793133));
#21220=CARTESIAN_POINT('Ctrl Pts',(-1.20939173367485,1.58634164418815,30.3638461432804));
#21221=CARTESIAN_POINT('Ctrl Pts',(-1.19754619333474,1.59528840247737,30.3629133082341));
#21222=CARTESIAN_POINT('Ctrl Pts',(-1.19284977722775,1.59880310858834,30.3625438915353));
#21223=CARTESIAN_POINT('Ctrl Pts',(-1.18370561852511,1.60558370045337,30.3618254027196));
#21224=CARTESIAN_POINT('Ctrl Pts',(-1.17925968858737,1.60885194979654,30.3614764266885));
#21225=CARTESIAN_POINT('Ctrl Pts',(-1.17477665416828,1.61211890882029,30.3611248798015));
#21226=CARTESIAN_POINT('Ctrl Pts',(-1.17475301654721,1.61213613366491,30.3611230262156));
#21227=CARTESIAN_POINT('Ctrl Pts',(-1.17470501832466,1.61217110857708,30.3611192623693));
#21228=CARTESIAN_POINT('Ctrl Pts',(-1.17468065827152,1.6121888581958,30.3611173521525));
#21229=CARTESIAN_POINT('Ctrl Pts',(-1.17463118657791,1.6122249033504,30.3611134728031));
#21230=CARTESIAN_POINT('Ctrl Pts',(-1.17460607548248,1.61224319843639,30.3611115037137));
#21231=CARTESIAN_POINT('Ctrl Pts',(-1.17455507163147,1.61228035627505,30.3611075042629));
#21232=CARTESIAN_POINT('Ctrl Pts',(-1.1745291793961,1.61229921859214,30.3611054739429));
#21233=CARTESIAN_POINT('Ctrl Pts',(-1.17447658165263,1.61233753375047,30.3611013495539));
#21234=CARTESIAN_POINT('Ctrl Pts',(-1.17444987661594,1.61235698618758,30.3610992555226));
#21235=CARTESIAN_POINT('Ctrl Pts',(-1.17439561991206,1.6123965056997,30.3610950010975));
#21236=CARTESIAN_POINT('Ctrl Pts',(-1.17436806870536,1.61241657237407,30.3610928407406));
#21237=CARTESIAN_POINT('Ctrl Pts',(-1.17431208451571,1.61245734576052,30.3610884509108));
#21238=CARTESIAN_POINT('Ctrl Pts',(-1.17428365196805,1.61247805208547,30.3610862214729));
#21239=CARTESIAN_POINT('Ctrl Pts',(-1.1742258680442,1.61252013154369,30.3610816905783));
#21240=CARTESIAN_POINT('Ctrl Pts',(-1.17419651706862,1.61254150430984,30.3610793891539));
#21241=CARTESIAN_POINT('Ctrl Pts',(-1.17413685713103,1.6125849449352,30.3610747112187));
#21242=CARTESIAN_POINT('Ctrl Pts',(-1.17410654855901,1.61260701242928,30.3610723347395));
#21243=CARTESIAN_POINT('Ctrl Pts',(-1.17404493213218,1.61265187233141,30.3610675034594));
#21244=CARTESIAN_POINT('Ctrl Pts',(-1.17401362461838,1.61267466440375,30.3610650486865));
#21245=CARTESIAN_POINT('Ctrl Pts',(-1.1739499665713,1.61272100503713,30.3610600573928));
#21246=CARTESIAN_POINT('Ctrl Pts',(-1.17391761637694,1.61274455325718,30.3610575208998));
#21247=CARTESIAN_POINT('Ctrl Pts',(-1.17385182676162,1.61279243953418,30.3610523625466));
#21248=CARTESIAN_POINT('Ctrl Pts',(-1.1738183876307,1.61281677727829,30.3610497407103));
#21249=CARTESIAN_POINT('Ctrl Pts',(-1.17375037124547,1.6128662778822,30.3610444078403));
#21250=CARTESIAN_POINT('Ctrl Pts',(-1.17371579423155,1.61289144045715,30.3610416968268));
#21251=CARTESIAN_POINT('Ctrl Pts',(-1.17364545012493,1.61294262819773,30.3610361815328));
#21252=CARTESIAN_POINT('Ctrl Pts',(-1.17360968330331,1.61296865304726,30.361033377275));
#21253=CARTESIAN_POINT('Ctrl Pts',(-1.17353690462833,1.61302160496073,30.3610276711881));
#21254=CARTESIAN_POINT('Ctrl Pts',(-1.1734998929798,1.613048531747,30.3610247693767));
#21255=CARTESIAN_POINT('Ctrl Pts',(-1.17342456627785,1.61310332961044,30.3610188636106));
#21256=CARTESIAN_POINT('Ctrl Pts',(-1.17338625139744,1.61313120042238,30.3610158596712));
#21257=CARTESIAN_POINT('Ctrl Pts',(-1.17330825620532,1.61318793103211,30.3610097447912));
#21258=CARTESIAN_POINT('Ctrl Pts',(-1.17326857604437,1.61321679056911,30.3610066338643));
#21259=CARTESIAN_POINT('Ctrl Pts',(-1.17318778435371,1.61327554612565,30.3610002998454));
#21260=CARTESIAN_POINT('Ctrl Pts',(-1.17314667294667,1.61330544189189,30.3609970767649));
#21261=CARTESIAN_POINT('Ctrl Pts',(-1.17306294856002,1.61336632045898,30.3609905129408));
#21262=CARTESIAN_POINT('Ctrl Pts',(-1.17302033568964,1.61339730300204,30.3609871722079));
#21263=CARTESIAN_POINT('Ctrl Pts',(-1.17293353364606,1.61346040891404,30.3609803672267));
#21264=CARTESIAN_POINT('Ctrl Pts',(-1.17288934453556,1.61349253204329,30.3609769029857));
#21265=CARTESIAN_POINT('Ctrl Pts',(-1.17279931030378,1.61355797648023,30.3609698447465));
#21266=CARTESIAN_POINT('Ctrl Pts',(-1.17275346521908,1.61359129754987,30.3609662507537));
#21267=CARTESIAN_POINT('Ctrl Pts',(-1.17266003397574,1.61365919904923,30.3609589263502));
#21268=CARTESIAN_POINT('Ctrl Pts',(-1.17261244783259,1.61369377923703,30.3609551959434));
#21269=CARTESIAN_POINT('Ctrl Pts',(-1.17251914935189,1.61376157163806,30.3609478820975));
#21270=CARTESIAN_POINT('Ctrl Pts',(-1.17247343729051,1.61379478389938,30.360944298677));
#21271=CARTESIAN_POINT('Ctrl Pts',(-1.16859673567131,1.61661116363172,30.3606404026141));
#21272=CARTESIAN_POINT('Ctrl Pts',(-1.16475587701931,1.61938066288131,30.3603395636112));
#21273=CARTESIAN_POINT('Ctrl Pts',(-1.15583163972442,1.6257674213605,30.3596411150445));
#21274=CARTESIAN_POINT('Ctrl Pts',(-1.15074110011931,1.62937454465798,30.359243119517));
#21275=CARTESIAN_POINT('Ctrl Pts',(-1.13501272429323,1.64040909782194,30.3580146282341));
#21276=CARTESIAN_POINT('Ctrl Pts',(-1.12431944900311,1.64775655237485,30.3571810976589));
#21277=CARTESIAN_POINT('Ctrl Pts',(-1.01789323044253,1.7193647499095,30.34890045313));
#21278=CARTESIAN_POINT('Ctrl Pts',(-0.91684810955211,1.77530359854768,30.341139356087));
#21279=CARTESIAN_POINT('Ctrl Pts',(-0.66521501300496,1.88737377633127,30.3221230288653));
#21280=CARTESIAN_POINT('Ctrl Pts',(-0.511559342251409,1.93468320884565,
30.3107290315539));
#21281=CARTESIAN_POINT('Ctrl Pts',(-0.329817526449159,1.96744675655863,
30.2984025546668));
#21282=CARTESIAN_POINT('Ctrl Pts',(-0.305656538455194,1.97134485983718,
30.2967878261163));
#21283=CARTESIAN_POINT('Ctrl Pts',(-0.275996518025113,1.97557171257568,
30.2948397746447));
#21284=CARTESIAN_POINT('Ctrl Pts',(-0.270561168326607,1.9763234364378,30.2944841850787));
#21285=CARTESIAN_POINT('Ctrl Pts',(-0.2620387437074,1.97746629330736,30.2939289010564));
#21286=CARTESIAN_POINT('Ctrl Pts',(-0.258953789495453,1.97787263988403,
30.293728363844));
#21287=CARTESIAN_POINT('Ctrl Pts',(-0.253196166089922,1.97861732565822,
30.2933549732022));
#21288=CARTESIAN_POINT('Ctrl Pts',(-0.25052379089714,1.97895746549567,30.2931820222134));
#21289=CARTESIAN_POINT('Ctrl Pts',(-0.244466599660409,1.97971595835107,
30.2927908129422));
#21290=CARTESIAN_POINT('Ctrl Pts',(-0.241081403439257,1.98013104400671,
30.2925727411421));
#21291=CARTESIAN_POINT('Ctrl Pts',(-0.231062947396517,1.98133341369536,
30.2919289842313));
#21292=CARTESIAN_POINT('Ctrl Pts',(-0.224426696722137,1.98209607303317,
30.291504663611));
#21293=CARTESIAN_POINT('Ctrl Pts',(-0.1777111085203,1.98722715034128,30.288531692265));
#21294=CARTESIAN_POINT('Ctrl Pts',(-0.137507988255322,1.99041329263624,
30.2860456553246));
#21295=CARTESIAN_POINT('Ctrl Pts',(-0.0563548842666095,1.99437375319577,
30.2811235913442));
#21296=CARTESIAN_POINT('Ctrl Pts',(-0.0154231428127811,1.99511027609926,
30.2786900443058));
#21297=CARTESIAN_POINT('Ctrl Pts',(0.0696939432603636,1.99402190705517,
30.2736801147433));
#21298=CARTESIAN_POINT('Ctrl Pts',(0.113853778871762,1.99198848396273,30.2711091737496));
#21299=CARTESIAN_POINT('Ctrl Pts',(0.200626784587728,1.98509763953635,30.2660566993938));
#21300=CARTESIAN_POINT('Ctrl Pts',(0.243222513348809,1.98032990487091,30.2635761672926));
#21301=CARTESIAN_POINT('Ctrl Pts',(0.401846263907804,1.95737982017132,30.2542512439538));
#21302=CARTESIAN_POINT('Ctrl Pts',(0.516333895195177,1.93033941821418,30.2473275949846));
#21303=CARTESIAN_POINT('Ctrl Pts',(0.641414689460609,1.88886774831417,30.2391736180503));
#21304=CARTESIAN_POINT('Ctrl Pts',(0.655008731771161,1.88419683660323,30.2382796204874));
#21305=CARTESIAN_POINT('Ctrl Pts',(0.676166651754766,1.87667033913496,30.2368753883034));
#21306=CARTESIAN_POINT('Ctrl Pts',(0.683765837338168,1.87391493386405,30.2363684362566));
#21307=CARTESIAN_POINT('Ctrl Pts',(0.696499459218093,1.86921005413598,30.2355144867702));
#21308=CARTESIAN_POINT('Ctrl Pts',(0.701643016338607,1.8672854093101,30.2351683146824));
#21309=CARTESIAN_POINT('Ctrl Pts',(0.711690686803729,1.86347833965617,30.2344896399933));
#21310=CARTESIAN_POINT('Ctrl Pts',(0.716595444989848,1.86159773404717,30.2341572003642));
#21311=CARTESIAN_POINT('Ctrl Pts',(0.72150063993698,1.85969470320895,30.233823568999));
#21312=CARTESIAN_POINT('Ctrl Pts',(0.721508600135357,1.85969161489308,30.2338230275757));
#21313=CARTESIAN_POINT('Ctrl Pts',(0.721524537637443,1.85968543150725,30.2338219435594));
#21314=CARTESIAN_POINT('Ctrl Pts',(0.721532514982225,1.8596823364211,30.2338214009637));
#21315=CARTESIAN_POINT('Ctrl Pts',(0.721548487002828,1.85967613940639,30.2338203145873));
#21316=CARTESIAN_POINT('Ctrl Pts',(0.721556481614404,1.8596730375025,30.233819770811));
#21317=CARTESIAN_POINT('Ctrl Pts',(0.721572488237506,1.85966682682479,30.2338186820686));
#21318=CARTESIAN_POINT('Ctrl Pts',(0.721580500204912,1.85966371806784,30.2338181371056));
#21319=CARTESIAN_POINT('Ctrl Pts',(0.721596541552215,1.85965749367835,30.2338170459889));
#21320=CARTESIAN_POINT('Ctrl Pts',(0.721604570938548,1.85965437804307,30.2338164998348));
#21321=CARTESIAN_POINT('Ctrl Pts',(0.72162064720136,1.85964813986603,30.2338154063306));
#21322=CARTESIAN_POINT('Ctrl Pts',(0.721628694086015,1.85964501732084,30.23381485898));
#21323=CARTESIAN_POINT('Ctrl Pts',(0.721644805413988,1.85963876529659,30.2338137630782));
#21324=CARTESIAN_POINT('Ctrl Pts',(0.721652869866033,1.85963563581389,30.2338132145264));
#21325=CARTESIAN_POINT('Ctrl Pts',(0.721669016452481,1.85962936986585,30.2338121162136));
#21326=CARTESIAN_POINT('Ctrl Pts',(0.721677098562723,1.85962623340962,30.2338115664543));
#21327=CARTESIAN_POINT('Ctrl Pts',(0.726093489696471,1.8579123140468,30.2335111540689));
#21328=CARTESIAN_POINT('Ctrl Pts',(0.730495670037904,1.85618587374475,30.2332107665123));
#21329=CARTESIAN_POINT('Ctrl Pts',(0.740619760255113,1.85217383023168,30.2325177457645));
#21330=CARTESIAN_POINT('Ctrl Pts',(0.74633727925959,1.84987734481367,30.2321247477341));
#21331=CARTESIAN_POINT('Ctrl Pts',(0.763696412171434,1.84281133809574,30.2309265669909));
#21332=CARTESIAN_POINT('Ctrl Pts',(0.775303449601213,1.83795821137453,30.2301185625849));
#21333=CARTESIAN_POINT('Ctrl Pts',(0.930030426104529,1.77153742094551,30.219253746891));
#21334=CARTESIAN_POINT('Ctrl Pts',(1.0654731073403,1.69353140090503,30.2085992605668));
#21335=CARTESIAN_POINT('Ctrl Pts',(1.26397311294647,1.54589729249184,30.1913569259095));
#21336=CARTESIAN_POINT('Ctrl Pts',(1.33365559086546,1.4862000157858,30.1849354583402));
#21337=CARTESIAN_POINT('Ctrl Pts',(1.42363398434183,1.39767278890527,30.1763208342768));
#21338=CARTESIAN_POINT('Ctrl Pts',(1.44764665256479,1.37278636874968,30.1739870317407));
#21339=CARTESIAN_POINT('Ctrl Pts',(1.48402522927104,1.33306732363768,30.1704124377485));
#21340=CARTESIAN_POINT('Ctrl Pts',(1.49684256813808,1.31865907834359,30.1691450204073));
#21341=CARTESIAN_POINT('Ctrl Pts',(1.51276706525988,1.30022656510334,30.1675626282775));
#21342=CARTESIAN_POINT('Ctrl Pts',(1.51606997812326,1.2963738415834,30.1672339926103));
#21343=CARTESIAN_POINT('Ctrl Pts',(1.52131506047581,1.29020818864268,30.1667114827525));
#21344=CARTESIAN_POINT('Ctrl Pts',(1.52326671426154,1.28790341283503,30.1665169202843));
#21345=CARTESIAN_POINT('Ctrl Pts',(1.52695989579606,1.28352186768229,30.1661484902583));
#21346=CARTESIAN_POINT('Ctrl Pts',(1.52870240371332,1.28144600711636,30.1659745528368));
#21347=CARTESIAN_POINT('Ctrl Pts',(1.53268600418052,1.27668062987651,30.1655766549996));
#21348=CARTESIAN_POINT('Ctrl Pts',(1.534924248718,1.27398876339921,30.1653529034966));
#21349=CARTESIAN_POINT('Ctrl Pts',(1.54197073156149,1.26546865327324,30.1646478420626));
#21350=CARTESIAN_POINT('Ctrl Pts',(1.54675302050689,1.25961888972123,30.1641683817167));
#21351=CARTESIAN_POINT('Ctrl Pts',(1.62886865214448,1.15800103505688,30.1559162981046));
#21352=CARTESIAN_POINT('Ctrl Pts',(1.69722065669643,1.05528742763423,30.1487393801663));
#21353=CARTESIAN_POINT('Ctrl Pts',(1.80316997393057,0.858846372859983,30.135782691383));
#21354=CARTESIAN_POINT('Ctrl Pts',(1.84397285642237,0.767334328811819,30.130011044752));
#21355=CARTESIAN_POINT('Ctrl Pts',(1.89475235165458,0.625686499903933,30.1210623121413));
#21356=CARTESIAN_POINT('Ctrl Pts',(1.90996133925146,0.57759603000583,30.1180233262793));
#21357=CARTESIAN_POINT('Ctrl Pts',(1.93135261642658,0.499819485274614,30.1130707630029));
#21358=CARTESIAN_POINT('Ctrl Pts',(1.93870903581534,0.470478020351055,30.1111941718594));
#21359=CARTESIAN_POINT('Ctrl Pts',(1.94731138664546,0.432528673478925,30.1087520657233));
#21360=CARTESIAN_POINT('Ctrl Pts',(1.94917240423737,0.42406323193522,30.1082063554833));
#21361=CARTESIAN_POINT('Ctrl Pts',(1.95208802314533,0.410375792195459,30.1073223902778));
#21362=CARTESIAN_POINT('Ctrl Pts',(1.95317699424345,0.405161164460992,30.1069852378996));
#21363=CARTESIAN_POINT('Ctrl Pts',(1.95521640718318,0.395195944799523,30.1063401839851));
#21364=CARTESIAN_POINT('Ctrl Pts',(1.95617045725483,0.39044612328369,30.1060324003162));
#21365=CARTESIAN_POINT('Ctrl Pts',(1.95831470495417,0.379565646867008,30.1053265906224));
#21366=CARTESIAN_POINT('Ctrl Pts',(1.95949342957825,0.373432807737394,30.1049282016409));
#21367=CARTESIAN_POINT('Ctrl Pts',(1.96303802874306,0.354511498117409,30.1036973058093));
#21368=CARTESIAN_POINT('Ctrl Pts',(1.96530761165989,0.341705549883269,30.1028617468941));
#21369=CARTESIAN_POINT('Ctrl Pts',(1.98835204356511,0.203846740700948,30.0938385779487));
#21370=CARTESIAN_POINT('Ctrl Pts',(1.99728239456358,0.0771318025587282,
30.0852673401902));
#21371=CARTESIAN_POINT('Ctrl Pts',(1.9902602694282,-0.205460999781071,30.0656800467879));
#21372=CARTESIAN_POINT('Ctrl Pts',(1.9681157817375,-0.36038107897085,30.054611354457));
#21373=CARTESIAN_POINT('Ctrl Pts',(1.92349535757947,-0.52869937830307,30.0430699986609));
#21374=CARTESIAN_POINT('Ctrl Pts',(1.91860167385474,-0.546191447865313,
30.0418772846926));
#21375=CARTESIAN_POINT('Ctrl Pts',(1.91206510591828,-0.568383057686739,
30.0403748014609));
#21376=CARTESIAN_POINT('Ctrl Pts',(1.91064282657059,-0.573145932639903,
30.0400529613236));
#21377=CARTESIAN_POINT('Ctrl Pts',(1.90833452214748,-0.580771809805676,
30.0395387277533));
#21378=CARTESIAN_POINT('Ctrl Pts',(1.90745983425723,-0.583638179415678,
30.0393456829692));
#21379=CARTESIAN_POINT('Ctrl Pts',(1.90577995688558,-0.589099056214416,
30.0389783796749));
#21380=CARTESIAN_POINT('Ctrl Pts',(1.90497593704651,-0.591693857879293,
30.0388040585938));
#21381=CARTESIAN_POINT('Ctrl Pts',(1.90311049600848,-0.597670953478845,
30.0384029780734));
#21382=CARTESIAN_POINT('Ctrl Pts',(1.90204535819706,-0.601052064704276,
30.038176439128));
#21383=CARTESIAN_POINT('Ctrl Pts',(1.89916467344168,-0.610111998177867,
30.0375702883828));
#21384=CARTESIAN_POINT('Ctrl Pts',(1.89733265355348,-0.61578560481305,30.0371916238709));
#21385=CARTESIAN_POINT('Ctrl Pts',(1.88383338224745,-0.656959460811448,
30.0344497780979));
#21386=CARTESIAN_POINT('Ctrl Pts',(1.87119516144548,-0.692136581925847,
30.0321405607066));
#21387=CARTESIAN_POINT('Ctrl Pts',(1.82656844291455,-0.806172713941301,
30.0247006622978));
#21388=CARTESIAN_POINT('Ctrl Pts',(1.79052151244,-0.883346979058934,30.0197369165592));
#21389=CARTESIAN_POINT('Ctrl Pts',(1.70125728344307,-1.04637754464846,30.0089438351228));
#21390=CARTESIAN_POINT('Ctrl Pts',(1.64623431731441,-1.13097027787818,30.0031348664401));
#21391=CARTESIAN_POINT('Ctrl Pts',(1.55390433102242,-1.25181553033917,29.9940972528022));
#21392=CARTESIAN_POINT('Ctrl Pts',(1.52119051994729,-1.29137120457922,29.9910065241158));
#21393=CARTESIAN_POINT('Ctrl Pts',(1.46656997161629,-1.35245649742028,29.9859770507631));
#21394=CARTESIAN_POINT('Ctrl Pts',(1.44562755267283,-1.37481885299057,29.9840767912153));
#21395=CARTESIAN_POINT('Ctrl Pts',(1.41808315652934,-1.402905388239,29.9816080421236));
#21396=CARTESIAN_POINT('Ctrl Pts',(1.41194640158631,-1.40908151728623,29.981059901067));
#21397=CARTESIAN_POINT('Ctrl Pts',(1.40198388105152,-1.41897753002168,29.9801729505615));
#21398=CARTESIAN_POINT('Ctrl Pts',(1.3981832320712,-1.42272263006079,29.9798352574502));
#21399=CARTESIAN_POINT('Ctrl Pts',(1.39090469115614,-1.42983745689816,29.9791898025587));
#21400=CARTESIAN_POINT('Ctrl Pts',(1.38742946003484,-1.43320986103817,29.9788821613116));
#21401=CARTESIAN_POINT('Ctrl Pts',(1.37945653546241,-1.44089070407277,29.9781775731668));
#21402=CARTESIAN_POINT('Ctrl Pts',(1.3749508917345,-1.4451907826226,29.977780267753));
#21403=CARTESIAN_POINT('Ctrl Pts',(1.36103738448895,-1.45834553981789,29.9765559875253));
#21404=CARTESIAN_POINT('Ctrl Pts',(1.35156372418896,-1.4671298381135,29.9757260079733));
#21405=CARTESIAN_POINT('Ctrl Pts',(1.26044409600532,-1.5499874632589,29.967776057998));
#21406=CARTESIAN_POINT('Ctrl Pts',(1.17288938503415,-1.61725183938662,29.9603703392054));
#21407=CARTESIAN_POINT('Ctrl Pts',(0.935667596511906,-1.77006464507373,
29.9409268967729));
#21408=CARTESIAN_POINT('Ctrl Pts',(0.779661265895116,-1.84410734432581,
29.9286576484827));
#21409=CARTESIAN_POINT('Ctrl Pts',(0.598277101336207,-1.90300891659655,
29.9160090894163));
#21410=CARTESIAN_POINT('Ctrl Pts',(0.580380124860129,-1.90854326648443,
29.9147784256211));
#21411=CARTESIAN_POINT('Ctrl Pts',(0.557586649798532,-1.91524148176705,
29.913235285106));
#21412=CARTESIAN_POINT('Ctrl Pts',(0.552760837188338,-1.91663983672436,
29.9129099414633));
#21413=CARTESIAN_POINT('Ctrl Pts',(0.54503665523231,-1.91884643989487,29.9123914405375));
#21414=CARTESIAN_POINT('Ctrl Pts',(0.542141691221527,-1.91966637788402,
29.9121976129662));
#21415=CARTESIAN_POINT('Ctrl Pts',(0.53663268622214,-1.92121323230813,29.9118297365021));
#21416=CARTESIAN_POINT('Ctrl Pts',(0.534019049742052,-1.92194135667876,
29.9116556212613));
#21417=CARTESIAN_POINT('Ctrl Pts',(0.528009453264891,-1.92360234512286,
29.9112562181817));
#21418=CARTESIAN_POINT('Ctrl Pts',(0.524612505404947,-1.92453154937436,
29.9110311447455));
#21419=CARTESIAN_POINT('Ctrl Pts',(0.515534613523457,-1.92698890307561,
29.9104314651091));
#21420=CARTESIAN_POINT('Ctrl Pts',(0.509849286799737,-1.92850094040665,
29.9100577747491));
#21421=CARTESIAN_POINT('Ctrl Pts',(0.469566370420368,-1.93902376589892,
29.9074227588315));
#21422=CARTESIAN_POINT('Ctrl Pts',(0.434736163110228,-1.94712880776038,
29.9052107850648));
#21423=CARTESIAN_POINT('Ctrl Pts',(0.386656507434843,-1.95696235935127,
29.9022243398097));
#21424=CARTESIAN_POINT('Ctrl Pts',(0.373581970546604,-1.95950030801102,
29.9014189537047));
#21425=CARTESIAN_POINT('Ctrl Pts',(0.336881953554389,-1.96624360463748,
29.899174636119));
#21426=CARTESIAN_POINT('Ctrl Pts',(0.313204132028088,-1.97015395452307,
29.8977456068746));
#21427=CARTESIAN_POINT('Ctrl Pts',(0.18450760265531,-1.98902906657953,29.8900537795893));
#21428=CARTESIAN_POINT('Ctrl Pts',(0.0784906052197476,-1.99602619720032,
29.8839799332439));
#21429=CARTESIAN_POINT('Ctrl Pts',(-0.145681996287054,-1.99292607095643,
29.8709016394709));
#21430=CARTESIAN_POINT('Ctrl Pts',(-0.263384832330395,-1.9808079286306,
29.8638892917108));
#21431=CARTESIAN_POINT('Ctrl Pts',(-0.39255818662144,-1.95578822709646,
29.8556816097451));
#21432=CARTESIAN_POINT('Ctrl Pts',(-0.405774564570033,-1.95308896562998,
29.8548360114642));
#21433=CARTESIAN_POINT('Ctrl Pts',(-0.42515941144419,-1.94892463013027,
29.8535867749573));
#21434=CARTESIAN_POINT('Ctrl Pts',(-0.431350086775581,-1.94756382185559,
29.8531864729945));
#21435=CARTESIAN_POINT('Ctrl Pts',(-0.44227311022526,-1.94510813366725,
29.852477737646));
#21436=CARTESIAN_POINT('Ctrl Pts',(-0.447008164803977,-1.94402542565722,
29.8521696971042));
#21437=CARTESIAN_POINT('Ctrl Pts',(-0.456251663323227,-1.94187626934649,
29.8515667574413));
#21438=CARTESIAN_POINT('Ctrl Pts',(-0.460760442578518,-1.94081138694474,
29.851271910462));
#21439=CARTESIAN_POINT('Ctrl Pts',(-0.472902267712806,-1.93789903870934,
29.8504758744366));
#21440=CARTESIAN_POINT('Ctrl Pts',(-0.480528118888391,-1.93602220107952,
29.8499737416978));
#21441=CARTESIAN_POINT('Ctrl Pts',(-0.508515430137787,-1.92895855597037,
29.8481227675753));
#21442=CARTESIAN_POINT('Ctrl Pts',(-0.528805068106709,-1.92349530727224,
29.8467650347883));
#21443=CARTESIAN_POINT('Ctrl Pts',(-0.702168349245475,-1.87386475958351,
29.835023170862));
#21444=CARTESIAN_POINT('Ctrl Pts',(-0.849498380171197,-1.8118339125268,
29.8240271018646));
#21445=CARTESIAN_POINT('Ctrl Pts',(-1.05351260044327,-1.69553850004089,
29.8076424475808));
#21446=CARTESIAN_POINT('Ctrl Pts',(-1.11699486635934,-1.65440717737234,
29.8023685791579));
#21447=CARTESIAN_POINT('Ctrl Pts',(-1.20588760888744,-1.58935757225439,
29.7948510907989));
#21448=CARTESIAN_POINT('Ctrl Pts',(-1.2332495311162,-1.56822138432968,29.7925178193457));
#21449=CARTESIAN_POINT('Ctrl Pts',(-1.27499571825495,-1.53420506201687,
29.78894394596));
#21450=CARTESIAN_POINT('Ctrl Pts',(-1.289764900205,-1.52181004868533,29.7876767303591));
#21451=CARTESIAN_POINT('Ctrl Pts',(-1.30819190051769,-1.50588421300893,
29.786094553357));
#21452=CARTESIAN_POINT('Ctrl Pts',(-1.31201846812658,-1.502551447451,29.7857659354969));
#21453=CARTESIAN_POINT('Ctrl Pts',(-1.31810208379111,-1.49721193543508,
29.7852434473215));
#21454=CARTESIAN_POINT('Ctrl Pts',(-1.32036733210652,-1.49521463058243,
29.7850488888265));
#21455=CARTESIAN_POINT('Ctrl Pts',(-1.32465691245024,-1.49141509063294,
29.7846804618319));
#21456=CARTESIAN_POINT('Ctrl Pts',(-1.32668208225354,-1.48961389661295,
29.7845065234876));
#21457=CARTESIAN_POINT('Ctrl Pts',(-1.33131480846138,-1.48547659007489,
29.784108617686));
#21458=CARTESIAN_POINT('Ctrl Pts',(-1.33391988743018,-1.48313773914112,
29.7838848591704));
#21459=CARTESIAN_POINT('Ctrl Pts',(-1.34212810592106,-1.47572924534879,
29.7831797535112));
#21460=CARTESIAN_POINT('Ctrl Pts',(-1.34770868755247,-1.47063454201164,
29.7827002562826));
#21461=CARTESIAN_POINT('Ctrl Pts',(-1.44350876425442,-1.3821720934168,29.7744641282722));
#21462=CARTESIAN_POINT('Ctrl Pts',(-1.52588213403983,-1.29066298475416,
29.7673007549229));
#21463=CARTESIAN_POINT('Ctrl Pts',(-1.65917078808642,-1.11184925662339,
29.7543532894403));
#21464=CARTESIAN_POINT('Ctrl Pts',(-1.71288817501726,-1.02716571279457,
29.748577090161));
#21465=CARTESIAN_POINT('Ctrl Pts',(-1.78379968354245,-0.894225745179675,
29.7396175415534));
#21466=CARTESIAN_POINT('Ctrl Pts',(-1.80587759752339,-0.848755862964658,
29.7365722738101));
#21467=CARTESIAN_POINT('Ctrl Pts',(-1.83839194569144,-0.774764712321493,
29.7316103664774));
#21468=CARTESIAN_POINT('Ctrl Pts',(-1.84994556731505,-0.746757356213623,
29.7297308933589));
#21469=CARTESIAN_POINT('Ctrl Pts',(-1.86398024165095,-0.710408636922516,
29.7272855418833));
#21470=CARTESIAN_POINT('Ctrl Pts',(-1.86705115570611,-0.702298192243683,
29.7267395340787));
#21471=CARTESIAN_POINT('Ctrl Pts',(-1.87192324721275,-0.689172916463398,
29.7258552034461));
#21472=CARTESIAN_POINT('Ctrl Pts',(-1.87375741228224,-0.684170381747702,
29.7255179848849));
#21473=CARTESIAN_POINT('Ctrl Pts',(-1.87722090542567,-0.674605590966897,
29.7248728821735));
#21474=CARTESIAN_POINT('Ctrl Pts',(-1.87885370165506,-0.670044624057021,
29.7245651162179));
#21475=CARTESIAN_POINT('Ctrl Pts',(-1.88255262427622,-0.659592415705384,
29.7238594573999));
#21476=CARTESIAN_POINT('Ctrl Pts',(-1.88460773234966,-0.653697354842725,
29.7234612021293));
#21477=CARTESIAN_POINT('Ctrl Pts',(-1.89085517223222,-0.635502278453995,
29.7222311237586));
#21478=CARTESIAN_POINT('Ctrl Pts',(-1.8949549442572,-0.623171063373311,
29.7213962544618));
#21479=CARTESIAN_POINT('Ctrl Pts',(-1.93511570973685,-0.498314278954933,
29.7129293291086));
#21480=CARTESIAN_POINT('Ctrl Pts',(-1.9612246098998,-0.382856239917268,
29.7049666528438));
#21481=CARTESIAN_POINT('Ctrl Pts',(-1.98887518461848,-0.177185840241624,
29.6906262161521));
#21482=CARTESIAN_POINT('Ctrl Pts',(-1.99481690558367,-0.0878868767612705,
29.6843555906316));
#21483=CARTESIAN_POINT('Ctrl Pts',(-1.99468269335407,0.0899240126054698,
29.6720070532425));
#21484=CARTESIAN_POINT('Ctrl Pts',(-1.98873717617692,0.178252204240259,
29.6659421718432));
#21485=CARTESIAN_POINT('Ctrl Pts',(-1.97590266168009,0.273674450671789,
29.659653047608));
#21486=CARTESIAN_POINT('Ctrl Pts',(-1.97481170536337,0.281438744108537,
29.6591432579223));
#21487=CARTESIAN_POINT('Ctrl Pts',(-1.9731597213127,0.292713012403177,29.6584060316065));
#21488=CARTESIAN_POINT('Ctrl Pts',(-1.97263506419656,0.29622811720631,29.6581766059426));
#21489=CARTESIAN_POINT('Ctrl Pts',(-1.97169260979237,0.302428837526234,
29.6577726716034));
#21490=CARTESIAN_POINT('Ctrl Pts',(-1.97127871491979,0.305115023790714,
29.657597943365));
#21491=CARTESIAN_POINT('Ctrl Pts',(-1.97039760502827,0.310756808663185,
29.6572315131497));
#21492=CARTESIAN_POINT('Ctrl Pts',(-1.9699292305424,0.31371219768379,29.6570398781321));
#21493=CARTESIAN_POINT('Ctrl Pts',(-1.96866837429776,0.321553880574816,
29.6565322143381));
#21494=CARTESIAN_POINT('Ctrl Pts',(-1.96786434482808,0.326438336739092,
29.6562168353945));
#21495=CARTESIAN_POINT('Ctrl Pts',(-1.96406089804911,0.34901935900467,29.6547624873377));
#21496=CARTESIAN_POINT('Ctrl Pts',(-1.9608407825424,0.366678611527238,29.6536355387752));
#21497=CARTESIAN_POINT('Ctrl Pts',(-1.95135780568296,0.414979847897621,
29.6505757688381));
#21498=CARTESIAN_POINT('Ctrl Pts',(-1.94461183516986,0.445522833706953,
29.6486660442634));
#21499=CARTESIAN_POINT('Ctrl Pts',(-1.91836248795739,0.552371595047287,
29.6420339473941));
#21500=CARTESIAN_POINT('Ctrl Pts',(-1.89506135114121,0.627672866895404,
29.6374463997027));
#21501=CARTESIAN_POINT('Ctrl Pts',(-1.81072224382273,0.852211318433263,
29.6235232603464));
#21502=CARTESIAN_POINT('Ctrl Pts',(-1.73602666167702,0.995581932743773,
29.614238060434));
#21503=CARTESIAN_POINT('Ctrl Pts',(-1.63819113968824,1.13819963853713,29.603535906655));
#21504=CARTESIAN_POINT('Ctrl Pts',(-1.63138520232766,1.14793333410339,29.6027978258839));
#21505=CARTESIAN_POINT('Ctrl Pts',(-1.61697564899362,1.16815457204016,29.6012479664391));
#21506=CARTESIAN_POINT('Ctrl Pts',(-1.6093560098812,1.17862995654739,29.6004356104254));
#21507=CARTESIAN_POINT('Ctrl Pts',(-1.59791849996567,1.19403639163864,29.5992263880552));
#21508=CARTESIAN_POINT('Ctrl Pts',(-1.59417855627439,1.19902508996725,29.5988325556329));
#21509=CARTESIAN_POINT('Ctrl Pts',(-1.58749192040203,1.20785778294067,29.5981311557343));
#21510=CARTESIAN_POINT('Ctrl Pts',(-1.58455448751181,1.21170875072365,29.5978239536142));
#21511=CARTESIAN_POINT('Ctrl Pts',(-1.57835367276,1.21977689777012,29.5971773684635));
#21512=CARTESIAN_POINT('Ctrl Pts',(-1.57508735206549,1.22399176022619,29.5968378706508));
#21513=CARTESIAN_POINT('Ctrl Pts',(-1.5664529748821,1.23504177061498,29.5959432562952));
#21514=CARTESIAN_POINT('Ctrl Pts',(-1.56105712497378,1.24185496185503,29.5953870352665));
#21515=CARTESIAN_POINT('Ctrl Pts',(-1.53653758136221,1.2724027940613,29.5928720001395));
#21516=CARTESIAN_POINT('Ctrl Pts',(-1.51691679507018,1.29573140545769,29.5908932323507));
#21517=CARTESIAN_POINT('Ctrl Pts',(-1.46308431817299,1.35683774807051,29.5855486130291));
#21518=CARTESIAN_POINT('Ctrl Pts',(-1.42794830067102,1.39376730676925,29.5821457534618));
#21519=CARTESIAN_POINT('Ctrl Pts',(-1.31940463850189,1.49943512045892,29.5718814143154));
#21520=CARTESIAN_POINT('Ctrl Pts',(-1.24217729250116,1.56400976385522,29.5648828858498));
#21521=CARTESIAN_POINT('Ctrl Pts',(-1.06136825096233,1.69332661587501,29.5493732462378));
#21522=CARTESIAN_POINT('Ctrl Pts',(-0.956024337976294,1.75495937265301,
29.5408843601799));
#21523=CARTESIAN_POINT('Ctrl Pts',(-0.838841317786708,1.80981497286336,
29.5324367075282));
#21524=CARTESIAN_POINT('Ctrl Pts',(-0.831959469096917,1.81298881372095,
29.5319441211451));
#21525=CARTESIAN_POINT('Ctrl Pts',(-0.821868361964223,1.81757317423066,
29.5312271403572));
#21526=CARTESIAN_POINT('Ctrl Pts',(-0.818673311137647,1.81901452940124,
29.531000905191));
#21527=CARTESIAN_POINT('Ctrl Pts',(-0.813000479095079,1.82155569010856,
29.5306006188287));
#21528=CARTESIAN_POINT('Ctrl Pts',(-0.810524237857629,1.82265887411017,
29.5304263611579));
#21529=CARTESIAN_POINT('Ctrl Pts',(-0.805286672135983,1.82497946422341,
29.5300587849174));
#21530=CARTESIAN_POINT('Ctrl Pts',(-0.802524839234077,1.82619564994166,
29.529865541486));
#21531=CARTESIAN_POINT('Ctrl Pts',(-0.795120924133763,1.8294359579301,29.5293490298217));
#21532=CARTESIAN_POINT('Ctrl Pts',(-0.790473837363793,1.83144869487509,
29.5290264522268));
#21533=CARTESIAN_POINT('Ctrl Pts',(-0.768202472402139,1.8409942637053,29.5274879525778));
#21534=CARTESIAN_POINT('Ctrl Pts',(-0.750477170208798,1.84829083219049,
29.5262858109905));
#21535=CARTESIAN_POINT('Ctrl Pts',(-0.700762706701203,1.86792249549073,
29.5229686086327));
#21536=CARTESIAN_POINT('Ctrl Pts',(-0.668555464807695,1.87969058560893,
29.5208816631549));
#21537=CARTESIAN_POINT('Ctrl Pts',(-0.549982384435761,1.91958191382647,
29.5133682219611));
#21538=CARTESIAN_POINT('Ctrl Pts',(-0.462022617878833,1.9426303534154,29.5081145492054));
#21539=CARTESIAN_POINT('Ctrl Pts',(-0.218449517138189,1.98896744515433,
29.493734928394));
#21540=CARTESIAN_POINT('Ctrl Pts',(-0.0612028394111058,1.99998914096932,
29.4845880091085));
#21541=CARTESIAN_POINT('Ctrl Pts',(0.108221522271149,1.99185161473854,29.4739955096605));
#21542=CARTESIAN_POINT('Ctrl Pts',(0.120738466222123,1.9911320810915,29.4732089718794));
#21543=CARTESIAN_POINT('Ctrl Pts',(0.139386752225096,1.98988360319602,29.4720309176832));
#21544=CARTESIAN_POINT('Ctrl Pts',(0.145523941327363,1.98944419426288,29.4716422099475));
#21545=CARTESIAN_POINT('Ctrl Pts',(0.156478485427015,1.98860891306648,29.4709465491798));
#21546=CARTESIAN_POINT('Ctrl Pts',(0.161296640220893,1.98822391060676,29.4706399398293));
#21547=CARTESIAN_POINT('Ctrl Pts',(0.171471438358703,1.98737364838928,29.4699910897493));
#21548=CARTESIAN_POINT('Ctrl Pts',(0.176827687050827,1.98690423539829,29.4696487207939));
#21549=CARTESIAN_POINT('Ctrl Pts',(0.191035449280268,1.98560118446814,29.4687384126165));
#21550=CARTESIAN_POINT('Ctrl Pts',(0.199883320149152,1.98473002212479,29.4681692977063));
#21551=CARTESIAN_POINT('Ctrl Pts',(0.241080165248053,1.98039550721082,29.4655088380872));
#21552=CARTESIAN_POINT('Ctrl Pts',(0.273345546375769,1.97620039863636,29.4633946024729));
#21553=CARTESIAN_POINT('Ctrl Pts',(0.360613604713349,1.96267590587993,29.4575891008301));
#21554=CARTESIAN_POINT('Ctrl Pts',(0.415347551650833,1.95182589837783,29.4538524908469));
#21555=CARTESIAN_POINT('Ctrl Pts',(0.570931040727586,1.91414370410869,29.4429638838575));
#21556=CARTESIAN_POINT('Ctrl Pts',(0.6702219243729,1.88167683896254,29.4356774166701));
#21557=CARTESIAN_POINT('Ctrl Pts',(0.837265265202727,1.81215010657783,29.4230613258358));
#21558=CARTESIAN_POINT('Ctrl Pts',(0.90626945205378,1.77864511198752,29.4177387087298));
#21559=CARTESIAN_POINT('Ctrl Pts',(1.00434662604989,1.72383013431698,29.4101549621578));
#21560=CARTESIAN_POINT('Ctrl Pts',(1.03504405586912,1.70557517293847,29.4077789588422));
#21561=CARTESIAN_POINT('Ctrl Pts',(1.07020890669867,1.68336420291293,29.4050687400411));
#21562=CARTESIAN_POINT('Ctrl Pts',(1.0751669282844,1.68020183967615,29.4046868922337));
#21563=CARTESIAN_POINT('Ctrl Pts',(1.08307115893924,1.67511098882462,29.4040786726542));
#21564=CARTESIAN_POINT('Ctrl Pts',(1.08602632523621,1.6731965758895,29.403851396787));
#21565=CARTESIAN_POINT('Ctrl Pts',(1.09124954002506,1.66979321013697,29.4034499247904));
#21566=CARTESIAN_POINT('Ctrl Pts',(1.09351963681289,1.66830744393357,29.4032755179165));
#21567=CARTESIAN_POINT('Ctrl Pts',(1.09830119694076,1.66516398542629,29.4029083356749));
#21568=CARTESIAN_POINT('Ctrl Pts',(1.10081193618029,1.66350524466242,29.402715632723));
#21569=CARTESIAN_POINT('Ctrl Pts',(1.10750597897225,1.65906097775051,29.4022020949817));
#21570=CARTESIAN_POINT('Ctrl Pts',(1.1116825593925,1.65626528968634,29.4018819370027));
#21571=CARTESIAN_POINT('Ctrl Pts',(1.13138916337494,1.64296610587366,29.4003722807648));
#21572=CARTESIAN_POINT('Ctrl Pts',(1.14678179656807,1.63225936567296,29.3991959452767));
#21573=CARTESIAN_POINT('Ctrl Pts',(1.18903581765834,1.60197565289214,29.3959678785352));
#21574=CARTESIAN_POINT('Ctrl Pts',(1.21556333250924,1.5819412811859,29.3939424630068));
#21575=CARTESIAN_POINT('Ctrl Pts',(1.30966758123519,1.50710526837466,29.3867125361567));
#21576=CARTESIAN_POINT('Ctrl Pts',(1.3741456414647,1.44855835576325,29.381669042052));
#21577=CARTESIAN_POINT('Ctrl Pts',(1.53846118282463,1.27847941958292,29.3679530908451));
#21578=CARTESIAN_POINT('Ctrl Pts',(1.62989688063555,1.15965574372557,29.3592842263497));
#21579=CARTESIAN_POINT('Ctrl Pts',(1.71480370255174,1.01916234515257,29.3491293066863));
#21580=CARTESIAN_POINT('Ctrl Pts',(1.72226702145372,1.00649883905141,29.3482152320256));
#21581=CARTESIAN_POINT('Ctrl Pts',(1.73472791365769,0.984811154490312,29.3466512271324));
#21582=CARTESIAN_POINT('Ctrl Pts',(1.73979675418513,0.975828464525246,29.3460038599903));
#21583=CARTESIAN_POINT('Ctrl Pts',(1.74782723583675,0.961335862312169,29.344959886108));
#21584=CARTESIAN_POINT('Ctrl Pts',(1.75083306420175,0.955850546032718,29.3445648620706));
#21585=CARTESIAN_POINT('Ctrl Pts',(1.75612871361583,0.946077760408783,29.3438612313486));
#21586=CARTESIAN_POINT('Ctrl Pts',(1.75842876675791,0.941795869113549,29.3435529919384));
#21587=CARTESIAN_POINT('Ctrl Pts',(1.76319051860419,0.932852905361689,29.3429093053458));
#21588=CARTESIAN_POINT('Ctrl Pts',(1.76564943456453,0.928190401415687,29.3425737625582));
#21589=CARTESIAN_POINT('Ctrl Pts',(1.77198615028136,0.916058662110182,29.341700785273));
#21590=CARTESIAN_POINT('Ctrl Pts',(1.77583518122866,0.908574595026239,29.3411623416014));
#21591=CARTESIAN_POINT('Ctrl Pts',(1.79221870899521,0.876216575432168,29.3388345617276));
#21592=CARTESIAN_POINT('Ctrl Pts',(1.804278300622,0.851106968125027,29.3370287374579));
#21593=CARTESIAN_POINT('Ctrl Pts',(1.83446293809845,0.784731885145469,29.3322538886938));
#21594=CARTESIAN_POINT('Ctrl Pts',(1.85172134675272,0.743092143853861,29.3292568521593));
#21595=CARTESIAN_POINT('Ctrl Pts',(1.93290702330323,0.526774165873512,29.3136804573127));
#21596=CARTESIAN_POINT('Ctrl Pts',(1.97357526088913,0.344391154345442,29.3004112078428));
#21597=CARTESIAN_POINT('Ctrl Pts',(1.98903093849333,0.151149127975669,29.2872158370067));
#21598=CARTESIAN_POINT('Ctrl Pts',(1.9896146876436,0.143260361243321,29.2866788402576));
#21599=CARTESIAN_POINT('Ctrl Pts',(1.99280073243957,0.0964198891996078,
29.2835010760387));
#21600=CARTESIAN_POINT('Ctrl Pts',(1.99430625162311,0.0573988624375412,
29.2808976380761));
#21601=CARTESIAN_POINT('Ctrl Pts',(1.99472650006532,0.0117317454929255,
29.277920722126));
#21602=CARTESIAN_POINT('Ctrl Pts',(1.99475446156921,0.00510734466025873,
29.2774906188408));
#21603=CARTESIAN_POINT('Ctrl Pts',(1.99474683809922,-0.00491576492343968,
29.2768425789152));
#21604=CARTESIAN_POINT('Ctrl Pts',(1.99473556759528,-0.00831436368357211,
29.2766233191499));
#21605=CARTESIAN_POINT('Ctrl Pts',(1.99469979830948,-0.0144058748249083,
29.2762311985545));
#21606=CARTESIAN_POINT('Ctrl Pts',(1.99467853223731,-0.0170987698666067,
29.2760581590104));
#21607=CARTESIAN_POINT('Ctrl Pts',(1.99462085554161,-0.0229115665326558,
29.2756853059508));
#21608=CARTESIAN_POINT('Ctrl Pts',(1.99458257860969,-0.0260314170960715,
29.2754855985625));
#21609=CARTESIAN_POINT('Ctrl Pts',(1.99445623140718,-0.0346761467921984,
29.2749333398556));
#21610=CARTESIAN_POINT('Ctrl Pts',(1.99435252395427,-0.0402008221434106,
29.2745816545407));
#21611=CARTESIAN_POINT('Ctrl Pts',(1.99365218038771,-0.0707451848983417,
29.2726438590587));
#21612=CARTESIAN_POINT('Ctrl Pts',(1.99260765508568,-0.0957537034461689,
29.2710816526476));
#21613=CARTESIAN_POINT('Ctrl Pts',(1.98129094390957,-0.282378853568761,
29.2595619515875));
#21614=CARTESIAN_POINT('Ctrl Pts',(1.95184123842895,-0.442246226024752,
29.2504300232227));
#21615=CARTESIAN_POINT('Ctrl Pts',(1.86958648990062,-0.704577793124424,
29.2343627628488));
#21616=CARTESIAN_POINT('Ctrl Pts',(1.82670905431181,-0.80926638931887,29.2276365199524));
#21617=CARTESIAN_POINT('Ctrl Pts',(1.76930240973371,-0.921284060672225,
29.2197798315951));
#21618=CARTESIAN_POINT('Ctrl Pts',(1.7632829307337,-0.932753253072947,29.2189675141049));
#21619=CARTESIAN_POINT('Ctrl Pts',(1.75420119853841,-0.949654985046272,
29.2177583381817));
#21620=CARTESIAN_POINT('Ctrl Pts',(1.75122439982988,-0.955133255406537,
29.2173645133408));
#21621=CARTESIAN_POINT('Ctrl Pts',(1.74588959366236,-0.964842239821923,
29.2166631219817));
#21622=CARTESIAN_POINT('Ctrl Pts',(1.74354175804883,-0.969078509856197,
29.2163559207877));
#21623=CARTESIAN_POINT('Ctrl Pts',(1.73857666037765,-0.977960731986841,
29.2157093325255));
#21624=CARTESIAN_POINT('Ctrl Pts',(1.73595615400385,-0.982604817708438,
29.2153698306559));
#21625=CARTESIAN_POINT('Ctrl Pts',(1.7290155555785,-0.994790586581263,29.2144751941241));
#21626=CARTESIAN_POINT('Ctrl Pts',(1.72466477671083,-1.0023145746672,29.2139189548768));
#21627=CARTESIAN_POINT('Ctrl Pts',(1.70483345895507,-1.03609828577954,29.2114037202105));
#21628=CARTESIAN_POINT('Ctrl Pts',(1.6888020874888,-1.06202830414087,29.2094247672188));
#21629=CARTESIAN_POINT('Ctrl Pts',(1.64439607954055,-1.13030375973011,29.204079526719));
#21630=CARTESIAN_POINT('Ctrl Pts',(1.61498357460313,-1.17194384135886,29.2006762205873));
#21631=CARTESIAN_POINT('Ctrl Pts',(1.52290448083161,-1.29224504771991,29.1904110380524));
#21632=CARTESIAN_POINT('Ctrl Pts',(1.45585454405651,-1.36734032141634,29.1834121149305));
#21633=CARTESIAN_POINT('Ctrl Pts',(1.2957328348618,-1.5214877184818,29.1679047352846));
#21634=CARTESIAN_POINT('Ctrl Pts',(1.20047171591933,-1.59772446057512,29.1594185247704));
#21635=CARTESIAN_POINT('Ctrl Pts',(1.09313300079835,-1.66857262417747,29.1510212467001));
#21636=CARTESIAN_POINT('Ctrl Pts',(1.08740423646716,-1.67231169026018,29.150576386859));
#21637=CARTESIAN_POINT('Ctrl Pts',(1.07875334735924,-1.67789472695013,29.149909714621));
#21638=CARTESIAN_POINT('Ctrl Pts',(1.07584555489214,-1.67976065009983,29.1496864901218));
#21639=CARTESIAN_POINT('Ctrl Pts',(1.07080017794599,-1.68297978050172,29.1493006786138));
#21640=CARTESIAN_POINT('Ctrl Pts',(1.06866485186282,-1.68433648575218,29.149137860532));
#21641=CARTESIAN_POINT('Ctrl Pts',(1.0642315057073,-1.68714144130097,29.1488007952327));
#21642=CARTESIAN_POINT('Ctrl Pts',(1.06193310394885,-1.68858906296089,29.1486265918141));
#21643=CARTESIAN_POINT('Ctrl Pts',(1.05641288901803,-1.69205017789126,29.1482094800557));
#21644=CARTESIAN_POINT('Ctrl Pts',(1.05318824484642,-1.69405918376061,29.1479668686416));
#21645=CARTESIAN_POINT('Ctrl Pts',(1.04628075485438,-1.69833531648587,29.1474493591027));
#21646=CARTESIAN_POINT('Ctrl Pts',(1.04259622788232,-1.70059970940683,29.1471746368819));
#21647=CARTESIAN_POINT('Ctrl Pts',(1.03242275924415,-1.70680650822678,29.1464196460598));
#21648=CARTESIAN_POINT('Ctrl Pts',(1.02591854938596,-1.71072392413257,29.1459409242689));
#21649=CARTESIAN_POINT('Ctrl Pts',(0.967963137306254,-1.74518043883418,
29.141708940551));
#21650=CARTESIAN_POINT('Ctrl Pts',(0.91517909713262,-1.77343060331604,29.138088701647));
#21651=CARTESIAN_POINT('Ctrl Pts',(0.7373153419182,-1.85856314200701,29.1263810362761));
#21652=CARTESIAN_POINT('Ctrl Pts',(0.607635294874978,-1.90490776991815,
29.1185892814105));
#21653=CARTESIAN_POINT('Ctrl Pts',(0.382335811180314,-1.96004968451904,
29.1049355028131));
#21654=CARTESIAN_POINT('Ctrl Pts',(0.28898325439819,-1.97597077470157,29.0992513680315));
#21655=CARTESIAN_POINT('Ctrl Pts',(0.182263431093813,-1.98644603354663,
29.0925557835163));
#21656=CARTESIAN_POINT('Ctrl Pts',(0.169654133564061,-1.98756264447166,
29.0917617304716));
#21657=CARTESIAN_POINT('Ctrl Pts',(0.1508775158442,-1.9890454223966,29.0905745955482));
#21658=CARTESIAN_POINT('Ctrl Pts',(0.144717573471841,-1.98950308863245,
29.090184387057));
#21659=CARTESIAN_POINT('Ctrl Pts',(0.133731026157236,-1.990268063626,29.089487052718));
#21660=CARTESIAN_POINT('Ctrl Pts',(0.128905221234699,-1.99058644517388,
29.0891802768922));
#21661=CARTESIAN_POINT('Ctrl Pts',(0.118725365463809,-1.99122088572276,
29.0885321246352));
#21662=CARTESIAN_POINT('Ctrl Pts',(0.113371110068733,-1.9915329067375,29.088190624007));
#21663=CARTESIAN_POINT('Ctrl Pts',(0.0991983455425936,-1.99230148953258,
29.0872850624796));
#21664=CARTESIAN_POINT('Ctrl Pts',(0.0903780290164882,-1.99272109053517,
29.0867198476139));
#21665=CARTESIAN_POINT('Ctrl Pts',(0.0496833626137043,-1.99438628389095,
29.0841042826778));
#21666=CARTESIAN_POINT('Ctrl Pts',(0.0177863390575472,-1.99492569689813,
29.082031971538));
#21667=CARTESIAN_POINT('Ctrl Pts',(-0.068374917324342,-1.99431628173908,
29.0763705137672));
#21668=CARTESIAN_POINT('Ctrl Pts',(-0.122598623136321,-1.99171816591562,
29.0727387323324));
#21669=CARTESIAN_POINT('Ctrl Pts',(-0.352674846251479,-1.97126340031703,
29.0570458634451));
#21670=CARTESIAN_POINT('Ctrl Pts',(-0.525820179741654,-1.93229452706614,
29.0444416512425));
#21671=CARTESIAN_POINT('Ctrl Pts',(-0.702560740995732,-1.86696908936891,
29.031659069985));
#21672=CARTESIAN_POINT('Ctrl Pts',(-0.71352819186916,-1.86280506394832,
29.0308666179083));
#21673=CARTESIAN_POINT('Ctrl Pts',(-0.753443472610029,-1.84724613329007,
29.0279868409863));
#21674=CARTESIAN_POINT('Ctrl Pts',(-0.782162225180227,-1.83527051486149,
29.0259231268357));
#21675=CARTESIAN_POINT('Ctrl Pts',(-0.815741446972016,-1.82033657015145,
29.0235296790506));
#21676=CARTESIAN_POINT('Ctrl Pts',(-0.82088227714723,-1.81802409936181,
29.0231638026675));
#21677=CARTESIAN_POINT('Ctrl Pts',(-0.829186504529237,-1.81424625018304,
29.0225737585325));
#21678=CARTESIAN_POINT('Ctrl Pts',(-0.832355938761917,-1.81279433672401,
29.0223487897179));
#21679=CARTESIAN_POINT('Ctrl Pts',(-0.837974475018411,-1.81020265125403,
29.021950412703));
#21680=CARTESIAN_POINT('Ctrl Pts',(-0.840425079500347,-1.80906620814867,
29.021776801773));
#21681=CARTESIAN_POINT('Ctrl Pts',(-0.845166886736786,-1.80685552808274,
29.0214411619055));
#21682=CARTESIAN_POINT('Ctrl Pts',(-0.847458339547273,-1.8057819161533,
29.021279095258));
#21683=CARTESIAN_POINT('Ctrl Pts',(-0.853903828548873,-1.80274704726758,
29.0208235755316));
#21684=CARTESIAN_POINT('Ctrl Pts',(-0.858053176041891,-1.80077578086284,
29.0205307375961));
#21685=CARTESIAN_POINT('Ctrl Pts',(-0.875450133658827,-1.79243707481151,
29.0193045169851));
#21686=CARTESIAN_POINT('Ctrl Pts',(-0.888634385470293,-1.78593744659649,
29.0183790373044));
#21687=CARTESIAN_POINT('Ctrl Pts',(-0.923084770713577,-1.76847797905721,
29.0159676801844));
#21688=CARTESIAN_POINT('Ctrl Pts',(-0.944228247774239,-1.7572799951707,
29.0144947471362));
#21689=CARTESIAN_POINT('Ctrl Pts',(-1.04221221354983,-1.70310654137577,
29.007677939762));
#21690=CARTESIAN_POINT('Ctrl Pts',(-1.1163609292893,-1.65545136752319,29.0025431818502));
#21691=CARTESIAN_POINT('Ctrl Pts',(-1.31824026067784,-1.50595140882999,
28.9879573301493));
#21692=CARTESIAN_POINT('Ctrl Pts',(-1.43693250606842,-1.39314924625441,
28.9785636495392));
#21693=CARTESIAN_POINT('Ctrl Pts',(-1.55383371680727,-1.25102550456506,
28.9671751700723));
#21694=CARTESIAN_POINT('Ctrl Pts',(-1.56685051354219,-1.23468354204676,
28.9658726103616));
#21695=CARTESIAN_POINT('Ctrl Pts',(-1.58437523995888,-1.21195858301741,
28.9640692189897));
#21696=CARTESIAN_POINT('Ctrl Pts',(-1.58910622951228,-1.20574868711128,
28.9635772177295));
#21697=CARTESIAN_POINT('Ctrl Pts',(-1.59658100181716,-1.19581689488158,
28.9627915283571));
#21698=CARTESIAN_POINT('Ctrl Pts',(-1.59934854018609,-1.19211290902519,
28.9624987731733));
#21699=CARTESIAN_POINT('Ctrl Pts',(-1.60499926881264,-1.18449505725215,
28.9618971913992));
#21700=CARTESIAN_POINT('Ctrl Pts',(-1.60788107797538,-1.18058020987352,
28.9615883137886));
#21701=CARTESIAN_POINT('Ctrl Pts',(-1.61450359065645,-1.17151450795343,
28.9608736566693));
#21702=CARTESIAN_POINT('Ctrl Pts',(-1.61823398907472,-1.16635622416048,
28.9604674821747));
#21703=CARTESIAN_POINT('Ctrl Pts',(-1.62987545786151,-1.15009538984348,
28.9591884390637));
#21704=CARTESIAN_POINT('Ctrl Pts',(-1.63769730572518,-1.13892973152651,
28.9583121625329));
#21705=CARTESIAN_POINT('Ctrl Pts',(-1.71507399433766,-1.02602949122731,
28.9494700392553));
#21706=CARTESIAN_POINT('Ctrl Pts',(-1.77516054061037,-0.918155869470301,
28.941143523288));
#21707=CARTESIAN_POINT('Ctrl Pts',(-1.85838563392994,-0.729592615704861,
28.926872576684));
#21708=CARTESIAN_POINT('Ctrl Pts',(-1.88710310707098,-0.65172383881565,
28.9210596919052));
#21709=CARTESIAN_POINT('Ctrl Pts',(-1.91766546543442,-0.549676532124244,
28.9136608865835));
#21710=CARTESIAN_POINT('Ctrl Pts',(-1.92403797609486,-0.526937415471637,
28.9120261167439));
#21711=CARTESIAN_POINT('Ctrl Pts',(-1.93382961471452,-0.489448252179756,
28.9093583934285));
#21712=CARTESIAN_POINT('Ctrl Pts',(-1.9374871849228,-0.474763094905207,
28.9083202475327));
#21713=CARTESIAN_POINT('Ctrl Pts',(-1.95275747153124,-0.41033512349148,
28.9037991070087));
#21714=CARTESIAN_POINT('Ctrl Pts',(-1.96262537178659,-0.360193481078364,
28.9003671221817));
#21715=CARTESIAN_POINT('Ctrl Pts',(-1.97167414499397,-0.302622375618298,
28.8965648626167));
#21716=CARTESIAN_POINT('Ctrl Pts',(-1.97275191725003,-0.295514996350605,
28.8960978494781));
#21717=CARTESIAN_POINT('Ctrl Pts',(-1.97429258291513,-0.284970844872324,
28.8954087084629));
#21718=CARTESIAN_POINT('Ctrl Pts',(-1.97478495940073,-0.2815385407945,28.8951849607858));
#21719=CARTESIAN_POINT('Ctrl Pts',(-1.97564471693772,-0.275432026133444,
28.8947879362226));
#21720=CARTESIAN_POINT('Ctrl Pts',(-1.97601562117872,-0.272758343161151,
28.8946144617332));
#21721=CARTESIAN_POINT('Ctrl Pts',(-1.9767239862926,-0.267574770195167,
28.894278840156));
#21722=CARTESIAN_POINT('Ctrl Pts',(-1.97706209261052,-0.265065006682137,
28.8941166562815));
#21723=CARTESIAN_POINT('Ctrl Pts',(-1.97779457991747,-0.25954837468441,
28.8937608461641));
#21724=CARTESIAN_POINT('Ctrl Pts',(-1.9781868862003,-0.256541230041903,
28.893567336597));
#21725=CARTESIAN_POINT('Ctrl Pts',(-1.97913716695173,-0.249125241262451,
28.8930911874896));
#21726=CARTESIAN_POINT('Ctrl Pts',(-1.97968727218915,-0.244715378902829,
28.892808980054));
#21727=CARTESIAN_POINT('Ctrl Pts',(-1.9823636691879,-0.22266052620991,28.8914020755545));
#21728=CARTESIAN_POINT('Ctrl Pts',(-1.98426889701555,-0.204988836130511,
28.8902891269955));
#21729=CARTESIAN_POINT('Ctrl Pts',(-1.99176151272927,-0.125541967397613,
28.8853404638821));
#21730=CARTESIAN_POINT('Ctrl Pts',(-1.99470237642068,-0.063547662994927,
28.8816269784329));
#21731=CARTESIAN_POINT('Ctrl Pts',(-1.99474942627385,-0.00151290453868526,
28.8779715341069));
#21732=CARTESIAN_POINT('',(-1.99456009906478,-0.000760494884442119,28.0790451186048));
#21733=CARTESIAN_POINT('Ctrl Pts',(-1.99474985500375,-0.000760567235443675,
28.0790451186048));
#21734=CARTESIAN_POINT('Ctrl Pts',(-1.99472090390775,-0.0766909937140657,
28.0838673953792));
#21735=CARTESIAN_POINT('Ctrl Pts',(-1.99035228629733,-0.152487659476892,
28.0886896721536));
#21736=CARTESIAN_POINT('Ctrl Pts',(-1.98171477759731,-0.227671040653933,
28.093511948928));
#21737=CARTESIAN_POINT('Ctrl Pts',(-1.97305323617513,-0.30306360961574,
28.0983476430478));
#21738=CARTESIAN_POINT('Ctrl Pts',(-1.96009914796827,-0.377839146982171,
28.1031833371677));
#21739=CARTESIAN_POINT('Ctrl Pts',(-1.9429741886226,-0.451529472843513,
28.1080190312875));
#21740=CARTESIAN_POINT('Ctrl Pts',(-1.92577546389587,-0.525537218142682,
28.1128755550521));
#21741=CARTESIAN_POINT('Ctrl Pts',(-1.90437000772297,-0.598450062555347,
28.1177320788166));
#21742=CARTESIAN_POINT('Ctrl Pts',(-1.87892964315567,-0.669814122403307,
28.1225886025812));
#21743=CARTESIAN_POINT('Ctrl Pts',(-1.85974397604313,-0.72363281247828,
28.1262511148862));
#21744=CARTESIAN_POINT('Ctrl Pts',(-1.83826454851322,-0.776571052191794,
28.1299136271912));
#21745=CARTESIAN_POINT('Ctrl Pts',(-1.81458234810635,-0.828443398453306,
28.1335761394962));
#21746=CARTESIAN_POINT('Ctrl Pts',(-1.78578205236523,-0.891526173172308,
28.1380301782142));
#21747=CARTESIAN_POINT('Ctrl Pts',(-1.75363125164456,-0.95323025320993,
28.1424842169322));
#21748=CARTESIAN_POINT('Ctrl Pts',(-1.71828444602139,-1.0131762556737,28.1469382556501));
#21749=CARTESIAN_POINT('Ctrl Pts',(-1.682990772139,-1.07303214998177,28.1513855992559));
#21750=CARTESIAN_POINT('Ctrl Pts',(-1.64451087491594,-1.13113479347519,
28.1558329428617));
#21751=CARTESIAN_POINT('Ctrl Pts',(-1.60304648564627,-1.18712658438649,
28.1602802864674));
#21752=CARTESIAN_POINT('Ctrl Pts',(-1.5616309786294,-1.24305236673174,28.1647223871122));
#21753=CARTESIAN_POINT('Ctrl Pts',(-1.51723825751373,-1.29687184739755,
28.169164487757));
#21754=CARTESIAN_POINT('Ctrl Pts',(-1.4701140003193,-1.34825531282661,28.1736065884018));
#21755=CARTESIAN_POINT('Ctrl Pts',(-1.42301946931509,-1.39960636533803,
28.1780458869498));
#21756=CARTESIAN_POINT('Ctrl Pts',(-1.37319715052399,-1.44852409100623,
28.1824851854978));
#21757=CARTESIAN_POINT('Ctrl Pts',(-1.3209327762968,-1.49471206692287,28.1869244840459));
#21758=CARTESIAN_POINT('Ctrl Pts',(-1.2686836111094,-1.54088660204405,28.1913624907489));
#21759=CARTESIAN_POINT('Ctrl Pts',(-1.21399416787632,-1.58433264032543,
28.195800497452));
#21760=CARTESIAN_POINT('Ctrl Pts',(-1.15718548899295,-1.6247920810258,28.2002385041551));
#21761=CARTESIAN_POINT('Ctrl Pts',(-1.10037403838995,-1.66525349575951,
28.2046767273904));
#21762=CARTESIAN_POINT('Ctrl Pts',(-1.04144354700391,-1.70272774155636,
28.2091149506257));
#21763=CARTESIAN_POINT('Ctrl Pts',(-0.980744981797496,-1.73699937915332,
28.213553173861));
#21764=CARTESIAN_POINT('Ctrl Pts',(-0.919982113159806,-1.77130732376818,
28.217996098904));
#21765=CARTESIAN_POINT('Ctrl Pts',(-0.857447859277962,-1.80240564711765,
28.222439023947));
#21766=CARTESIAN_POINT('Ctrl Pts',(-0.793517948224323,-1.83012481223163,
28.2268819489901));
#21767=CARTESIAN_POINT('Ctrl Pts',(-0.729550718650175,-1.85786015816324,
28.2313274675513));
#21768=CARTESIAN_POINT('Ctrl Pts',(-0.664186669228553,-1.88221224874948,
28.2357729861126));
#21769=CARTESIAN_POINT('Ctrl Pts',(-0.597819046438306,-1.90306067959369,
28.2402185046738));
#21770=CARTESIAN_POINT('Ctrl Pts',(-0.531335610293624,-1.92394549153171,
28.2446717807891));
#21771=CARTESIAN_POINT('Ctrl Pts',(-0.463845579006982,-1.94131431711732,
28.2491250569043));
#21772=CARTESIAN_POINT('Ctrl Pts',(-0.395754024367098,-1.95509752050818,
28.2535783330196));
#21773=CARTESIAN_POINT('Ctrl Pts',(-0.359292954951652,-1.96247802956337,
28.2559629343174));
#21774=CARTESIAN_POINT('Ctrl Pts',(-0.322659533583422,-1.96883132014021,
28.2583475356152));
#21775=CARTESIAN_POINT('Ctrl Pts',(-0.285916359981321,-1.97415283035408,
28.260732136913));
#21776=CARTESIAN_POINT('Ctrl Pts',(-0.217286221267569,-1.98409252658445,
28.265186175631));
#21777=CARTESIAN_POINT('Ctrl Pts',(-0.148001227391612,-1.99046881891421,
28.2696402143489));
#21778=CARTESIAN_POINT('Ctrl Pts',(-0.0784639955463822,-1.99320620205309,
28.2740942530669));
#21779=CARTESIAN_POINT('Ctrl Pts',(-0.00903128896481908,-1.9959394704798,
28.2785415966727));
#21780=CARTESIAN_POINT('Ctrl Pts',(0.0606524178666762,-1.99504466690194,
28.2829889402785));
#21781=CARTESIAN_POINT('Ctrl Pts',(0.130177248859435,-1.99049778858942,
28.2874362838842));
#21782=CARTESIAN_POINT('Ctrl Pts',(0.199620117222928,-1.98595627057906,
28.291878384529));
#21783=CARTESIAN_POINT('Ctrl Pts',(0.268903995586189,-1.97777126073603,
28.2963204851738));
#21784=CARTESIAN_POINT('Ctrl Pts',(0.337618661805003,-1.96597080387807,
28.3007625858186));
#21785=CARTESIAN_POINT('Ctrl Pts',(0.406289982507969,-1.95417779080057,
28.3052018843666));
#21786=CARTESIAN_POINT('Ctrl Pts',(0.474392321983942,-1.93877393764083,
28.3096411829146));
#21787=CARTESIAN_POINT('Ctrl Pts',(0.541521761563122,-1.9198389891482,28.3140804814626));
#21788=CARTESIAN_POINT('Ctrl Pts',(0.608631666338052,-1.90090955076432,
28.3185184881657));
#21789=CARTESIAN_POINT('Ctrl Pts',(0.674768762310941,-1.87845118974319,
28.3229564948688));
#21790=CARTESIAN_POINT('Ctrl Pts',(0.739542233185855,-1.85259408609508,
28.3273945015718));
#21791=CARTESIAN_POINT('Ctrl Pts',(0.804318864386049,-1.82673572086786,
28.3318327248071));
#21792=CARTESIAN_POINT('Ctrl Pts',(0.867731284613089,-1.79747846751092,
28.3362709480424));
#21793=CARTESIAN_POINT('Ctrl Pts',(0.929408344014541,-1.76500076276928,
28.3407091712778));
#21794=CARTESIAN_POINT('Ctrl Pts',(0.991150743453881,-1.73248865148364,
28.3451520963208));
#21795=CARTESIAN_POINT('Ctrl Pts',(1.05115367862411,-1.69674950775209,28.3495950213638));
#21796=CARTESIAN_POINT('Ctrl Pts',(1.10907118641276,-1.65800743845406,28.3540379464068));
#21797=CARTESIAN_POINT('Ctrl Pts',(1.16702250303466,-1.61924275381551,28.3584834649681));
#21798=CARTESIAN_POINT('Ctrl Pts',(1.22288557708541,-1.57747194785833,28.3629289835293));
#21799=CARTESIAN_POINT('Ctrl Pts',(1.2763462693605,-1.5329604571513,28.3673745020906));
#21800=CARTESIAN_POINT('Ctrl Pts',(1.32990025203595,-1.48837129265046,28.3718277782058));
#21801=CARTESIAN_POINT('Ctrl Pts',(1.3810431252692,-1.44103222904822,28.3762810543211));
#21802=CARTESIAN_POINT('Ctrl Pts',(1.42949703153687,-1.39124613182833,28.3807343304363));
#21803=CARTESIAN_POINT('Ctrl Pts',(1.45544270496476,-1.36458710845505,28.3831189317341));
#21804=CARTESIAN_POINT('Ctrl Pts',(1.48061805011818,-1.33722703062777,28.3855035330319));
#21805=CARTESIAN_POINT('Ctrl Pts',(1.50498533932892,-1.30921605967274,28.3878881343298));
#21806=CARTESIAN_POINT('Ctrl Pts',(1.55049938383449,-1.25689622353235,28.3923421730477));
#21807=CARTESIAN_POINT('Ctrl Pts',(1.59337201604558,-1.20209654390236,28.3967962117657));
#21808=CARTESIAN_POINT('Ctrl Pts',(1.63332177260354,-1.145114644758,28.4012502504837));
#21809=CARTESIAN_POINT('Ctrl Pts',(1.67321147847031,-1.08821839826146,28.4056975940895));
#21810=CARTESIAN_POINT('Ctrl Pts',(1.71018675001396,-1.02914684025344,28.4101449376952));
#21811=CARTESIAN_POINT('Ctrl Pts',(1.74400549498859,-0.968231581776595,
28.414592281301));
#21812=CARTESIAN_POINT('Ctrl Pts',(1.77778437113911,-0.907388136128027,
28.4190343819458));
#21813=CARTESIAN_POINT('Ctrl Pts',(1.80841387505166,-0.844705732877582,
28.4234764825906));
#21814=CARTESIAN_POINT('Ctrl Pts',(1.83569548648917,-0.780544453175667,
28.4279185832353));
#21815=CARTESIAN_POINT('Ctrl Pts',(1.86295988856532,-0.716423646693214,
28.4323578817834));
#21816=CARTESIAN_POINT('Ctrl Pts',(1.8868803965012,-0.650826263861637,28.4367971803314));
#21817=CARTESIAN_POINT('Ctrl Pts',(1.90730536994191,-0.58413507709326,28.4412364788794));
#21818=CARTESIAN_POINT('Ctrl Pts',(1.92772439967357,-0.51746329759665,28.4456744855825));
#21819=CARTESIAN_POINT('Ctrl Pts',(1.94464977094004,-0.449698813897798,
28.4501124922855));
#21820=CARTESIAN_POINT('Ctrl Pts',(1.9579793409919,-0.381240688737356,28.4545504989886));
#21821=CARTESIAN_POINT('Ctrl Pts',(1.97130956139916,-0.312779223475779,
28.4589887222239));
#21822=CARTESIAN_POINT('Ctrl Pts',(1.98104354105954,-0.243624530554679,
28.4634269454592));
#21823=CARTESIAN_POINT('Ctrl Pts',(1.98713035708185,-0.174185264772244,
28.4678651686945));
#21824=CARTESIAN_POINT('Ctrl Pts',(1.993223621414,-0.104672435750919,28.4723080937375));
#21825=CARTESIAN_POINT('Ctrl Pts',(1.99566196737844,-0.0348749208047779,
28.4767510187806));
#21826=CARTESIAN_POINT('Ctrl Pts',(1.9944465059925,0.0347950748572986,28.4811939438236));
#21827=CARTESIAN_POINT('Ctrl Pts',(1.99323033509171,0.104505739763558,28.4856394623848));
#21828=CARTESIAN_POINT('Ctrl Pts',(1.98835614581087,0.174088248712013,28.4900849809461));
#21829=CARTESIAN_POINT('Ctrl Pts',(1.97987702725532,0.24313477630037,28.4945304995074));
#21830=CARTESIAN_POINT('Ctrl Pts',(1.9713831124012,0.312301792006778,28.4989837756226));
#21831=CARTESIAN_POINT('Ctrl Pts',(1.95927179597492,0.380930477260881,28.5034370517378));
#21832=CARTESIAN_POINT('Ctrl Pts',(1.94364727905563,0.448623246298778,28.5078903278531));
#21833=CARTESIAN_POINT('Ctrl Pts',(1.93528079955626,0.484870777492008,28.5102749291509));
#21834=CARTESIAN_POINT('Ctrl Pts',(1.92590783839721,0.520850208579681,28.5126595304487));
#21835=CARTESIAN_POINT('Ctrl Pts',(1.91555014288437,0.556502661804665,28.5150441317464));
#21836=CARTESIAN_POINT('Ctrl Pts',(1.89620368992137,0.62309551621691,28.5194981704644));
#21837=CARTESIAN_POINT('Ctrl Pts',(1.87334219798095,0.688810200013788,28.5239522091824));
#21838=CARTESIAN_POINT('Ctrl Pts',(1.84706350906263,0.753248933613074,28.5284062479004));
#21839=CARTESIAN_POINT('Ctrl Pts',(1.82082432109675,0.817590805783743,28.5328535915062));
#21840=CARTESIAN_POINT('Ctrl Pts',(1.79117831434442,0.880660084793923,28.5373009351119));
#21841=CARTESIAN_POINT('Ctrl Pts',(1.75827322167461,0.942073691619719,28.5417482787177));
#21842=CARTESIAN_POINT('Ctrl Pts',(1.72540692072673,1.00341489811577,28.5461903793625));
#21843=CARTESIAN_POINT('Ctrl Pts',(1.68928939490203,1.06310387964073,28.5506324800073));
#21844=CARTESIAN_POINT('Ctrl Pts',(1.65011590392848,1.12077877661129,28.555074580652));
#21845=CARTESIAN_POINT('Ctrl Pts',(1.61096712376658,1.17841729200133,28.5595138792001));
#21846=CARTESIAN_POINT('Ctrl Pts',(1.56876647703001,1.23404383916435,28.5639531777481));
#21847=CARTESIAN_POINT('Ctrl Pts',(1.52375368261948,1.28732368781265,28.5683924762961));
#21848=CARTESIAN_POINT('Ctrl Pts',(1.47875398702419,1.34058803191603,28.5728304829992));
#21849=CARTESIAN_POINT('Ctrl Pts',(1.43094408406991,1.39150665938169,28.5772684897022));
#21850=CARTESIAN_POINT('Ctrl Pts',(1.38060418746342,1.43977763562936,28.5817064964053));
#21851=CARTESIAN_POINT('Ctrl Pts',(1.3302618347519,1.48805096703855,28.5861447196406));
#21852=CARTESIAN_POINT('Ctrl Pts',(1.2773895983274,1.53367605365235,28.5905829428759));
#21853=CARTESIAN_POINT('Ctrl Pts',(1.22230348752928,1.57638883111806,28.5950211661112));
#21854=CARTESIAN_POINT('Ctrl Pts',(1.16715901907598,1.61914685805777,28.5994640911542));
#21855=CARTESIAN_POINT('Ctrl Pts',(1.1097963826876,1.65898611721601,28.6039070161973));
#21856=CARTESIAN_POINT('Ctrl Pts',(1.05056274451245,1.69568436990569,28.6083499412403));
#21857=CARTESIAN_POINT('Ctrl Pts',(0.991294529224582,1.73240404487601,28.6127954598015));
#21858=CARTESIAN_POINT('Ctrl Pts',(0.930153567536852,1.76597882822019,28.6172409783628));
#21859=CARTESIAN_POINT('Ctrl Pts',(0.867511484794862,1.79623255349885,28.6216864969241));
#21860=CARTESIAN_POINT('Ctrl Pts',(0.804760089869839,1.82653907237266,28.6261397730393));
#21861=CARTESIAN_POINT('Ctrl Pts',(0.740502796257915,1.85351277517669,28.6305930491545));
#21862=CARTESIAN_POINT('Ctrl Pts',(0.675130292879802,1.87702601210959,28.6350463252698));
#21863=CARTESIAN_POINT('Ctrl Pts',(0.640125197223682,1.88961667432212,28.6374309265676));
#21864=CARTESIAN_POINT('Ctrl Pts',(0.604800587654434,1.90121597693428,28.6398155278654));
#21865=CARTESIAN_POINT('Ctrl Pts',(0.56921774033835,1.91181032704191,28.6422001291632));
#21866=CARTESIAN_POINT('Ctrl Pts',(0.502754898190598,1.9315988114374,28.6466541678812));
#21867=CARTESIAN_POINT('Ctrl Pts',(0.435127300851099,1.94795654839455,28.6511082065992));
#21868=CARTESIAN_POINT('Ctrl Pts',(0.366722357313723,1.96075043673239,28.6555622453172));
#21869=CARTESIAN_POINT('Ctrl Pts',(0.298420237034797,1.97352509386824,28.6600095889229));
#21870=CARTESIAN_POINT('Ctrl Pts',(0.229343566979604,1.982746445467,28.6644569325287));
#21871=CARTESIAN_POINT('Ctrl Pts',(0.159894408044754,1.98833129552799,28.6689042761344));
#21872=CARTESIAN_POINT('Ctrl Pts',(0.0905271225295731,1.99390956162483,
28.6733463767792));
#21873=CARTESIAN_POINT('Ctrl Pts',(0.0207887059247658,1.99585980177506,
28.677788477424));
#21874=CARTESIAN_POINT('Ctrl Pts',(-0.0489108896728576,1.99415026699881,
28.6822305780688));
#21875=CARTESIAN_POINT('Ctrl Pts',(-0.118566518456798,1.99244181060466,
28.6866698766168));
#21876=CARTESIAN_POINT('Ctrl Pts',(-0.18818288653511,1.98707817099578,28.6911091751649));
#21877=CARTESIAN_POINT('Ctrl Pts',(-0.257348780247559,1.97807966669826,
28.6955484737129));
#21878=CARTESIAN_POINT('Ctrl Pts',(-0.326494546543439,1.96908378098389,
28.6999864804159));
#21879=CARTESIAN_POINT('Ctrl Pts',(-0.395189613484428,1.95645519351512,
28.704424487119));
#21880=CARTESIAN_POINT('Ctrl Pts',(-0.463028416280303,1.94026602511536,
28.7088624938221));
#21881=CARTESIAN_POINT('Ctrl Pts',(-0.530870528960365,1.92407606683915,
28.7133007170574));
#21882=CARTESIAN_POINT('Ctrl Pts',(-0.597855818918246,1.90432529869434,
28.7177389402927));
#21883=CARTESIAN_POINT('Ctrl Pts',(-0.663591180862934,1.88113644034157,
28.722177163528));
#21884=CARTESIAN_POINT('Ctrl Pts',(-0.729396182169134,1.85792301595246,
28.726620088571));
#21885=CARTESIAN_POINT('Ctrl Pts',(-0.793948149902581,1.83126439473065,
28.7310630136141));
#21886=CARTESIAN_POINT('Ctrl Pts',(-0.856872275349802,1.80133213656917,
28.7355059386571));
#21887=CARTESIAN_POINT('Ctrl Pts',(-0.919833132199041,1.77138240571657,
28.7399514572184));
#21888=CARTESIAN_POINT('Ctrl Pts',(-0.981163824840807,1.73815546765738,
28.7443969757796));
#21889=CARTESIAN_POINT('Ctrl Pts',(-1.04051503765132,1.70186839059942,28.7488424943409));
#21890=CARTESIAN_POINT('Ctrl Pts',(-1.09996981998501,1.66551799157902,28.7532957704561));
#21891=CARTESIAN_POINT('Ctrl Pts',(-1.15743782352383,1.62609707080648,28.7577490465713));
#21892=CARTESIAN_POINT('Ctrl Pts',(-1.21260020212703,1.58386499181638,28.7622023226866));
#21893=CARTESIAN_POINT('Ctrl Pts',(-1.2421380695763,1.56125092797605,28.7645869239844));
#21894=CARTESIAN_POINT('Ctrl Pts',(-1.27101543260124,1.53783149657783,28.7669715252822));
#21895=CARTESIAN_POINT('Ctrl Pts',(-1.29918768722305,1.51365085666016,28.76935612658));
#21896=CARTESIAN_POINT('Ctrl Pts',(-1.35318319536139,1.46730575730648,28.7739265012451));
#21897=CARTESIAN_POINT('Ctrl Pts',(-1.40482250508354,1.41795863007694,28.7784968759102));
#21898=CARTESIAN_POINT('Ctrl Pts',(-1.45374853911666,1.36588533468816,28.7830672505753));
#21899=CARTESIAN_POINT('Ctrl Pts',(-1.50065853549726,1.31595776245616,28.7874492991765));
#21900=CARTESIAN_POINT('Ctrl Pts',(-1.54507405645156,1.26352467347088,28.7918313477777));
#21901=CARTESIAN_POINT('Ctrl Pts',(-1.58671329490916,1.20887074671302,28.7962133963789));
#21902=CARTESIAN_POINT('Ctrl Pts',(-1.62831315497145,1.15426850639357,28.8005913008591));
#21903=CARTESIAN_POINT('Ctrl Pts',(-1.66714163101419,1.0974499897678,28.8049692053393));
#21904=CARTESIAN_POINT('Ctrl Pts',(-1.70295563913342,1.03873464062949,28.8093471098196));
#21905=CARTESIAN_POINT('Ctrl Pts',(-1.73874877114827,0.980053516863378,
28.8137224624047));
#21906=CARTESIAN_POINT('Ctrl Pts',(-1.77153065696791,0.919478183176294,
28.8180978149899));
#21907=CARTESIAN_POINT('Ctrl Pts',(-1.8011013554795,0.857357259134092,28.822473167575));
#21908=CARTESIAN_POINT('Ctrl Pts',(-1.83066554242213,0.795250014331845,
28.8268475566925));
#21909=CARTESIAN_POINT('Ctrl Pts',(-1.85701973001042,0.73159831112045,28.8312219458101));
#21910=CARTESIAN_POINT('Ctrl Pts',(-1.88001071204681,0.666773788543948,
28.8355963349276));
#21911=CARTESIAN_POINT('Ctrl Pts',(-1.90301678880371,0.601906705451793,
28.8399735960487));
#21912=CARTESIAN_POINT('Ctrl Pts',(-1.9226550823902,0.535865742243995,28.8443508571697));
#21913=CARTESIAN_POINT('Ctrl Pts',(-1.93882166625638,0.4690395601171,28.8487281182908));
#21914=CARTESIAN_POINT('Ctrl Pts',(-1.95499461229697,0.402187079309592,
28.8531071020329));
#21915=CARTESIAN_POINT('Ctrl Pts',(-1.96769303523254,0.334549260828964,
28.8574860857751));
#21916=CARTESIAN_POINT('Ctrl Pts',(-1.97686429343349,0.266524159970012,
28.8618650695173));
#21917=CARTESIAN_POINT('Ctrl Pts',(-1.98604794688615,0.198407120989854,
28.8662499715974));
#21918=CARTESIAN_POINT('Ctrl Pts',(-1.99169488580679,0.129902258227077,
28.8706348736776));
#21919=CARTESIAN_POINT('Ctrl Pts',(-1.99380447786887,0.0614106385737057,
28.8750197757577));
#21920=CARTESIAN_POINT('Ctrl Pts',(-1.99445001346885,0.0404521890321277,
28.8763615566859));
#21921=CARTESIAN_POINT('Ctrl Pts',(-1.99476469430693,0.0194949600558917,
28.8777033376141));
#21922=CARTESIAN_POINT('Ctrl Pts',(-1.99474947325114,-0.00144964281222297,
28.8790451185423));
#21923=CARTESIAN_POINT('',(-1.99382862437974,0.00178311505610039,27.2790451186048));
#21924=CARTESIAN_POINT('Ctrl Pts',(-1.99382862437974,0.00178311505610039,
27.2790451186048));
#21925=CARTESIAN_POINT('Ctrl Pts',(-1.9897025744846,-0.476968105037969,
27.3095767974018));
#21926=CARTESIAN_POINT('Ctrl Pts',(-1.57649467124548,-1.62673224728373,
27.3824938086711));
#21927=CARTESIAN_POINT('Ctrl Pts',(0.346093998518022,-2.33304570413791,
27.4977961524125));
#21928=CARTESIAN_POINT('Ctrl Pts',(2.1489051180945,-0.97215744961082,27.6249521498293));
#21929=CARTESIAN_POINT('Ctrl Pts',(1.98079137716424,1.28037058446309,27.752108147246));
#21930=CARTESIAN_POINT('Ctrl Pts',(-0.00405728419479211,2.35857305416888,
27.8792641446628));
#21931=CARTESIAN_POINT('Ctrl Pts',(-1.70198164629091,1.42865299045872,27.9882431351157));
#21932=CARTESIAN_POINT('Ctrl Pts',(-1.99043493990472,0.379843564099569,
28.0548367930963));
#21933=CARTESIAN_POINT('Ctrl Pts',(-1.99173494636544,-0.000759417697459401,
28.0790451186048));
#21934=CARTESIAN_POINT('',(-1.99474927319053,-0.00170282290822489,25.6790451186048));
#21935=CARTESIAN_POINT('Ctrl Pts',(-1.99474916919083,0.00182058025913,27.2795743230551));
#21936=CARTESIAN_POINT('Ctrl Pts',(-1.99460679985945,0.157809916119892,
27.2687736719809));
#21937=CARTESIAN_POINT('Ctrl Pts',(-1.97616814764425,0.31325218485814,27.257698223344));
#21938=CARTESIAN_POINT('Ctrl Pts',(-1.9366719416301,0.478026890473197,27.2464400873559));
#21939=CARTESIAN_POINT('Ctrl Pts',(-1.93340965083876,0.49105504968079,27.2455536757105));
#21940=CARTESIAN_POINT('Ctrl Pts',(-1.92837363507333,0.510338051726765,
27.2442482324704));
#21941=CARTESIAN_POINT('Ctrl Pts',(-1.92670058705654,0.516618480185472,
27.2438240871158));
#21942=CARTESIAN_POINT('Ctrl Pts',(-1.92359632482327,0.528046671149623,
27.2430543177036));
#21943=CARTESIAN_POINT('Ctrl Pts',(-1.92217507498526,0.533197046587033,
27.2427081563871));
#21944=CARTESIAN_POINT('Ctrl Pts',(-1.91990197759731,0.541307161942427,
27.2421643244256));
#21945=CARTESIAN_POINT('Ctrl Pts',(-1.91906395256792,0.544270698662273,
27.2419658665239));
#21946=CARTESIAN_POINT('Ctrl Pts',(-1.91747880769462,0.549827123364246,
27.2415942849693));
#21947=CARTESIAN_POINT('Ctrl Pts',(-1.916733298736,0.552420406188063,27.2414210732377));
#21948=CARTESIAN_POINT('Ctrl Pts',(-1.91502036904709,0.558333687439218,
27.2410265859094));
#21949=CARTESIAN_POINT('Ctrl Pts',(-1.91404957783869,0.56165268130021,27.2408055095512));
#21950=CARTESIAN_POINT('Ctrl Pts',(-1.91104766060861,0.57181762234811,27.2401294254953));
#21951=CARTESIAN_POINT('Ctrl Pts',(-1.90898837277144,0.578655295219941,
27.2396760308093));
#21952=CARTESIAN_POINT('Ctrl Pts',(-1.89229171892375,0.633035665688997,
27.2360801415041));
#21953=CARTESIAN_POINT('Ctrl Pts',(-1.87591589196118,0.680031342406879,
27.233033363773));
#21954=CARTESIAN_POINT('Ctrl Pts',(-1.85116402537216,0.743337907443125,
27.2289504846696));
#21955=CARTESIAN_POINT('Ctrl Pts',(-1.84429744256836,0.760214751048216,
27.2278641730061));
#21956=CARTESIAN_POINT('Ctrl Pts',(-1.80294357986268,0.857995667637109,
27.2215701409892));
#21957=CARTESIAN_POINT('Ctrl Pts',(-1.76336597820338,0.93664501430885,27.2165031169297));
#21958=CARTESIAN_POINT('Ctrl Pts',(-1.68864944448531,1.06348579843691,27.2079559484914));
#21959=CARTESIAN_POINT('Ctrl Pts',(-1.65631440973545,1.11317614552078,27.2045027073776));
#21960=CARTESIAN_POINT('Ctrl Pts',(-1.57672341043266,1.22432420945706,27.1964089487888));
#21961=CARTESIAN_POINT('Ctrl Pts',(-1.5280056341374,1.2846101233949,27.1917349277779));
#21962=CARTESIAN_POINT('Ctrl Pts',(-1.46531419190174,1.35356196891362,27.1859368631662));
#21963=CARTESIAN_POINT('Ctrl Pts',(-1.45458015558808,1.36509055859065,27.1849512328303));
#21964=CARTESIAN_POINT('Ctrl Pts',(-1.44005880385412,1.38032105497168,27.1836266436172));
#21965=CARTESIAN_POINT('Ctrl Pts',(-1.43639145787625,1.38413697018114,27.1832928559376));
#21966=CARTESIAN_POINT('Ctrl Pts',(-1.42956740734128,1.39118114440309,27.1826730875579));
#21967=CARTESIAN_POINT('Ctrl Pts',(-1.42641483695275,1.39441337524033,27.1823872877461));
#21968=CARTESIAN_POINT('Ctrl Pts',(-1.41986715172456,1.40108106942304,27.1817947560018));
#21969=CARTESIAN_POINT('Ctrl Pts',(-1.41647048159474,1.40451495746349,27.1814879567318));
#21970=CARTESIAN_POINT('Ctrl Pts',(-1.40874079147721,1.41227278397408,27.1807910766158));
#21971=CARTESIAN_POINT('Ctrl Pts',(-1.40440028780705,1.41658916562026,27.1804006654354));
#21972=CARTESIAN_POINT('Ctrl Pts',(-1.39316664946732,1.42765799821397,27.1793925385091));
#21973=CARTESIAN_POINT('Ctrl Pts',(-1.38624432530855,1.43438047189903,27.1787735191574));
#21974=CARTESIAN_POINT('Ctrl Pts',(-1.34363916263484,1.47515912622825,27.1749766115967));
#21975=CARTESIAN_POINT('Ctrl Pts',(-1.3067548080363,1.50792964144487,27.1717440914835));
#21976=CARTESIAN_POINT('Ctrl Pts',(-1.23917019810692,1.56363321087344,27.1659089241363));
#21977=CARTESIAN_POINT('Ctrl Pts',(-1.20895134501141,1.58711308664897,27.1633289037337));
#21978=CARTESIAN_POINT('Ctrl Pts',(-1.10163276113008,1.66565502008231,27.1542712093847));
#21979=CARTESIAN_POINT('Ctrl Pts',(-1.02130482323748,1.71608140769274,27.1476655744769));
#21980=CARTESIAN_POINT('Ctrl Pts',(-0.872022788501079,1.79558954503728,
27.1358663647506));
#21981=CARTESIAN_POINT('Ctrl Pts',(-0.804430309719816,1.82687127517369,
27.1306847785493));
#21982=CARTESIAN_POINT('Ctrl Pts',(-0.707129944025984,1.86545155570333,
27.1235715257642));
#21983=CARTESIAN_POINT('Ctrl Pts',(-0.678763766444861,1.87595901448863,
27.1215378019557));
#21984=CARTESIAN_POINT('Ctrl Pts',(-0.633669838145158,1.89150591951069,
27.1183788083664));
#21985=CARTESIAN_POINT('Ctrl Pts',(-0.617096991088353,1.89697745426736,
27.1172333335376));
#21986=CARTESIAN_POINT('Ctrl Pts',(-0.595738540309857,1.90371941289554,
27.1157788054274));
#21987=CARTESIAN_POINT('Ctrl Pts',(-0.591017709481509,1.90519030015296,
27.1154586657663));
#21988=CARTESIAN_POINT('Ctrl Pts',(-0.583432496204787,1.90752274718303,
27.1149465036827));
#21989=CARTESIAN_POINT('Ctrl Pts',(-0.580571598435654,1.90839543282521,
27.1147538390233));
#21990=CARTESIAN_POINT('Ctrl Pts',(-0.57510695190225,1.91004893794979,27.1143868076051));
#21991=CARTESIAN_POINT('Ctrl Pts',(-0.572503601830494,1.91083086050498,
27.1142123801221));
#21992=CARTESIAN_POINT('Ctrl Pts',(-0.566490368498008,1.91262355770618,
27.1138104559202));
#21993=CARTESIAN_POINT('Ctrl Pts',(-0.563079375545609,1.9136305360251,27.1135831827497));
#21994=CARTESIAN_POINT('Ctrl Pts',(-0.552127353515837,1.91683192529738,
27.1128556991488));
#21995=CARTESIAN_POINT('Ctrl Pts',(-0.544575933696427,1.9189909592504,27.112357509485));
#21996=CARTESIAN_POINT('Ctrl Pts',(-0.443617997709538,1.94721200556986,
27.1057400168433));
#21997=CARTESIAN_POINT('Ctrl Pts',(-0.348430252232567,1.9664774098224,27.0999883637565));
#21998=CARTESIAN_POINT('Ctrl Pts',(-0.0721855841925019,2.00168696613813,
27.0837221410369));
#21999=CARTESIAN_POINT('Ctrl Pts',(0.110105217391063,1.99995861702493,27.0734183590793));
#22000=CARTESIAN_POINT('Ctrl Pts',(0.306738966596962,1.97110049161639,27.0611718749675));
#22001=CARTESIAN_POINT('Ctrl Pts',(0.323795820453936,1.9683704376302,27.0601009726926));
#22002=CARTESIAN_POINT('Ctrl Pts',(0.353735505063498,1.96317872925446,27.0582049368789));
#22003=CARTESIAN_POINT('Ctrl Pts',(0.366633679381107,1.96081086865013,27.0573827662986));
#22004=CARTESIAN_POINT('Ctrl Pts',(0.385654884983612,1.9571246981102,27.0561620208309));
#22005=CARTESIAN_POINT('Ctrl Pts',(0.391796739459875,1.95590441682651,27.0557665693331));
#22006=CARTESIAN_POINT('Ctrl Pts',(0.402699531751236,1.95368480420153,27.0550622630596));
#22007=CARTESIAN_POINT('Ctrl Pts',(0.407462772644021,1.95269693379777,27.0547537766876));
#22008=CARTESIAN_POINT('Ctrl Pts',(0.416738749694144,1.95073772843451,27.0541514728172));
#22009=CARTESIAN_POINT('Ctrl Pts',(0.421251824923678,1.94976813237951,27.0538577127876));
#22010=CARTESIAN_POINT('Ctrl Pts',(0.433349820505624,1.94712501583074,27.0530682923024));
#22011=CARTESIAN_POINT('Ctrl Pts',(0.440928339461058,1.94542285656315,27.0525717161052));
#22012=CARTESIAN_POINT('Ctrl Pts',(0.4685984680652,1.93903806999769,27.0507509835917));
#22013=CARTESIAN_POINT('Ctrl Pts',(0.488626475890427,1.93408822835178,27.0494182754833));
#22014=CARTESIAN_POINT('Ctrl Pts',(0.671058754418088,1.88598638384895,27.0371383524665));
#22015=CARTESIAN_POINT('Ctrl Pts',(0.827447741541594,1.82279224832791,27.025501814765));
#22016=CARTESIAN_POINT('Ctrl Pts',(1.03861266980297,1.70463717140479,27.0086216873806));
#22017=CARTESIAN_POINT('Ctrl Pts',(1.1011370423934,1.66493320945291,27.0034697841364));
#22018=CARTESIAN_POINT('Ctrl Pts',(1.19763801000848,1.59583419625229,26.995404636848));
#22019=CARTESIAN_POINT('Ctrl Pts',(1.23308217854283,1.56860850895439,26.9924161919143));
#22020=CARTESIAN_POINT('Ctrl Pts',(1.272664747017,1.53603231929917,26.9890754019891));
#22021=CARTESIAN_POINT('Ctrl Pts',(1.27772389726021,1.53182652071015,26.988648345017));
#22022=CARTESIAN_POINT('Ctrl Pts',(1.28532359894526,1.52544485158716,26.9880068601596));
#22023=CARTESIAN_POINT('Ctrl Pts',(1.28787957481,1.52328754686328,26.9877911169253));
#22024=CARTESIAN_POINT('Ctrl Pts',(1.29228366208294,1.51955138356075,26.987419405886));
#22025=CARTESIAN_POINT('Ctrl Pts',(1.2941343169128,1.51797557311783,26.9872632169682));
#22026=CARTESIAN_POINT('Ctrl Pts',(1.29831035626929,1.51440653768285,26.9869107965521));
#22027=CARTESIAN_POINT('Ctrl Pts',(1.30063402763084,1.51241134254242,26.9867147133901));
#22028=CARTESIAN_POINT('Ctrl Pts',(1.30694051471286,1.50697106295087,26.9861825485773));
#22029=CARTESIAN_POINT('Ctrl Pts',(1.31091433360489,1.50351551539601,26.9858472322528));
#22030=CARTESIAN_POINT('Ctrl Pts',(1.32901417061324,1.48764997402661,26.9843197336432));
#22031=CARTESIAN_POINT('Ctrl Pts',(1.34297853469373,1.47505587292216,26.9831406530443));
#22032=CARTESIAN_POINT('Ctrl Pts',(1.36414978678315,1.4554121245445,26.9813482976862));
#22033=CARTESIAN_POINT('Ctrl Pts',(1.37148435928995,1.44850259010828,26.9807264521344));
#22034=CARTESIAN_POINT('Ctrl Pts',(1.5219094480837,1.30462770661271,26.9679463144279));
#22035=CARTESIAN_POINT('Ctrl Pts',(1.64387870841392,1.1471472277165,26.9569813693188));
#22036=CARTESIAN_POINT('Ctrl Pts',(1.76534526605985,0.930129337140123,26.942193020355));
#22037=CARTESIAN_POINT('Ctrl Pts',(1.78835387866926,0.88508435395895,26.9391457441888));
#22038=CARTESIAN_POINT('Ctrl Pts',(1.82237676931385,0.811719859633889,26.934180849798));
#22039=CARTESIAN_POINT('Ctrl Pts',(1.83449937217942,0.783937573250285,26.9323004557604));
#22040=CARTESIAN_POINT('Ctrl Pts',(1.84927073273663,0.747863995754283,26.9298540673233));
#22041=CARTESIAN_POINT('Ctrl Pts',(1.85250518945258,0.739815732682226,26.9293079645264));
#22042=CARTESIAN_POINT('Ctrl Pts',(1.85764171375973,0.726789666378497,26.9284235172365));
#22043=CARTESIAN_POINT('Ctrl Pts',(1.85957653018366,0.721824828712571,26.9280862775469));
#22044=CARTESIAN_POINT('Ctrl Pts',(1.86323233010537,0.712331604214012,26.9274411592409));
#22045=CARTESIAN_POINT('Ctrl Pts',(1.86495675816197,0.707804577420693,26.9271333989234));
#22046=CARTESIAN_POINT('Ctrl Pts',(1.86886548573625,0.697429800048986,26.9264277881906));
#22047=CARTESIAN_POINT('Ctrl Pts',(1.87103885145382,0.691578010537166,26.9260295755416));
#22048=CARTESIAN_POINT('Ctrl Pts',(1.87765064034761,0.673516453456321,26.9247997576797));
#22049=CARTESIAN_POINT('Ctrl Pts',(1.8819972083418,0.661273645922266,26.9239651081388));
#22050=CARTESIAN_POINT('Ctrl Pts',(1.92763843406612,0.528621935544873,26.9149090043765));
#22051=CARTESIAN_POINT('Ctrl Pts',(1.95742857562902,0.404590235290474,26.9063005177591));
#22052=CARTESIAN_POINT('Ctrl Pts',(1.99691470390854,0.12463226314581,26.8867069778729));
#22053=CARTESIAN_POINT('Ctrl Pts',(2.00055582696806,-0.0313380870244883,
26.8756739806269));
#22054=CARTESIAN_POINT('Ctrl Pts',(1.98435228346906,-0.204212107640017,
26.8641661205944));
#22055=CARTESIAN_POINT('Ctrl Pts',(1.98241324781325,-0.222248378817915,
26.8629749732254));
#22056=CARTESIAN_POINT('Ctrl Pts',(1.97962995826503,-0.245188652906416,
26.8614741712327));
#22057=CARTESIAN_POINT('Ctrl Pts',(1.97901311340757,-0.250118662688979,
26.8611524780768));
#22058=CARTESIAN_POINT('Ctrl Pts',(1.97799474047609,-0.258018113938238,
26.8606384235504));
#22059=CARTESIAN_POINT('Ctrl Pts',(1.97760493531469,-0.260989004714034,
26.8604454116184));
#22060=CARTESIAN_POINT('Ctrl Pts',(1.97684894350177,-0.26665182818081,26.8600781319914));
#22061=CARTESIAN_POINT('Ctrl Pts',(1.97648395620222,-0.269343858014512,
26.8599038018848));
#22062=CARTESIAN_POINT('Ctrl Pts',(1.97562989414417,-0.275547921533612,
26.8595026492185));
#22063=CARTESIAN_POINT('Ctrl Pts',(1.9751369539273,-0.279059401208969,26.8592760474144));
#22064=CARTESIAN_POINT('Ctrl Pts',(1.97378961891658,-0.28847476144236,26.8586696185915));
#22065=CARTESIAN_POINT('Ctrl Pts',(1.97291809153942,-0.294376211637407,
26.8582907402236));
#22066=CARTESIAN_POINT('Ctrl Pts',(1.96638433329972,-0.337286064338147,
26.8555442252955));
#22067=CARTESIAN_POINT('Ctrl Pts',(1.95970723516138,-0.37413530337609,26.8532307589938));
#22068=CARTESIAN_POINT('Ctrl Pts',(1.93448831525661,-0.493974477653454,
26.8457909822654));
#22069=CARTESIAN_POINT('Ctrl Pts',(1.91167774270641,-0.575974372203325,
26.8408310162175));
#22070=CARTESIAN_POINT('Ctrl Pts',(1.85054944419298,-0.751430752443487,
26.8300419323936));
#22071=CARTESIAN_POINT('Ctrl Pts',(1.81023517969291,-0.843936550597181,
26.8242331946577));
#22072=CARTESIAN_POINT('Ctrl Pts',(1.73910795866076,-0.978347448872652,
26.8151961323744));
#22073=CARTESIAN_POINT('Ctrl Pts',(1.71336992197817,-1.02275272047976,26.8121057254511));
#22074=CARTESIAN_POINT('Ctrl Pts',(1.66957838426229,-1.0920045469544,26.8070767299766));
#22075=CARTESIAN_POINT('Ctrl Pts',(1.65261308554818,-1.11751319535862,26.8051766171205));
#22076=CARTESIAN_POINT('Ctrl Pts',(1.63008075361425,-1.14975653931474,26.8027080330895));
#22077=CARTESIAN_POINT('Ctrl Pts',(1.62504703464881,-1.1568601878827,26.8021599070082));
#22078=CARTESIAN_POINT('Ctrl Pts',(1.61685363524085,-1.16826382083532,26.8012729748947));
#22079=CARTESIAN_POINT('Ctrl Pts',(1.61372288483648,-1.17258453124573,26.8009352851152));
#22080=CARTESIAN_POINT('Ctrl Pts',(1.60771775859644,-1.18080253296128,26.8002898327103));
#22081=CARTESIAN_POINT('Ctrl Pts',(1.60484644835808,-1.18470202568707,26.7999821906016));
#22082=CARTESIAN_POINT('Ctrl Pts',(1.598249729667,-1.19359296127723,26.7992775950071));
#22083=CARTESIAN_POINT('Ctrl Pts',(1.59451510002529,-1.198577469306,26.7988802829783));
#22084=CARTESIAN_POINT('Ctrl Pts',(1.58296185977137,-1.21384770030322,26.7976559624247));
#22085=CARTESIAN_POINT('Ctrl Pts',(1.57506673642062,-1.22407485546644,26.7968259488745));
#22086=CARTESIAN_POINT('Ctrl Pts',(1.49883835472969,-1.32086068868532,26.7888733501473));
#22087=CARTESIAN_POINT('Ctrl Pts',(1.42354897002234,-1.40167409221848,26.7814647968924));
#22088=CARTESIAN_POINT('Ctrl Pts',(1.21473376378135,-1.5915493224345,26.7620173305601));
#22089=CARTESIAN_POINT('Ctrl Pts',(1.07306056622204,-1.69031041188822,26.7497471057844));
#22090=CARTESIAN_POINT('Ctrl Pts',(0.903899811883599,-1.77829744931058,
26.7371014203918));
#22091=CARTESIAN_POINT('Ctrl Pts',(0.887202112564299,-1.78668664345683,
26.735873854914));
#22092=CARTESIAN_POINT('Ctrl Pts',(0.865871430225537,-1.79703072552548,
26.7343340288122));
#22093=CARTESIAN_POINT('Ctrl Pts',(0.861346277993833,-1.79920408872352,
26.7340089671626));
#22094=CARTESIAN_POINT('Ctrl Pts',(0.854096671865346,-1.80265234716841,
26.7334908096801));
#22095=CARTESIAN_POINT('Ctrl Pts',(0.851377492694039,-1.80393818488103,
26.7332970450913));
#22096=CARTESIAN_POINT('Ctrl Pts',(0.846199760827307,-1.80637230107773,
26.732929215386));
#22097=CARTESIAN_POINT('Ctrl Pts',(0.843741804024056,-1.80752169932998,
26.7327550842244));
#22098=CARTESIAN_POINT('Ctrl Pts',(0.838086633390827,-1.81015214076514,
26.7323555490711));
#22099=CARTESIAN_POINT('Ctrl Pts',(0.83488783779947,-1.81162972942749,26.7321303599627));
#22100=CARTESIAN_POINT('Ctrl Pts',(0.824707677684042,-1.81629946248286,
26.7314161971569));
#22101=CARTESIAN_POINT('Ctrl Pts',(0.817711688158443,-1.81945983486432,
26.7309291415866));
#22102=CARTESIAN_POINT('Ctrl Pts',(0.704192853961239,-1.86995388408844,
26.7230834950702));
#22103=CARTESIAN_POINT('Ctrl Pts',(0.593722365550085,-1.90790922564198,
26.7162582654751));
#22104=CARTESIAN_POINT('Ctrl Pts',(0.381331703983508,-1.96062878259491,
26.7035419080329));
#22105=CARTESIAN_POINT('Ctrl Pts',(0.280367517858031,-1.97759252206167,
26.6976564886392));
#22106=CARTESIAN_POINT('Ctrl Pts',(0.125593572910727,-1.99150215547713,
26.6884354119564));
#22107=CARTESIAN_POINT('Ctrl Pts',(0.0724717364806699,-1.99414186156437,
26.6852372413083));
#22108=CARTESIAN_POINT('Ctrl Pts',(-0.0121201715123191,-1.99496081668052,
26.6800484637605));
#22109=CARTESIAN_POINT('Ctrl Pts',(-0.0435524338473951,-1.99452214133124,
26.6780995607384));
#22110=CARTESIAN_POINT('Ctrl Pts',(-0.083738947343184,-1.99301092113365,
26.6755761218088));
#22111=CARTESIAN_POINT('Ctrl Pts',(-0.0925155966413155,-1.99262279507719,
26.6750230758507));
#22112=CARTESIAN_POINT('Ctrl Pts',(-0.106635705332029,-1.99190487899414,
26.6741301009403));
#22113=CARTESIAN_POINT('Ctrl Pts',(-0.111980967619995,-1.99161152903668,
26.6737913162781));
#22114=CARTESIAN_POINT('Ctrl Pts',(-0.122155072704288,-1.99101208229963,
26.6731450364761));
#22115=CARTESIAN_POINT('Ctrl Pts',(-0.126984116495725,-1.99070992541116,
26.6728376672052));
#22116=CARTESIAN_POINT('Ctrl Pts',(-0.137993752388975,-1.98998082119529,
26.6721354697561));
#22117=CARTESIAN_POINT('Ctrl Pts',(-0.144173527124846,-1.98954264519977,
26.6717402917702));
#22118=CARTESIAN_POINT('Ctrl Pts',(-0.163066403830353,-1.98811456236324,
26.6705289414675));
#22119=CARTESIAN_POINT('Ctrl Pts',(-0.17577194331572,-1.98703154895143,
26.6697098558245));
#22120=CARTESIAN_POINT('Ctrl Pts',(-0.287350873418209,-1.97644208926666,
26.6624764334676));
#22121=CARTESIAN_POINT('Ctrl Pts',(-0.385380687577209,-1.9596862162087,
26.65583225197));
#22122=CARTESIAN_POINT('Ctrl Pts',(-0.616787739014875,-1.90209546357603,
26.6394756916763));
#22123=CARTESIAN_POINT('Ctrl Pts',(-0.74793506557626,-1.85444983353104,
26.629630275672));
#22124=CARTESIAN_POINT('Ctrl Pts',(-0.926498968511898,-1.76752954014019,
26.6160078528213));
#22125=CARTESIAN_POINT('Ctrl Pts',(-0.978762556778147,-1.73913381651503,
26.6119972700661));
#22126=CARTESIAN_POINT('Ctrl Pts',(-1.0355491879007,-1.70490830422718,26.6076741718831));
#22127=CARTESIAN_POINT('Ctrl Pts',(-1.04139545693419,-1.70134357258578,
26.6072295335165));
#22128=CARTESIAN_POINT('Ctrl Pts',(-1.05011658572411,-1.69596411358556,
26.6065670299919));
#22129=CARTESIAN_POINT('Ctrl Pts',(-1.05300527414928,-1.69417207249398,
26.6063477190831));
#22130=CARTESIAN_POINT('Ctrl Pts',(-1.05795712487784,-1.69108255985268,
26.6059720131795));
#22131=CARTESIAN_POINT('Ctrl Pts',(-1.06002249834409,-1.68978868666051,
26.6058153826207));
#22132=CARTESIAN_POINT('Ctrl Pts',(-1.06432336690025,-1.68708337746436,
26.6054893763965));
#22133=CARTESIAN_POINT('Ctrl Pts',(-1.06655841983701,-1.68567128738697,
26.605320045839));
#22134=CARTESIAN_POINT('Ctrl Pts',(-1.07275900920254,-1.68173653102068,
26.604850502667));
#22135=CARTESIAN_POINT('Ctrl Pts',(-1.07671848014454,-1.67920426607269,
26.6045509219677));
#22136=CARTESIAN_POINT('Ctrl Pts',(-1.09135159271219,-1.66977267578,26.6034445466298));
#22137=CARTESIAN_POINT('Ctrl Pts',(-1.10196845470289,-1.66278520333276,
26.6026433980875));
#22138=CARTESIAN_POINT('Ctrl Pts',(-1.12418832813985,-1.64785492368984,
26.600968377322));
#22139=CARTESIAN_POINT('Ctrl Pts',(-1.13577564304281,-1.63988992283795,
26.6000958687759));
#22140=CARTESIAN_POINT('Ctrl Pts',(-1.31505183333017,-1.51384549806041,
26.5865958649654));
#22141=CARTESIAN_POINT('Ctrl Pts',(-1.46365152895638,-1.37070760257481,
26.5752812872329));
#22142=CARTESIAN_POINT('Ctrl Pts',(-1.61694016391936,-1.16912155139533,
26.5601911800423));
#22143=CARTESIAN_POINT('Ctrl Pts',(-1.64465578330973,-1.1297997781298,26.55728756095));
#22144=CARTESIAN_POINT('Ctrl Pts',(-1.68688208749409,-1.06504001305279,
26.5525368107231));
#22145=CARTESIAN_POINT('Ctrl Pts',(-1.70230170220518,-1.04021641126892,
26.5507229007947));
#22146=CARTESIAN_POINT('Ctrl Pts',(-1.72152687731665,-1.00769344647638,
26.5483514616334));
#22147=CARTESIAN_POINT('Ctrl Pts',(-1.72583627845885,-1.00029496033239,
26.5478123339418));
#22148=CARTESIAN_POINT('Ctrl Pts',(-1.73273771173502,-0.988269049228014,
26.5469364513506));
#22149=CARTESIAN_POINT('Ctrl Pts',(-1.73535918492558,-0.983658573763605,
26.5466007621425));
#22150=CARTESIAN_POINT('Ctrl Pts',(-1.74034307807082,-0.974811296802802,
26.5459567662677));
#22151=CARTESIAN_POINT('Ctrl Pts',(-1.74270849414668,-0.97057621931986,
26.5456485701755));
#22152=CARTESIAN_POINT('Ctrl Pts',(-1.74805615038108,-0.960919117117224,
26.5449459529696));
#22153=CARTESIAN_POINT('Ctrl Pts',(-1.75102864427979,-0.955491779143886,
26.5445511869786));
#22154=CARTESIAN_POINT('Ctrl Pts',(-1.76019452973022,-0.938569797468603,
26.5433206194059));
#22155=CARTESIAN_POINT('Ctrl Pts',(-1.76630024818284,-0.927028298922435,
26.5424817174519));
#22156=CARTESIAN_POINT('Ctrl Pts',(-1.77788070048859,-0.90460824395497,
26.5408525887931));
#22157=CARTESIAN_POINT('Ctrl Pts',(-1.78336999617227,-0.893737828460682,
26.540062921269));
#22158=CARTESIAN_POINT('Ctrl Pts',(-1.85354314901331,-0.751553508897692,
26.5297358685534));
#22159=CARTESIAN_POINT('Ctrl Pts',(-1.90366914354141,-0.613582078641405,
26.5196835777378));
#22160=CARTESIAN_POINT('Ctrl Pts',(-1.96803445699008,-0.34893188742608,
26.5006927911525));
#22161=CARTESIAN_POINT('Ctrl Pts',(-1.98614825525813,-0.223906023392428,
26.4918495679565));
#22162=CARTESIAN_POINT('Ctrl Pts',(-1.99288065852635,-0.0870330910302871,
26.4827851965441));
#22163=CARTESIAN_POINT('Ctrl Pts',(-1.99332947186261,-0.0760638362088492,
26.4820631776488));
#22164=CARTESIAN_POINT('Ctrl Pts',(-1.99395253335949,-0.0569799828751236,
26.4808153551949));
#22165=CARTESIAN_POINT('Ctrl Pts',(-1.99416785543449,-0.0488671009836684,
26.4802874960542));
#22166=CARTESIAN_POINT('Ctrl Pts',(-1.99440810146639,-0.037110146430956,
26.4795265400302));
#22167=CARTESIAN_POINT('Ctrl Pts',(-1.99447255989448,-0.0334670959027242,
26.4792913042332));
#22168=CARTESIAN_POINT('Ctrl Pts',(-1.99456773336815,-0.0271021885634675,
26.4788813116109));
#22169=CARTESIAN_POINT('Ctrl Pts',(-1.99460285948886,-0.0243804204677668,
26.4787063089989));
#22170=CARTESIAN_POINT('Ctrl Pts',(-1.99466073430711,-0.0190504690719636,
26.4783642390629));
#22171=CARTESIAN_POINT('Ctrl Pts',(-1.99468393876935,-0.0164423224033568,
26.478197145991));
#22172=CARTESIAN_POINT('Ctrl Pts',(-1.99473339151064,-0.00931187333839594,
26.4777411151937));
#22173=CARTESIAN_POINT('Ctrl Pts',(-1.99474937674971,-0.0047894801152562,
26.4774527494229));
#22174=CARTESIAN_POINT('Ctrl Pts',(-1.99475185659427,0.0137361181896936,
26.47627488716));
#22175=CARTESIAN_POINT('Ctrl Pts',(-1.9946062781266,0.0277393604116115,
26.4753925230793));
#22176=CARTESIAN_POINT('Ctrl Pts',(-1.99241474663792,0.132448529288717,
26.468846486816));
#22177=CARTESIAN_POINT('Ctrl Pts',(-1.98432958457099,0.222933759005454,
26.4634783153668));
#22178=CARTESIAN_POINT('Ctrl Pts',(-1.95880133593162,0.383839807844613,
26.4539688877398));
#22179=CARTESIAN_POINT('Ctrl Pts',(-1.94363352561543,0.454449734028068,
26.4498087069397));
#22180=CARTESIAN_POINT('Ctrl Pts',(-1.89190203917916,0.644431498507619,
26.4383407757964));
#22181=CARTESIAN_POINT('Ctrl Pts',(-1.84792148585435,0.761422867130402,
26.4309560836767));
#22182=CARTESIAN_POINT('Ctrl Pts',(-1.78761479324789,0.885228867718535,
26.4223607905538));
#22183=CARTESIAN_POINT('Ctrl Pts',(-1.78180376652631,0.896867951321353,
26.4215449831546));
#22184=CARTESIAN_POINT('Ctrl Pts',(-1.77303495211782,0.914009645017655,
26.4203316002231));
#22185=CARTESIAN_POINT('Ctrl Pts',(-1.7701644123944,0.919556699865657,26.4199370893696));
#22186=CARTESIAN_POINT('Ctrl Pts',(-1.76502105930991,0.929382426540547,
26.4192349247278));
#22187=CARTESIAN_POINT('Ctrl Pts',(-1.76275861020527,0.933666490797689,
26.4189276391711));
#22188=CARTESIAN_POINT('Ctrl Pts',(-1.75797590985675,0.942643430729684,
26.4182813297268));
#22189=CARTESIAN_POINT('Ctrl Pts',(-1.75545242613107,0.947334532157192,
26.4179421927728));
#22190=CARTESIAN_POINT('Ctrl Pts',(-1.7487742582021,0.95963079154519,26.4170495510533));
#22191=CARTESIAN_POINT('Ctrl Pts',(-1.74458878643574,0.967219015809541,
26.4164949506273));
#22192=CARTESIAN_POINT('Ctrl Pts',(-1.7255808327729,1.00115547518758,26.4139976001845));
#22193=CARTESIAN_POINT('Ctrl Pts',(-1.7102106353266,1.02719078649811,26.4120352389543));
#22194=CARTESIAN_POINT('Ctrl Pts',(-1.66765988422647,1.09566281040562,26.406745552761));
#22195=CARTESIAN_POINT('Ctrl Pts',(-1.6394543682798,1.13743357580766,26.4033821493995));
#22196=CARTESIAN_POINT('Ctrl Pts',(-1.55059729495721,1.25884478170398,26.3931924628638));
#22197=CARTESIAN_POINT('Ctrl Pts',(-1.4855063352444,1.33503174736399,26.3862289557524));
#22198=CARTESIAN_POINT('Ctrl Pts',(-1.32818174023148,1.49336051102167,26.3706557698497));
#22199=CARTESIAN_POINT('Ctrl Pts',(-1.23346858964307,1.57249961726009,26.3620662708068));
#22200=CARTESIAN_POINT('Ctrl Pts',(-1.12583008763503,1.64669099971828,26.3535312768325));
#22201=CARTESIAN_POINT('Ctrl Pts',(-1.11958546507842,1.65094307157835,26.3530402414235));
#22202=CARTESIAN_POINT('Ctrl Pts',(-1.11041204981948,1.65711342292827,26.3523250893724));
#22203=CARTESIAN_POINT('Ctrl Pts',(-1.10750221808766,1.65905956922099,26.3520991450738));
#22204=CARTESIAN_POINT('Ctrl Pts',(-1.10233047906725,1.66249884896086,26.3516991893072));
#22205=CARTESIAN_POINT('Ctrl Pts',(-1.10007063648844,1.66399504295032,26.3515249725581));
#22206=CARTESIAN_POINT('Ctrl Pts',(-1.09528607307665,1.66714879419957,26.3511572825438));
#22207=CARTESIAN_POINT('Ctrl Pts',(-1.09276064212373,1.66880522026967,26.3509638851877));
#22208=CARTESIAN_POINT('Ctrl Pts',(-1.08598143671414,1.67322970270345,26.3504465263594));
#22209=CARTESIAN_POINT('Ctrl Pts',(-1.08172080870011,1.67598729478594,26.3501232594853));
#22210=CARTESIAN_POINT('Ctrl Pts',(-1.06121794808537,1.68914653892736,26.348576436171));
#22211=CARTESIAN_POINT('Ctrl Pts',(-1.04483527341616,1.69932895040902,26.3473668412685));
#22212=CARTESIAN_POINT('Ctrl Pts',(-0.998669686648428,1.72710239342899,
26.3440237401053));
#22213=CARTESIAN_POINT('Ctrl Pts',(-0.968572048685566,1.74415948255465,
26.3419188843811));
#22214=CARTESIAN_POINT('Ctrl Pts',(-0.857072985933626,1.80357183198289,
26.3343338739697));
#22215=CARTESIAN_POINT('Ctrl Pts',(-0.773215844155963,1.84108255915724,
26.3290291909821));
#22216=CARTESIAN_POINT('Ctrl Pts',(-0.540926164620284,1.9263071435606,26.3146788441818));
#22217=CARTESIAN_POINT('Ctrl Pts',(-0.389033331272474,1.96262684333847,
26.3056089302712));
#22218=CARTESIAN_POINT('Ctrl Pts',(-0.221984301227528,1.98239973084691,
26.2951046108969));
#22219=CARTESIAN_POINT('Ctrl Pts',(-0.20948183725367,1.98375983202795,26.2943156750733));
#22220=CARTESIAN_POINT('Ctrl Pts',(-0.190837078200525,1.98560991261882,
26.2931347225811));
#22221=CARTESIAN_POINT('Ctrl Pts',(-0.184703855599289,1.98618981969231,
26.292745535163));
#22222=CARTESIAN_POINT('Ctrl Pts',(-0.173753098931749,1.98717407255697,
26.2920493401442));
#22223=CARTESIAN_POINT('Ctrl Pts',(-0.168936575170822,1.98758933558376,
26.2917426782509));
#22224=CARTESIAN_POINT('Ctrl Pts',(-0.158764373488071,1.9884291034863,26.2910940544471));
#22225=CARTESIAN_POINT('Ctrl Pts',(-0.15340840288067,1.98884948824057,26.290751965607));
#22226=CARTESIAN_POINT('Ctrl Pts',(-0.139204106616541,1.98990665043685,
26.2898431887471));
#22227=CARTESIAN_POINT('Ctrl Pts',(-0.130353198129671,1.99050604125467,
26.2892753320646));
#22228=CARTESIAN_POINT('Ctrl Pts',(-0.0892312018048569,1.99301540984878,
26.2866294448014));
#22229=CARTESIAN_POINT('Ctrl Pts',(-0.0569222911537299,1.99419965905707,
26.284528827396));
#22230=CARTESIAN_POINT('Ctrl Pts',(0.0306817334046424,1.99528012333654,
26.2787702558293));
#22231=CARTESIAN_POINT('Ctrl Pts',(0.0859636232140479,1.99366332694163,
26.2750678508332));
#22232=CARTESIAN_POINT('Ctrl Pts',(0.244771471743728,1.98240149380513,26.2642428765634));
#22233=CARTESIAN_POINT('Ctrl Pts',(0.347699623840962,1.96695970827862,26.2569854971615));
#22234=CARTESIAN_POINT('Ctrl Pts',(0.518424920590111,1.92752378182725,26.2447665599753));
#22235=CARTESIAN_POINT('Ctrl Pts',(0.58699673550787,1.90776004002007,26.2398108903183));
#22236=CARTESIAN_POINT('Ctrl Pts',(0.662727332694286,1.88146176734226,26.2343734404213));
#22237=CARTESIAN_POINT('Ctrl Pts',(0.671069080322281,1.87850264672185,26.2337750311104));
#22238=CARTESIAN_POINT('Ctrl Pts',(0.710894065166959,1.86407614292352,26.2309215021966));
#22239=CARTESIAN_POINT('Ctrl Pts',(0.74210697676578,1.85187143207115,26.228695138789));
#22240=CARTESIAN_POINT('Ctrl Pts',(0.778317152497066,1.83665000582119,26.2261362416073));
#22241=CARTESIAN_POINT('Ctrl Pts',(0.783624929106467,1.8343916719782,26.2257617646161));
#22242=CARTESIAN_POINT('Ctrl Pts',(0.79212643437708,1.83073084857593,26.2251630334546));
#22243=CARTESIAN_POINT('Ctrl Pts',(0.795326361449667,1.82934297145295,26.224937918412));
#22244=CARTESIAN_POINT('Ctrl Pts',(0.801004702247619,1.82686243751916,26.2245389032379));
#22245=CARTESIAN_POINT('Ctrl Pts',(0.803484546826355,1.82577311898268,26.2243648012286));
#22246=CARTESIAN_POINT('Ctrl Pts',(0.808731333047573,1.82345560887289,26.2239967778307));
#22247=CARTESIAN_POINT('Ctrl Pts',(0.811497691986622,1.82222617223619,26.2238029345731));
#22248=CARTESIAN_POINT('Ctrl Pts',(0.818923149510501,1.81890585691757,26.2232831209708));
#22249=CARTESIAN_POINT('Ctrl Pts',(0.823577074781566,1.81680335876355,26.2229578567514));
#22250=CARTESIAN_POINT('Ctrl Pts',(0.846091617724544,1.80652770123288,26.2213866397609));
#22251=CARTESIAN_POINT('Ctrl Pts',(0.86383969047805,1.7981085675307,26.2201551864568));
#22252=CARTESIAN_POINT('Ctrl Pts',(0.91329673198017,1.77374633450444,26.2167357284304));
#22253=CARTESIAN_POINT('Ctrl Pts',(0.944710020340432,1.75721662622919,26.2145779848323));
#22254=CARTESIAN_POINT('Ctrl Pts',(1.0589970846477,1.69312734096632,26.2067195810789));
#22255=CARTESIAN_POINT('Ctrl Pts',(1.13886760514968,1.64046884265803,26.2012068375491));
#22256=CARTESIAN_POINT('Ctrl Pts',(1.22293719960101,1.57593180041014,26.1950585883482));
#22257=CARTESIAN_POINT('Ctrl Pts',(1.23116382018762,1.5695133260715,26.1944531002979));
#22258=CARTESIAN_POINT('Ctrl Pts',(1.34869327843517,1.47632326267751,26.1857424046758));
#22259=CARTESIAN_POINT('Ctrl Pts',(1.44862871503805,1.37839423452942,26.1775421761836));
#22260=CARTESIAN_POINT('Ctrl Pts',(1.54574829324497,1.26089512000377,26.16802657748));
#22261=CARTESIAN_POINT('Ctrl Pts',(1.55387767494147,1.25086308145653,26.167216774584));
#22262=CARTESIAN_POINT('Ctrl Pts',(1.56578212778264,1.23587728561667,26.1660106308452));
#22263=CARTESIAN_POINT('Ctrl Pts',(1.56963242968722,1.23098349746558,26.16561730129));
#22264=CARTESIAN_POINT('Ctrl Pts',(1.57643609614817,1.22225212050456,26.1649164675145));
#22265=CARTESIAN_POINT('Ctrl Pts',(1.57939853241792,1.21842163737982,26.1646093265203));
#22266=CARTESIAN_POINT('Ctrl Pts',(1.58559633456413,1.21034718369656,26.1639625335058));
#22267=CARTESIAN_POINT('Ctrl Pts',(1.58882867148446,1.20610094644759,26.1636227654224));
#22268=CARTESIAN_POINT('Ctrl Pts',(1.59729163250779,1.19489031519034,26.162726673718));
#22269=CARTESIAN_POINT('Ctrl Pts',(1.60249370412724,1.18790460427443,26.1621692389836));
#22270=CARTESIAN_POINT('Ctrl Pts',(1.62580514522594,1.15616855123185,26.159640875042));
#22271=CARTESIAN_POINT('Ctrl Pts',(1.6433871858039,1.13103778559928,26.1576497319203));
#22272=CARTESIAN_POINT('Ctrl Pts',(1.68886413643025,1.06273544179683,26.15226355236));
#22273=CARTESIAN_POINT('Ctrl Pts',(1.71568008045751,1.01887673064159,26.1488307955993));
#22274=CARTESIAN_POINT('Ctrl Pts',(1.79002954141133,0.88600118239082,26.1385100615273));
#22275=CARTESIAN_POINT('Ctrl Pts',(1.8325351114359,0.794364910200626,26.131485189322));
#22276=CARTESIAN_POINT('Ctrl Pts',(1.89528980754297,0.626886221083859,26.1190069485199));
#22277=CARTESIAN_POINT('Ctrl Pts',(1.91834950455345,0.552309976563445,26.1135718554628));
#22278=CARTESIAN_POINT('Ctrl Pts',(1.94744166928258,0.434067354181813,26.1052995602191));
#22279=CARTESIAN_POINT('Ctrl Pts',(1.95649839041601,0.391226604846006,26.1023717119027));
#22280=CARTESIAN_POINT('Ctrl Pts',(1.96534497275748,0.341312874227525,26.0990661093336));
#22281=CARTESIAN_POINT('Ctrl Pts',(1.9665158984502,0.334500470266664,26.0986172135613));
#22282=CARTESIAN_POINT('Ctrl Pts',(1.96821198039782,0.324315906977759,26.0979496318969));
#22283=CARTESIAN_POINT('Ctrl Pts',(1.96876391735158,0.320948353261616,26.0977294678346));
#22284=CARTESIAN_POINT('Ctrl Pts',(1.96973613618521,0.31491963178232,26.0973363681478));
#22285=CARTESIAN_POINT('Ctrl Pts',(1.97015966938895,0.312259024031686,26.0971632499953));
#22286=CARTESIAN_POINT('Ctrl Pts',(1.97106054339876,0.306524991128492,26.0967909430602));
#22287=CARTESIAN_POINT('Ctrl Pts',(1.97153608513815,0.303451316114563,26.0965918575256));
#22288=CARTESIAN_POINT('Ctrl Pts',(1.97282976192237,0.294958187562228,26.0960430586312));
#22289=CARTESIAN_POINT('Ctrl Pts',(1.97363276078984,0.289536403895955,26.0956941935494));
#22290=CARTESIAN_POINT('Ctrl Pts',(1.97788617700363,0.259977558639935,26.0937999116733));
#22291=CARTESIAN_POINT('Ctrl Pts',(1.98091635127636,0.235780831643728,26.0922771517358));
#22292=CARTESIAN_POINT('Ctrl Pts',(1.98865181483683,0.163247059783556,26.087779333982));
#22293=CARTESIAN_POINT('Ctrl Pts',(1.99203682554155,0.114785151720892,26.0848625697586));
#22294=CARTESIAN_POINT('Ctrl Pts',(1.99446808830493,0.0416156628385256,
26.0805283161669));
#22295=CARTESIAN_POINT('Ctrl Pts',(1.99483001390177,0.016973098859942,26.0790804906789));
#22296=CARTESIAN_POINT('Ctrl Pts',(1.99426672636337,-0.129514519424248,
26.0705137595227));
#22297=CARTESIAN_POINT('Ctrl Pts',(1.98263568426723,-0.251056740084457,
26.0635525048635));
#22298=CARTESIAN_POINT('Ctrl Pts',(1.95414678151079,-0.401653202858875,
26.054471602337));
#22299=CARTESIAN_POINT('Ctrl Pts',(1.94757752788801,-0.432384765997712,
26.0525952119452));
#22300=CARTESIAN_POINT('Ctrl Pts',(1.92815637048739,-0.513781890406775,
26.0475466650199));
#22301=CARTESIAN_POINT('Ctrl Pts',(1.91403526826719,-0.564116187350478,
26.044342077686));
#22302=CARTESIAN_POINT('Ctrl Pts',(1.89492958659536,-0.623190261119388,
26.0404573063918));
#22303=CARTESIAN_POINT('Ctrl Pts',(1.89183480609136,-0.632522964511125,
26.0398398722316));
#22304=CARTESIAN_POINT('Ctrl Pts',(1.88668358510471,-0.647681072158943,
26.038830829571));
#22305=CARTESIAN_POINT('Ctrl Pts',(1.88466883283597,-0.65352055107582,26.0384405988675));
#22306=CARTESIAN_POINT('Ctrl Pts',(1.88102838348234,-0.663915034764084,
26.0377432397127));
#22307=CARTESIAN_POINT('Ctrl Pts',(1.87941317640742,-0.668473682745276,
26.0374364613772));
#22308=CARTESIAN_POINT('Ctrl Pts',(1.87597189274502,-0.678075057548505,
26.0367883192272));
#22309=CARTESIAN_POINT('Ctrl Pts',(1.87414202797496,-0.683116376681361,
26.0364468312747));
#22310=CARTESIAN_POINT('Ctrl Pts',(1.86924588554003,-0.696437607244069,
26.0355413390327));
#22311=CARTESIAN_POINT('Ctrl Pts',(1.8661449524954,-0.704704571795733,26.0349761810928));
#22312=CARTESIAN_POINT('Ctrl Pts',(1.85159155344792,-0.74273361280262,26.0323612654904));
#22313=CARTESIAN_POINT('Ctrl Pts',(1.83948186027241,-0.772237522004765,
26.0302895600559));
#22314=CARTESIAN_POINT('Ctrl Pts',(1.80487611604055,-0.851112455191398,
26.0246301739942));
#22315=CARTESIAN_POINT('Ctrl Pts',(1.78106603532669,-0.899873934694573,
26.0209998968339));
#22316=CARTESIAN_POINT('Ctrl Pts',(1.66142325844926,-1.12149566569647,26.0038893855869));
#22317=CARTESIAN_POINT('Ctrl Pts',(1.54224236576821,-1.280451718441,25.9896970254888));
#22318=CARTESIAN_POINT('Ctrl Pts',(1.38522509308509,-1.43551814194517,25.9749814697341));
#22319=CARTESIAN_POINT('Ctrl Pts',(1.36851196018866,-1.4514599626903,25.9734582545449));
#22320=CARTESIAN_POINT('Ctrl Pts',(1.34740476751152,-1.47090425795328,25.9715914848922));
#22321=CARTESIAN_POINT('Ctrl Pts',(1.3432686367981,-1.47468244541253,25.9712283276274));
#22322=CARTESIAN_POINT('Ctrl Pts',(1.33676644565324,-1.48057187824255,25.9706616422081));
#22323=CARTESIAN_POINT('Ctrl Pts',(1.33441121429464,-1.48269495459303,25.970457235715));
#22324=CARTESIAN_POINT('Ctrl Pts',(1.33006865634126,-1.48659073845232,25.9700819462337));
#22325=CARTESIAN_POINT('Ctrl Pts',(1.32808285889487,-1.48836506755106,25.9699109424082));
#22326=CARTESIAN_POINT('Ctrl Pts',(1.3236131314964,-1.49234274377136,25.9695274054526));
#22327=CARTESIAN_POINT('Ctrl Pts',(1.32112725814866,-1.49454386182717,25.9693150401472));
#22328=CARTESIAN_POINT('Ctrl Pts',(1.31378795609195,-1.50100983112605,25.9686907795093));
#22329=CARTESIAN_POINT('Ctrl Pts',(1.30891923113949,-1.50525737195677,25.9682801573117));
#22330=CARTESIAN_POINT('Ctrl Pts',(1.27017412859174,-1.53872898422214,25.9650392407669));
#22331=CARTESIAN_POINT('Ctrl Pts',(1.23534087024433,-1.5668321096658,25.9622869323671));
#22332=CARTESIAN_POINT('Ctrl Pts',(1.14075002505497,-1.63802939553656,25.9551395550182));
#22333=CARTESIAN_POINT('Ctrl Pts',(1.07949952888634,-1.67902745923303,25.9508358995551));
#22334=CARTESIAN_POINT('Ctrl Pts',(0.871070435635749,-1.80240808538269,
25.9367611815496));
#22335=CARTESIAN_POINT('Ctrl Pts',(0.715745215872706,-1.86952946016563,
25.927084225882));
#22336=CARTESIAN_POINT('Ctrl Pts',(0.534048661929887,-1.92204158425444,
25.9153763170266));
#22337=CARTESIAN_POINT('Ctrl Pts',(0.514174080390318,-1.92745344699057,
25.9140918647329));
#22338=CARTESIAN_POINT('Ctrl Pts',(0.486700466777882,-1.9344793761117,25.9123096860271));
#22339=CARTESIAN_POINT('Ctrl Pts',(0.479170039166781,-1.93635840478393,
25.9118205193527));
#22340=CARTESIAN_POINT('Ctrl Pts',(0.467144859729687,-1.9392845433052,25.9110382278996));
#22341=CARTESIAN_POINT('Ctrl Pts',(0.462657055146897,-1.94036009766553,
25.9107460213456));
#22342=CARTESIAN_POINT('Ctrl Pts',(0.453430501075795,-1.94253751906237,
25.9101447275935));
#22343=CARTESIAN_POINT('Ctrl Pts',(0.448691375477951,-1.94363764142218,
25.9098355865409));
#22344=CARTESIAN_POINT('Ctrl Pts',(0.437839937350715,-1.94611484974783,
25.90912703822));
#22345=CARTESIAN_POINT('Ctrl Pts',(0.431725090198839,-1.94748049134259,
25.9087272666594));
#22346=CARTESIAN_POINT('Ctrl Pts',(0.412745591548754,-1.9516254411941,25.9074848318487));
#22347=CARTESIAN_POINT('Ctrl Pts',(0.399860001809734,-1.95430620712455,
25.9066390268469));
#22348=CARTESIAN_POINT('Ctrl Pts',(0.369943586681603,-1.96022187505819,
25.9046696988374));
#22349=CARTESIAN_POINT('Ctrl Pts',(0.352895446308533,-1.96336263315835,
25.9035432508486));
#22350=CARTESIAN_POINT('Ctrl Pts',(0.156884942412084,-1.99683805978584,
25.890541251457));
#22351=CARTESIAN_POINT('Ctrl Pts',(-0.0253425947507,-2.00282435706728,25.8778530385365));
#22352=CARTESIAN_POINT('Ctrl Pts',(-0.302140482888902,-1.97411182075522,
25.8584881907062));
#22353=CARTESIAN_POINT('Ctrl Pts',(-0.397625518859958,-1.95711654969343,
25.851816954888));
#22354=CARTESIAN_POINT('Ctrl Pts',(-0.499120079866885,-1.93131260899514,
25.8449762414664));
#22355=CARTESIAN_POINT('Ctrl Pts',(-0.506720581867318,-1.92933239869856,
25.8444655548407));
#22356=CARTESIAN_POINT('Ctrl Pts',(-0.517745621579041,-1.92639032460175,
25.8437272749049));
#22357=CARTESIAN_POINT('Ctrl Pts',(-0.521179476180026,-1.92546414286883,
25.8434976846837));
#22358=CARTESIAN_POINT('Ctrl Pts',(-0.527233418461934,-1.92381388751366,
25.843093561166));
#22359=CARTESIAN_POINT('Ctrl Pts',(-0.52985452524474,-1.92309363624678,
25.8429188076313));
#22360=CARTESIAN_POINT('Ctrl Pts',(-0.535356654722064,-1.92156960862007,
25.8425524316907));
#22361=CARTESIAN_POINT('Ctrl Pts',(-0.53823733783313,-1.92076471150913,
25.8423608758351));
#22362=CARTESIAN_POINT('Ctrl Pts',(-0.545875317515864,-1.91861203693715,
25.8418536473996));
#22363=CARTESIAN_POINT('Ctrl Pts',(-0.550629469953649,-1.91725303458705,
25.8415386226704));
#22364=CARTESIAN_POINT('Ctrl Pts',(-0.572562116066159,-1.91089514939675,
25.8400882889479));
#22365=CARTESIAN_POINT('Ctrl Pts',(-0.589678584363909,-1.90568278310088,
25.8389649197564));
#22366=CARTESIAN_POINT('Ctrl Pts',(-0.636381000070517,-1.89077127956367,
25.8359172318337));
#22367=CARTESIAN_POINT('Ctrl Pts',(-0.665814658580627,-1.88060837802264,
25.8340157877586));
#22368=CARTESIAN_POINT('Ctrl Pts',(-0.775617918319599,-1.83979390981897,
25.826953416595));
#22369=CARTESIAN_POINT('Ctrl Pts',(-0.854219509873379,-1.80464289395786,
25.821958583593));
#22370=CARTESIAN_POINT('Ctrl Pts',(-1.02000801428476,-1.7172341610937,25.8110864151556));
#22371=CARTESIAN_POINT('Ctrl Pts',(-1.10596515850756,-1.66317436496698,
25.805222666529));
#22372=CARTESIAN_POINT('Ctrl Pts',(-1.24076967279879,-1.56330545228823,
25.7951955490725));
#22373=CARTESIAN_POINT('Ctrl Pts',(-1.29209339290553,-1.52115960602932,
25.7911529841031));
#22374=CARTESIAN_POINT('Ctrl Pts',(-1.34901745654908,-1.46945244906522,
25.786345818397));
#22375=CARTESIAN_POINT('Ctrl Pts',(-1.35676093838173,-1.46230583238358,
25.7856845890357));
#22376=CARTESIAN_POINT('Ctrl Pts',(-1.36905807138593,-1.45077479695036,
25.7846225509277));
#22377=CARTESIAN_POINT('Ctrl Pts',(-1.37364820636982,-1.44642943759363,
25.7842234146424));
#22378=CARTESIAN_POINT('Ctrl Pts',(-1.38173868762547,-1.43869714834417,
25.7835150417119));
#22379=CARTESIAN_POINT('Ctrl Pts',(-1.38524744344229,-1.43531906044685,
25.7832061895234));
#22380=CARTESIAN_POINT('Ctrl Pts',(-1.3919773898818,-1.42879207725204,25.7826106135402));
#22381=CARTESIAN_POINT('Ctrl Pts',(-1.39520035867988,-1.42564505138953,
25.7823239724779));
#22382=CARTESIAN_POINT('Ctrl Pts',(-1.40207890421909,-1.4188829201228,25.7817091491221));
#22383=CARTESIAN_POINT('Ctrl Pts',(-1.40573121329794,-1.41526455117506,
25.7813808240291));
#22384=CARTESIAN_POINT('Ctrl Pts',(-1.41945116733061,-1.4015665884746,25.7801403429386));
#22385=CARTESIAN_POINT('Ctrl Pts',(-1.42942452537626,-1.39139355579345,
25.7792240441544));
#22386=CARTESIAN_POINT('Ctrl Pts',(-1.48777662855196,-1.33058364036823,
25.7737748262578));
#22387=CARTESIAN_POINT('Ctrl Pts',(-1.53356512403361,-1.27753987903736,
25.7691321964156));
#22388=CARTESIAN_POINT('Ctrl Pts',(-1.61272772427735,-1.17543158055717,
25.7603866729488));
#22389=CARTESIAN_POINT('Ctrl Pts',(-1.6468875298684,-1.12707175312899,25.7563163230258));
#22390=CARTESIAN_POINT('Ctrl Pts',(-1.7629874576479,-0.946138305508907,
25.7414007200954));
#22391=CARTESIAN_POINT('Ctrl Pts',(-1.83148052572356,-0.805597278227731,
25.7303520866869));
#22392=CARTESIAN_POINT('Ctrl Pts',(-1.88759140389618,-0.645156132111088,
25.7191393419408));
#22393=CARTESIAN_POINT('Ctrl Pts',(-1.89212008276404,-0.631751029274498,
25.7182129962918));
#22394=CARTESIAN_POINT('Ctrl Pts',(-1.897966173964,-0.613819321714616,25.7169888378195));
#22395=CARTESIAN_POINT('Ctrl Pts',(-1.89941059427398,-0.609335008582619,
25.7166839462945));
#22396=CARTESIAN_POINT('Ctrl Pts',(-1.90164144578985,-0.602324144809895,
25.7162092576138));
#22397=CARTESIAN_POINT('Ctrl Pts',(-1.9024387477851,-0.599801112780958,
25.716038829642));
#22398=CARTESIAN_POINT('Ctrl Pts',(-1.90396060015198,-0.594951705963677,
25.7157120365177));
#22399=CARTESIAN_POINT('Ctrl Pts',(-1.90468589985617,-0.592625617336767,
25.7155556304472));
#22400=CARTESIAN_POINT('Ctrl Pts',(-1.90641144447034,-0.587055780126092,
25.7151819326798));
#22401=CARTESIAN_POINT('Ctrl Pts',(-1.9074076724485,-0.583810805046987,
25.7149648786783));
#22402=CARTESIAN_POINT('Ctrl Pts',(-1.91038134201225,-0.574035922213185,
25.7143129891375));
#22403=CARTESIAN_POINT('Ctrl Pts',(-1.91233359552819,-0.56749831238639,
25.7138796029367));
#22404=CARTESIAN_POINT('Ctrl Pts',(-1.9306447282768,-0.505011309619001,
25.7097609785098));
#22405=CARTESIAN_POINT('Ctrl Pts',(-1.94457906799819,-0.448373973983803,
25.706208800238));
#22406=CARTESIAN_POINT('Ctrl Pts',(-1.98166579443634,-0.262939890188768,
25.6949197026938));
#22407=CARTESIAN_POINT('Ctrl Pts',(-1.99464064461358,-0.132464691104114,
25.6874821624276));
#22408=CARTESIAN_POINT('Ctrl Pts',(-1.99474931168317,-0.00165711783231753,
25.6798260142406));
#22409=CARTESIAN_POINT('',(-1.99466367889413,0.000990252434004168,24.8790450931555));
#22410=CARTESIAN_POINT('Ctrl Pts',(-1.99474975438214,0.000989895140400634,
24.8790451186048));
#22411=CARTESIAN_POINT('Ctrl Pts',(-1.99478493408844,-0.0699011595160849,
24.8835489941164));
#22412=CARTESIAN_POINT('Ctrl Pts',(-1.99103669367566,-0.140785882431073,
24.8880528696279));
#22413=CARTESIAN_POINT('Ctrl Pts',(-1.98353341726112,-0.211240964560431,
24.8925567451395));
#22414=CARTESIAN_POINT('Ctrl Pts',(-1.97602707455192,-0.281724838917365,
24.8970624612082));
#22415=CARTESIAN_POINT('Ctrl Pts',(-1.96476269732732,-0.351778257317102,
24.9015681772769));
#22416=CARTESIAN_POINT('Ctrl Pts',(-1.94982031519319,-0.420984917734511,
24.9060738933457));
#22417=CARTESIAN_POINT('Ctrl Pts',(-1.93485533688121,-0.490296233888402,
24.910586423051));
#22418=CARTESIAN_POINT('Ctrl Pts',(-1.91620135044852,-0.558757776505707,
24.9150989527564));
#22419=CARTESIAN_POINT('Ctrl Pts',(-1.89398901392024,-0.625965795910172,
24.9196114824617));
#22420=CARTESIAN_POINT('Ctrl Pts',(-1.87175843849076,-0.693229000883427,
24.9241277174766));
#22421=CARTESIAN_POINT('Ctrl Pts',(-1.84596386614983,-0.759236196406817,
24.9286439524916));
#22422=CARTESIAN_POINT('Ctrl Pts',(-1.81678410869231,-0.82360370622229,
24.9331601875065));
#22423=CARTESIAN_POINT('Ctrl Pts',(-1.78754438766915,-0.88810348942644,
24.937685703255));
#22424=CARTESIAN_POINT('Ctrl Pts',(-1.75490580504173,-0.950956441190844,
24.9422112190035));
#22425=CARTESIAN_POINT('Ctrl Pts',(-1.71909291508943,-1.01180388998527,
24.946736734752));
#22426=CARTESIAN_POINT('Ctrl Pts',(-1.69814978896887,-1.04738705001267,
24.9493832245273));
#22427=CARTESIAN_POINT('Ctrl Pts',(-1.67612192428506,-1.08228490824662,
24.9520297143025));
#22428=CARTESIAN_POINT('Ctrl Pts',(-1.65306071014841,-1.11643085368671,
24.9546762040778));
#22429=CARTESIAN_POINT('Ctrl Pts',(-1.61424871789799,-1.17389843375214,
24.9591302427958));
#22430=CARTESIAN_POINT('Ctrl Pts',(-1.57235955514502,-1.22945350124489,
24.9635842815138));
#22431=CARTESIAN_POINT('Ctrl Pts',(-1.52760818907699,-1.28274735749676,
24.9680383202318));
#22432=CARTESIAN_POINT('Ctrl Pts',(-1.48292409126539,-1.33596110480217,
24.9724856638375));
#22433=CARTESIAN_POINT('Ctrl Pts',(-1.43538664146035,-1.38692001508527,
24.9769330074433));
#22434=CARTESIAN_POINT('Ctrl Pts',(-1.3852537979361,-1.43530466375735,24.981380351049));
#22435=CARTESIAN_POINT('Ctrl Pts',(-1.33518005588115,-1.48363227190217,
24.9858224516938));
#22436=CARTESIAN_POINT('Ctrl Pts',(-1.28251734762013,-1.529391307576,24.9902645523386));
#22437=CARTESIAN_POINT('Ctrl Pts',(-1.22756237558356,-1.57229710187091,
24.9947066529834));
#22438=CARTESIAN_POINT('Ctrl Pts',(-1.17264206938682,-1.61517583100068,
24.9991459515314));
#22439=CARTESIAN_POINT('Ctrl Pts',(-1.11543275287161,-1.65520458863969,
25.0035852500794));
#22440=CARTESIAN_POINT('Ctrl Pts',(-1.05626514235829,-1.69213814788829,
25.0080245486275));
#22441=CARTESIAN_POINT('Ctrl Pts',(-0.99711474974064,-1.72906095939562,
25.0124625553305));
#22442=CARTESIAN_POINT('Ctrl Pts',(-0.936007609482037,-1.76289010146123,
25.0169005620336));
#22443=CARTESIAN_POINT('Ctrl Pts',(-0.873302942494188,-1.79342396915258,
25.0213385687367));
#22444=CARTESIAN_POINT('Ctrl Pts',(-0.81059521611902,-1.8239593266043,25.025776791972));
#22445=CARTESIAN_POINT('Ctrl Pts',(-0.746290249464193,-1.85119887829924,
25.0302150152072));
#22446=CARTESIAN_POINT('Ctrl Pts',(-0.680769740515363,-1.87498803273478,
25.0346532384425));
#22447=CARTESIAN_POINT('Ctrl Pts',(-0.615179819817879,-1.89880238915418,
25.0390961634856));
#22448=CARTESIAN_POINT('Ctrl Pts',(-0.548372247658953,-1.91915888506903,
25.0435390885286));
#22449=CARTESIAN_POINT('Ctrl Pts',(-0.480745571768988,-1.93595228704752,
25.0479820135716));
#22450=CARTESIAN_POINT('Ctrl Pts',(-0.413079419404771,-1.95275549202596,
25.0524275321329));
#22451=CARTESIAN_POINT('Ctrl Pts',(-0.34459369243018,-1.96599137029154,
25.0568730506941));
#22452=CARTESIAN_POINT('Ctrl Pts',(-0.275696111969152,-1.97560603773756,
25.0613185692554));
#22453=CARTESIAN_POINT('Ctrl Pts',(-0.206678303306874,-1.98523748304667,
25.0657718453706));
#22454=CARTESIAN_POINT('Ctrl Pts',(-0.137247694206113,-1.99123506132352,
25.0702251214858));
#22455=CARTESIAN_POINT('Ctrl Pts',(-0.0678152942088697,-1.99359691220953,
25.0746783976011));
#22456=CARTESIAN_POINT('Ctrl Pts',(-0.0306362406624794,-1.99486161543976,
25.0770629988989));
#22457=CARTESIAN_POINT('Ctrl Pts',(0.00654335154922504,-1.99508474164078,
25.0794476001968));
#22458=CARTESIAN_POINT('Ctrl Pts',(0.0436609877908849,-1.99427211800324,
25.0818322014946));
#22459=CARTESIAN_POINT('Ctrl Pts',(0.112990560449697,-1.99275427216962,
25.0862862402126));
#22460=CARTESIAN_POINT('Ctrl Pts',(0.182378190338787,-1.98761381512302,
25.0907402789306));
#22461=CARTESIAN_POINT('Ctrl Pts',(0.251414320647691,-1.97884269255372,
25.0951943176486));
#22462=CARTESIAN_POINT('Ctrl Pts',(0.320346678926507,-1.97008475434442,
25.0996416612543));
#22463=CARTESIAN_POINT('Ctrl Pts',(0.388928104586969,-1.95770704350507,
25.1040890048601));
#22464=CARTESIAN_POINT('Ctrl Pts',(0.456750377337522,-1.94175350013899,
25.1085363484659));
#22465=CARTESIAN_POINT('Ctrl Pts',(0.524492694599824,-1.92581876436071,
25.1129784491106));
#22466=CARTESIAN_POINT('Ctrl Pts',(0.591477162207732,-1.90631668020356,
25.1174205497554));
#22467=CARTESIAN_POINT('Ctrl Pts',(0.657303804424595,-1.883342579349,25.1218626504002));
#22468=CARTESIAN_POINT('Ctrl Pts',(0.723088922903924,-1.86038297065905,
25.1263019489482));
#22469=CARTESIAN_POINT('Ctrl Pts',(0.787717203715071,-1.8339558509964,25.1307412474963));
#22470=CARTESIAN_POINT('Ctrl Pts',(0.850803416763638,-1.80420650384686,
25.1351805460443));
#22471=CARTESIAN_POINT('Ctrl Pts',(0.913871271595267,-1.77446581381815,
25.1396185527474));
#22472=CARTESIAN_POINT('Ctrl Pts',(0.975397506923356,-1.74140502420487,
25.1440565594504));
#22473=CARTESIAN_POINT('Ctrl Pts',(1.03501813542709,-1.70521700139221,25.1484945661535));
#22474=CARTESIAN_POINT('Ctrl Pts',(1.09464167284673,-1.66902721295046,25.1529327893888));
#22475=CARTESIAN_POINT('Ctrl Pts',(1.15235900159095,-1.62971014444717,25.1573710126241));
#22476=CARTESIAN_POINT('Ctrl Pts',(1.20783349187974,-1.58750301366441,25.1618092358594));
#22477=CARTESIAN_POINT('Ctrl Pts',(1.26336675126887,-1.54525116908453,25.1662521609025));
#22478=CARTESIAN_POINT('Ctrl Pts',(1.31665203935131,-1.50010344823748,25.1706950859455));
#22479=CARTESIAN_POINT('Ctrl Pts',(1.36738510186496,-1.45233795849924,25.1751380109885));
#22480=CARTESIAN_POINT('Ctrl Pts',(1.41814777935539,-1.4045445860786,25.1795835295498));
#22481=CARTESIAN_POINT('Ctrl Pts',(1.46635492747801,-1.35413075719609,25.184029048111));
#22482=CARTESIAN_POINT('Ctrl Pts',(1.51174049771817,-1.30141009296026,25.1884745666723));
#22483=CARTESIAN_POINT('Ctrl Pts',(1.55720526704536,-1.24859742969361,25.1929278427875));
#22484=CARTESIAN_POINT('Ctrl Pts',(1.59983833037512,-1.1934702826931,25.1973811189028));
#22485=CARTESIAN_POINT('Ctrl Pts',(1.63941559816193,-1.13637320410302,25.201834395018));
#22486=CARTESIAN_POINT('Ctrl Pts',(1.66060808694645,-1.10579936044693,25.2042189963158));
#22487=CARTESIAN_POINT('Ctrl Pts',(1.68092515364768,-1.07466114176135,25.2066035976136));
#22488=CARTESIAN_POINT('Ctrl Pts',(1.70033786218408,-1.04301424579114,25.2089881989113));
#22489=CARTESIAN_POINT('Ctrl Pts',(1.73659757382767,-0.983903106294958,
25.2134422376293));
#22490=CARTESIAN_POINT('Ctrl Pts',(1.76984298071321,-0.922781830119846,
25.2178962763473));
#22491=CARTESIAN_POINT('Ctrl Pts',(1.79984557221022,-0.859990394536619,
25.2223503150653));
#22492=CARTESIAN_POINT('Ctrl Pts',(1.82980306515073,-0.797293344236958,
25.226797658671));
#22493=CARTESIAN_POINT('Ctrl Pts',(1.85652720794401,-0.732931555392873,
25.2312450022768));
#22494=CARTESIAN_POINT('Ctrl Pts',(1.87983392826067,-0.667272031978011,
25.2356923458826));
#22495=CARTESIAN_POINT('Ctrl Pts',(1.90311317234972,-0.601689914392275,
25.2401344465274));
#22496=CARTESIAN_POINT('Ctrl Pts',(1.92298283267127,-0.534813559932045,
25.2445765471722));
#22497=CARTESIAN_POINT('Ctrl Pts',(1.93930650845159,-0.467030864908624,
25.249018647817));
#22498=CARTESIAN_POINT('Ctrl Pts',(1.9556198871849,-0.399290927509548,25.253457946365));
#22499=CARTESIAN_POINT('Ctrl Pts',(1.96839160436379,-0.330646258564595,
25.257897244913));
#22500=CARTESIAN_POINT('Ctrl Pts',(1.97753524003519,-0.261499401374021,
25.262336543461));
#22501=CARTESIAN_POINT('Ctrl Pts',(1.9866762148899,-0.19237266606033,25.2667745501641));
#22502=CARTESIAN_POINT('Ctrl Pts',(1.99219113997979,-0.122744517695394,
25.2712125568671));
#22503=CARTESIAN_POINT('Ctrl Pts',(1.99404510212167,-0.0530254015031812,
25.2756505635702));
#22504=CARTESIAN_POINT('Ctrl Pts',(1.99589915471916,0.0166971163145512,
25.2800887868055));
#22505=CARTESIAN_POINT('Ctrl Pts',(1.99409187911962,0.0865101213204753,
25.2845270100408));
#22506=CARTESIAN_POINT('Ctrl Pts',(1.98864046260717,0.156002156977167,25.2889652332761));
#22507=CARTESIAN_POINT('Ctrl Pts',(1.98318327092055,0.225567811776531,25.2934081583192));
#22508=CARTESIAN_POINT('Ctrl Pts',(1.97407427118063,0.294811329505175,25.2978510833622));
#22509=CARTESIAN_POINT('Ctrl Pts',(1.96138255739416,0.363326335475374,25.3022940084052));
#22510=CARTESIAN_POINT('Ctrl Pts',(1.94868343493193,0.431881336474788,25.3067395269665));
#22511=CARTESIAN_POINT('Ctrl Pts',(1.93239755011193,0.499706503104474,25.3111850455277));
#22512=CARTESIAN_POINT('Ctrl Pts',(1.912644540423,0.566408354890803,25.315630564089));
#22513=CARTESIAN_POINT('Ctrl Pts',(1.89285706118077,0.633226603270421,25.3200838402042));
#22514=CARTESIAN_POINT('Ctrl Pts',(1.8695905431547,0.698917162441658,25.3245371163195));
#22515=CARTESIAN_POINT('Ctrl Pts',(1.84301334641758,0.763105082820636,25.3289903924347));
#22516=CARTESIAN_POINT('Ctrl Pts',(1.82878202183952,0.797475868345489,25.3313749937325));
#22517=CARTESIAN_POINT('Ctrl Pts',(1.81360223082304,0.831416195494785,25.3337595950303));
#22518=CARTESIAN_POINT('Ctrl Pts',(1.79750513532881,0.864871580621396,25.3361441963281));
#22519=CARTESIAN_POINT('Ctrl Pts',(1.76743843753571,0.927360677149058,25.3405982350461));
#22520=CARTESIAN_POINT('Ctrl Pts',(1.73404972190266,0.98840378608566,25.3450522737641));
#22521=CARTESIAN_POINT('Ctrl Pts',(1.69750110851537,1.04762471767761,25.3495063124821));
#22522=CARTESIAN_POINT('Ctrl Pts',(1.66100743337272,1.10675663100796,25.3539536560879));
#22523=CARTESIAN_POINT('Ctrl Pts',(1.62136354270157,1.16407139004667,25.3584009996936));
#22524=CARTESIAN_POINT('Ctrl Pts',(1.57877833891398,1.219215534299,25.3628483432994));
#22525=CARTESIAN_POINT('Ctrl Pts',(1.53624333870432,1.27429466927355,25.3672904439441));
#22526=CARTESIAN_POINT('Ctrl Pts',(1.49077421006266,1.32720788622117,25.3717325445889));
#22527=CARTESIAN_POINT('Ctrl Pts',(1.44262323073612,1.37763049350705,25.3761746452337));
#22528=CARTESIAN_POINT('Ctrl Pts',(1.39450262526062,1.42802129398891,25.3806139437817));
#22529=CARTESIAN_POINT('Ctrl Pts',(1.34370386240992,1.47592424825168,25.3850532423298));
#22530=CARTESIAN_POINT('Ctrl Pts',(1.29051859470568,1.52104875635821,25.3894925408778));
#22531=CARTESIAN_POINT('Ctrl Pts',(1.2373488040231,1.56616013314062,25.3939305475808));
#22532=CARTESIAN_POINT('Ctrl Pts',(1.18179426024702,1.6084943522703,25.3983685542839));
#22533=CARTESIAN_POINT('Ctrl Pts',(1.12418114587633,1.64779984031926,25.402806560987));
#22534=CARTESIAN_POINT('Ctrl Pts',(1.06656522053736,1.68710724609965,25.4072447842223));
#22535=CARTESIAN_POINT('Ctrl Pts',(1.00689093095456,1.72338535348979,25.4116830074576));
#22536=CARTESIAN_POINT('Ctrl Pts',(0.945513517706415,1.75642584538444,25.4161212306928));
#22537=CARTESIAN_POINT('Ctrl Pts',(0.88407108186231,1.78950134003403,25.4205641557359));
#22538=CARTESIAN_POINT('Ctrl Pts',(0.820922353042827,1.8193321407639,25.4250070807789));
#22539=CARTESIAN_POINT('Ctrl Pts',(0.756446402137609,1.84575632280999,25.4294500058219));
#22540=CARTESIAN_POINT('Ctrl Pts',(0.691932813965891,1.87219592973881,25.4338955243832));
#22541=CARTESIAN_POINT('Ctrl Pts',(0.626090923900176,1.89522479825833,25.4383410429444));
#22542=CARTESIAN_POINT('Ctrl Pts',(0.559316326762558,1.91473047949753,25.4427865615057));
#22543=CARTESIAN_POINT('Ctrl Pts',(0.492425206088981,1.93427019869498,25.4472398376209));
#22544=CARTESIAN_POINT('Ctrl Pts',(0.424598605789145,1.95027434556549,25.4516931137362));
#22545=CARTESIAN_POINT('Ctrl Pts',(0.356242919684316,1.9626814679603,25.4561463898514));
#22546=CARTESIAN_POINT('Ctrl Pts',(0.319640415465156,1.96932512521373,25.4585309911492));
#22547=CARTESIAN_POINT('Ctrl Pts',(0.282886311397865,1.97493829690981,25.460915592447));
#22548=CARTESIAN_POINT('Ctrl Pts',(0.246043286473326,1.97951768460941,25.4633001937448));
#22549=CARTESIAN_POINT('Ctrl Pts',(0.177226642091959,1.9880712193817,25.4677542324628));
#22550=CARTESIAN_POINT('Ctrl Pts',(0.107827142843297,1.99304886785181,25.4722082711807));
#22551=CARTESIAN_POINT('Ctrl Pts',(0.0382488468277091,1.99438326011235,
25.4766623098987));
#22552=CARTESIAN_POINT('Ctrl Pts',(-0.0312248621984024,1.99571564657399,
25.4811096535045));
#22553=CARTESIAN_POINT('Ctrl Pts',(-0.100876349089344,1.99341563677056,
25.4855569971102));
#22554=CARTESIAN_POINT('Ctrl Pts',(-0.170295337034419,1.98746749927749,
25.490004340716));
#22555=CARTESIAN_POINT('Ctrl Pts',(-0.239632487128338,1.98152637402712,
25.4944464413608));
#22556=CARTESIAN_POINT('Ctrl Pts',(-0.308737197238971,1.9719457045458,25.4988885420056));
#22557=CARTESIAN_POINT('Ctrl Pts',(-0.377199894270806,1.95876180334978,
25.5033306426503));
#22558=CARTESIAN_POINT('Ctrl Pts',(-0.445619404730034,1.94558621861705,
25.5077699411984));
#22559=CARTESIAN_POINT('Ctrl Pts',(-0.51339722589405,1.9288120035081,25.5122092397464));
#22560=CARTESIAN_POINT('Ctrl Pts',(-0.58013112954922,1.90852703282609,25.5166485382944));
#22561=CARTESIAN_POINT('Ctrl Pts',(-0.646845613501994,1.88824796511202,
25.5210865449975));
#22562=CARTESIAN_POINT('Ctrl Pts',(-0.712516314841297,1.86446031224138,
25.5255245517006));
#22563=CARTESIAN_POINT('Ctrl Pts',(-0.776755122245963,1.83730210976983,
25.5299625584036));
#22564=CARTESIAN_POINT('Ctrl Pts',(-0.840997063889379,1.81014258223802,
25.5344007816389));
#22565=CARTESIAN_POINT('Ctrl Pts',(-0.903806522907634,1.77961237144815,
25.5388390048742));
#22566=CARTESIAN_POINT('Ctrl Pts',(-0.964816023669794,1.74589736324047,
25.5432772281095));
#22567=CARTESIAN_POINT('Ctrl Pts',(-1.02589015726518,1.71214663770227,25.5477201531526));
#22568=CARTESIAN_POINT('Ctrl Pts',(-1.08516009726805,1.6752046177823,25.5521630781956));
#22569=CARTESIAN_POINT('Ctrl Pts',(-1.14228447074454,1.63530234219726,25.5566060032386));
#22570=CARTESIAN_POINT('Ctrl Pts',(-1.19944219006916,1.59537677401153,25.5610515217999));
#22571=CARTESIAN_POINT('Ctrl Pts',(-1.25445146379816,1.55248781183562,25.5654970403611));
#22572=CARTESIAN_POINT('Ctrl Pts',(-1.30700356997422,1.50690717384139,25.5699425589224));
#22573=CARTESIAN_POINT('Ctrl Pts',(-1.35964738104254,1.46124699636148,25.5743958350376));
#22574=CARTESIAN_POINT('Ctrl Pts',(-1.40982511283057,1.41288610660636,25.5788491111529));
#22575=CARTESIAN_POINT('Ctrl Pts',(-1.45726507255276,1.36213291231723,25.5833023872681));
#22576=CARTESIAN_POINT('Ctrl Pts',(-1.48266780676331,1.33495603627405,25.5856869885659));
#22577=CARTESIAN_POINT('Ctrl Pts',(-1.50728623044283,1.3070937844297,25.5880715898637));
#22578=CARTESIAN_POINT('Ctrl Pts',(-1.53108363525564,1.2785970688033,25.5904561911615));
#22579=CARTESIAN_POINT('Ctrl Pts',(-1.57528287205678,1.22566973946071,25.5948851429009));
#22580=CARTESIAN_POINT('Ctrl Pts',(-1.61682821605232,1.17033542805466,25.5993140946403));
#22581=CARTESIAN_POINT('Ctrl Pts',(-1.65544488032248,1.11289254230321,25.6037430463797));
#22582=CARTESIAN_POINT('Ctrl Pts',(-1.69400648819274,1.05553155379868,25.6081656836913));
#22583=CARTESIAN_POINT('Ctrl Pts',(-1.72964742212998,0.996068358787369,
25.6125883210028));
#22584=CARTESIAN_POINT('Ctrl Pts',(-1.76213257527141,0.934834931775307,
25.6170109583144));
#22585=CARTESIAN_POINT('Ctrl Pts',(-1.79458275594071,0.873667426703344,
25.6214288343568));
#22586=CARTESIAN_POINT('Ctrl Pts',(-1.82388366463736,0.81073390527048,25.6258467103991));
#22587=CARTESIAN_POINT('Ctrl Pts',(-1.84984406934354,0.74639432045973,25.6302645864415));
#22588=CARTESIAN_POINT('Ctrl Pts',(-1.87578918887268,0.682092618030071,
25.634679861291));
#22589=CARTESIAN_POINT('Ctrl Pts',(-1.89839751658755,0.616386950766104,
25.6390951361406));
#22590=CARTESIAN_POINT('Ctrl Pts',(-1.9175250249787,0.549659295455327,25.6435104109902));
#22591=CARTESIAN_POINT('Ctrl Pts',(-1.93664550425373,0.482956161709385,
25.6479240632824));
#22592=CARTESIAN_POINT('Ctrl Pts',(-1.95228757073861,0.415232262406829,
25.6523377155746));
#22593=CARTESIAN_POINT('Ctrl Pts',(-1.96435699506207,0.346884935462325,
25.6567513678668));
#22594=CARTESIAN_POINT('Ctrl Pts',(-1.97643122831788,0.278510376260323,
25.6611667787313));
#22595=CARTESIAN_POINT('Ctrl Pts',(-1.98492988835067,0.209512381281266,
25.6655821895958));
#22596=CARTESIAN_POINT('Ctrl Pts',(-1.98981009553343,0.140297349273715,
25.6699976004603));
#22597=CARTESIAN_POINT('Ctrl Pts',(-1.99314340277558,0.0930216991187449,
25.6730134398418));
#22598=CARTESIAN_POINT('Ctrl Pts',(-1.99478969175973,0.045644973009116,
25.6760292792233));
#22599=CARTESIAN_POINT('Ctrl Pts',(-1.99474927319053,-0.00170282290822489,
25.6790451186048));
#22600=CARTESIAN_POINT('',(-1.99474960167085,0.00126060858432954,24.0790451186048));
#22601=CARTESIAN_POINT('Ctrl Pts',(-1.99701539600246,0.00124451192682707,
24.0790462410754));
#22602=CARTESIAN_POINT('Ctrl Pts',(-1.99268113066523,-0.585369854447445,
24.116610900576));
#22603=CARTESIAN_POINT('Ctrl Pts',(-1.40931803204236,-1.84136072419047,
24.196560892549));
#22604=CARTESIAN_POINT('Ctrl Pts',(0.72621645117898,-2.24399041429405,24.3188962169942));
#22605=CARTESIAN_POINT('Ctrl Pts',(2.27983401216692,-0.604351048955341,
24.4460522144109));
#22606=CARTESIAN_POINT('Ctrl Pts',(1.74244183309103,1.58958477965188,24.5732082118277));
#22607=CARTESIAN_POINT('Ctrl Pts',(-0.393076711783321,2.32559111024706,
24.7003642092444));
#22608=CARTESIAN_POINT('Ctrl Pts',(-1.81615388819116,1.20559137819909,24.8023095681518));
#22609=CARTESIAN_POINT('Ctrl Pts',(-1.99314839518148,0.270951615543583,
24.861869594587));
#22610=CARTESIAN_POINT('Ctrl Pts',(-1.99194231462318,0.00100154863538889,
24.87904428855));
#22611=CARTESIAN_POINT('',(-1.9947492845807,-0.00168942735291895,23.2790451186048));
#22612=CARTESIAN_POINT('Ctrl Pts',(-1.9947492845807,-0.00168942735291895,
23.2790451186048));
#22613=CARTESIAN_POINT('Ctrl Pts',(-1.99465920403236,-0.10804979203561,
23.2858496230972));
#22614=CARTESIAN_POINT('Ctrl Pts',(-1.98605925402385,-0.214061270660987,
23.2926541275897));
#22615=CARTESIAN_POINT('Ctrl Pts',(-1.96913368264437,-0.318653577377403,
23.2994586320821));
#22616=CARTESIAN_POINT('Ctrl Pts',(-1.96731820264146,-0.329872415255579,
23.3001885006082));
#22617=CARTESIAN_POINT('Ctrl Pts',(-1.96540697249395,-0.341074954761223,
23.3009183691343));
#22618=CARTESIAN_POINT('Ctrl Pts',(-1.96340024706976,-0.352259893127804,
23.3016482376603));
#22619=CARTESIAN_POINT('Ctrl Pts',(-1.95115416107432,-0.420516225279579,
23.3061022763783));
#22620=CARTESIAN_POINT('Ctrl Pts',(-1.93532024986766,-0.488268381969719,
23.3105563150963));
#22621=CARTESIAN_POINT('Ctrl Pts',(-1.91595404076151,-0.555110508087934,
23.3150103538143));
#22622=CARTESIAN_POINT('Ctrl Pts',(-1.89661694207666,-0.621852160105046,
23.31945769742));
#22623=CARTESIAN_POINT('Ctrl Pts',(-1.87375821884304,-0.687686030136642,
23.3239050410258));
#22624=CARTESIAN_POINT('Ctrl Pts',(-1.84748455717621,-0.752215642947846,
23.3283523846315));
#22625=CARTESIAN_POINT('Ctrl Pts',(-1.82124186945576,-0.816669181978649,
23.3327944852763));
#22626=CARTESIAN_POINT('Ctrl Pts',(-1.79159242289082,-0.879821066396918,
23.3372365859211));
#22627=CARTESIAN_POINT('Ctrl Pts',(-1.75869239605651,-0.941290931940295,
23.3416786865659));
#22628=CARTESIAN_POINT('Ctrl Pts',(-1.72581312270487,-1.00272202202017,
23.3461179851139));
#22629=CARTESIAN_POINT('Ctrl Pts',(-1.68968756724518,-1.06247276742969,
23.3505572836619));
#22630=CARTESIAN_POINT('Ctrl Pts',(-1.65051897062473,-1.12018511421455,
23.35499658221));
#22631=CARTESIAN_POINT('Ctrl Pts',(-1.61136177214606,-1.1778806665884,23.359434588913));
#22632=CARTESIAN_POINT('Ctrl Pts',(-1.56916356520635,-1.23353859301894,
23.3638725956161));
#22633=CARTESIAN_POINT('Ctrl Pts',(-1.5241713057499,-1.28682920126512,23.3683106023191));
#22634=CARTESIAN_POINT('Ctrl Pts',(-1.47917685110192,-1.34012240958282,
23.3727488255544));
#22635=CARTESIAN_POINT('Ctrl Pts',(-1.43138839093273,-1.39104769787549,
23.3771870487897));
#22636=CARTESIAN_POINT('Ctrl Pts',(-1.38109245590606,-1.43930927556914,
23.381625272025));
#22637=CARTESIAN_POINT('Ctrl Pts',(-1.33074323788676,-1.48762198107834,
23.3860681970681));
#22638=CARTESIAN_POINT('Ctrl Pts',(-1.2778815969231,-1.53326500396611,23.3905111221111));
#22639=CARTESIAN_POINT('Ctrl Pts',(-1.22282944061413,-1.57598087604747,
23.3949540471541));
#22640=CARTESIAN_POINT('Ctrl Pts',(-1.16774514809551,-1.61872168314158,
23.3993995657154));
#22641=CARTESIAN_POINT('Ctrl Pts',(-1.11046819725744,-1.65853165896925,
23.4038450842766));
#22642=CARTESIAN_POINT('Ctrl Pts',(-1.05134965802129,-1.69519658419857,
23.4082906028379));
#22643=CARTESIAN_POINT('Ctrl Pts',(-0.992127955283884,-1.73192549074592,
23.4127438789531));
#22644=CARTESIAN_POINT('Ctrl Pts',(-0.931058678142455,-1.76549815544073,
23.4171971550683));
#22645=CARTESIAN_POINT('Ctrl Pts',(-0.868516949756957,-1.79574660531069,
23.4216504311836));
#22646=CARTESIAN_POINT('Ctrl Pts',(-0.835027652705715,-1.81194378036781,
23.4240350324814));
#22647=CARTESIAN_POINT('Ctrl Pts',(-0.801116498800482,-1.82718863205936,
23.4264196337792));
#22648=CARTESIAN_POINT('Ctrl Pts',(-0.766842997888278,-1.84146120759839,
23.428804235077));
#22649=CARTESIAN_POINT('Ctrl Pts',(-0.702825797107145,-1.86812000549261,
23.4332582737949));
#22650=CARTESIAN_POINT('Ctrl Pts',(-0.63728999456594,-1.8914893457816,23.4377123125129));
#22651=CARTESIAN_POINT('Ctrl Pts',(-0.570606879146275,-1.91139617870575,
23.4421663512309));
#22652=CARTESIAN_POINT('Ctrl Pts',(-0.504023998809854,-1.93127308856703,
23.4466136948367));
#22653=CARTESIAN_POINT('Ctrl Pts',(-0.436297693757557,-1.94769768217472,
23.4510610384424));
#22654=CARTESIAN_POINT('Ctrl Pts',(-0.367819064652596,-1.96054500029407,
23.4555083820482));
#22655=CARTESIAN_POINT('Ctrl Pts',(-0.299421164812397,-1.97337717274594,
23.4599504826929));
#22656=CARTESIAN_POINT('Ctrl Pts',(-0.230273181283642,-1.98264035584297,
23.4643925833377));
#22657=CARTESIAN_POINT('Ctrl Pts',(-0.160779465112124,-1.9882599241795,
23.4688346839825));
#22658=CARTESIAN_POINT('Ctrl Pts',(-0.0913295858846346,-1.99387594766742,
23.4732739825305));
#22659=CARTESIAN_POINT('Ctrl Pts',(-0.0215348934897767,-1.99585287654051,
23.4777132810786));
#22660=CARTESIAN_POINT('Ctrl Pts',(0.0481935384601513,-1.99416773250163,
23.4821525796266));
#22661=CARTESIAN_POINT('Ctrl Pts',(0.117901679293752,-1.99248307884312,
23.4865905863297));
#22662=CARTESIAN_POINT('Ctrl Pts',(0.187543108792388,-1.98713847961906,
23.4910285930327));
#22663=CARTESIAN_POINT('Ctrl Pts',(0.256706930850311,-1.97816306561249,
23.4954665997358));
#22664=CARTESIAN_POINT('Ctrl Pts',(0.325874127440659,-1.96918721369164,
23.4999048229711));
#22665=CARTESIAN_POINT('Ctrl Pts',(0.394563185144293,-1.95658026065646,
23.5043430462064));
#22666=CARTESIAN_POINT('Ctrl Pts',(0.462370284715168,-1.94042296479722,
23.5087812694417));
#22667=CARTESIAN_POINT('Ctrl Pts',(0.530249218424936,-1.92424855206611,
23.5132241944847));
#22668=CARTESIAN_POINT('Ctrl Pts',(0.597243851932029,-1.90451640304601,
23.5176671195277));
#22669=CARTESIAN_POINT('Ctrl Pts',(0.662963432335407,-1.88135776764709,
23.5221100445708));
#22670=CARTESIAN_POINT('Ctrl Pts',(0.728721375962942,-1.85818561359946,
23.526555563132));
#22671=CARTESIAN_POINT('Ctrl Pts',(0.793202332343888,-1.83158317880671,
23.5310010816933));
#22672=CARTESIAN_POINT('Ctrl Pts',(0.856036121549,-1.80172964706233,23.5354466002545));
#22673=CARTESIAN_POINT('Ctrl Pts',(0.918979557470293,-1.77182402007169,
23.5398998763698));
#22674=CARTESIAN_POINT('Ctrl Pts',(0.980269657979123,-1.73865620427228,
23.544353152485));
#22675=CARTESIAN_POINT('Ctrl Pts',(1.03956210241269,-1.7024506447258,23.5488064286002));
#22676=CARTESIAN_POINT('Ctrl Pts',(1.07131150134714,-1.68306360874395,23.5511910298981));
#22677=CARTESIAN_POINT('Ctrl Pts',(1.10248862554588,-1.66280629428665,23.5535756311959));
#22678=CARTESIAN_POINT('Ctrl Pts',(1.13304448021701,-1.64171793203028,23.5559602324937));
#22679=CARTESIAN_POINT('Ctrl Pts',(1.19011773598109,-1.60232837786275,23.5604142712117));
#22680=CARTESIAN_POINT('Ctrl Pts',(1.24524754449985,-1.55988109652507,23.5648683099297));
#22681=CARTESIAN_POINT('Ctrl Pts',(1.29808739268708,-1.51459456074781,23.5693223486477));
#22682=CARTESIAN_POINT('Ctrl Pts',(1.35084781437262,-1.46937609767012,23.5737696922535));
#22683=CARTESIAN_POINT('Ctrl Pts',(1.40132473888279,-1.42132716674313,23.5782170358592));
#22684=CARTESIAN_POINT('Ctrl Pts',(1.44920135926868,-1.3707089343817,23.582664379465));
#22685=CARTESIAN_POINT('Ctrl Pts',(1.49702153804036,-1.32015037571318,23.5871064801098));
#22686=CARTESIAN_POINT('Ctrl Pts',(1.54224716635718,-1.26702888542403,23.5915485807546));
#22687=CARTESIAN_POINT('Ctrl Pts',(1.58459658190161,-1.21164402161928,23.5959906813993));
#22688=CARTESIAN_POINT('Ctrl Pts',(1.62691928324711,-1.15629409483195,23.6004299799474));
#22689=CARTESIAN_POINT('Ctrl Pts',(1.66636907435181,-1.09868401484527,23.6048692784954));
#22690=CARTESIAN_POINT('Ctrl Pts',(1.70270407591608,-1.03914695416903,23.6093085770434));
#22691=CARTESIAN_POINT('Ctrl Pts',(1.73902850392055,-0.979627218899252,
23.6137465837465));
#22692=CARTESIAN_POINT('Ctrl Pts',(1.77223968684989,-0.91818203379965,23.6181845904496));
#22693=CARTESIAN_POINT('Ctrl Pts',(1.80213965260977,-0.85517263461335,23.6226225971526));
#22694=CARTESIAN_POINT('Ctrl Pts',(1.83204107720174,-0.792160161171581,
23.6270608203879));
#22695=CARTESIAN_POINT('Ctrl Pts',(1.85863075615744,-0.727583765436892,
23.6314990436233));
#22696=CARTESIAN_POINT('Ctrl Pts',(1.88175795509335,-0.6618266849734,23.6359372668586));
#22697=CARTESIAN_POINT('Ctrl Pts',(1.90490965474427,-0.595999942139985,
23.6403801919016));
#22698=CARTESIAN_POINT('Ctrl Pts',(1.92459139023972,-0.528990480781164,
23.6448231169446));
#22699=CARTESIAN_POINT('Ctrl Pts',(1.94070195267942,-0.461197889594338,
23.6492660419877));
#22700=CARTESIAN_POINT('Ctrl Pts',(1.95682191951755,-0.393365725081634,
23.6537115605489));
#22701=CARTESIAN_POINT('Ctrl Pts',(1.96936647599005,-0.324750002571239,
23.6581570791102));
#22702=CARTESIAN_POINT('Ctrl Pts',(1.9782858524203,-0.255758965852019,23.6626025976714));
#22703=CARTESIAN_POINT('Ctrl Pts',(1.9872207934114,-0.186647537847844,23.6670558737867));
#22704=CARTESIAN_POINT('Ctrl Pts',(1.99251788924153,-0.117159976363346,
23.6715091499019));
#22705=CARTESIAN_POINT('Ctrl Pts',(1.99417942449901,-0.0477072888013889,
23.6759624260172));
#22706=CARTESIAN_POINT('Ctrl Pts',(1.99506912884897,-0.0105173718484036,
23.6783470273149));
#22707=CARTESIAN_POINT('Ctrl Pts',(1.99491730370229,0.026662579891606,23.6807316286127));
#22708=CARTESIAN_POINT('Ctrl Pts',(1.99373040618449,0.0637701337258532,
23.6831162299105));
#22709=CARTESIAN_POINT('Ctrl Pts',(1.99151347897597,0.133080874125654,23.6875702686285));
#22710=CARTESIAN_POINT('Ctrl Pts',(1.98567353928422,0.202413136346486,23.6920243073465));
#22711=CARTESIAN_POINT('Ctrl Pts',(1.97620666341123,0.271357303179857,23.6964783460644));
#22712=CARTESIAN_POINT('Ctrl Pts',(1.96675401772357,0.340197836218457,23.7009256896702));
#22713=CARTESIAN_POINT('Ctrl Pts',(1.95368532247587,0.408650950652678,23.705373033276));
#22714=CARTESIAN_POINT('Ctrl Pts',(1.93704863226097,0.476308890065993,23.7098203768817));
#22715=CARTESIAN_POINT('Ctrl Pts',(1.92043155499376,0.543887067723278,23.7142624775265));
#22716=CARTESIAN_POINT('Ctrl Pts',(1.90025495333303,0.610671459107838,23.7187045781713));
#22717=CARTESIAN_POINT('Ctrl Pts',(1.87661818769376,0.676263070200494,23.7231466788161));
#22718=CARTESIAN_POINT('Ctrl Pts',(1.85299633223096,0.74181330581431,23.7275859773641));
#22719=CARTESIAN_POINT('Ctrl Pts',(1.82591880832445,0.806171794247129,23.7320252759121));
#22720=CARTESIAN_POINT('Ctrl Pts',(1.79553477695009,0.868954790114415,23.7364645744602));
#22721=CARTESIAN_POINT('Ctrl Pts',(1.76515958739101,0.931719516001482,23.7409025811632));
#22722=CARTESIAN_POINT('Ctrl Pts',(1.73148001363771,0.992909219018232,23.7453405878663));
#22723=CARTESIAN_POINT('Ctrl Pts',(1.69469258292169,1.05216187532633,23.7497785945693));
#22724=CARTESIAN_POINT('Ctrl Pts',(1.65790335733123,1.11141742259679,23.7542168178046));
#22725=CARTESIAN_POINT('Ctrl Pts',(1.61800623398767,1.16873532086556,23.7586550410399));
#22726=CARTESIAN_POINT('Ctrl Pts',(1.57524181337524,1.22378134970847,23.7630932642752));
#22727=CARTESIAN_POINT('Ctrl Pts',(1.53243208857855,1.27888569374419,23.7675361893183));
#22728=CARTESIAN_POINT('Ctrl Pts',(1.48674930458348,1.33171297713226,23.7719791143613));
#22729=CARTESIAN_POINT('Ctrl Pts',(1.4384746228959,1.38196176567389,23.7764220394043));
#22730=CARTESIAN_POINT('Ctrl Pts',(1.39017176128957,1.4322398865017,23.7808675579656));
#22731=CARTESIAN_POINT('Ctrl Pts',(1.33927434787408,1.47993618174905,23.7853130765268));
#22732=CARTESIAN_POINT('Ctrl Pts',(1.28609867079362,1.52478777916236,23.7897585950881));
#22733=CARTESIAN_POINT('Ctrl Pts',(1.23283020067228,1.56971764386517,23.7942118712033));
#22734=CARTESIAN_POINT('Ctrl Pts',(1.17727592103198,1.61179260600342,23.7986651473186));
#22735=CARTESIAN_POINT('Ctrl Pts',(1.11978262634189,1.65079206208501,23.8031184234338));
#22736=CARTESIAN_POINT('Ctrl Pts',(1.08899662035741,1.67167514931789,23.8055030247316));
#22737=CARTESIAN_POINT('Ctrl Pts',(1.05765509629277,1.69167716750663,23.8078876260294));
#22738=CARTESIAN_POINT('Ctrl Pts',(1.02581404086839,1.71076974372862,23.8102722273273));
#22739=CARTESIAN_POINT('Ctrl Pts',(0.966340243797557,1.74643150143895,23.8147262660453));
#22740=CARTESIAN_POINT('Ctrl Pts',(0.904886810215522,1.77905883631686,23.8191803047632));
#22741=CARTESIAN_POINT('Ctrl Pts',(0.841796004535295,1.80842667787456,23.8236343434812));
#22742=CARTESIAN_POINT('Ctrl Pts',(0.778800034138541,1.83775037500346,23.828081687087));
#22743=CARTESIAN_POINT('Ctrl Pts',(0.714172016778803,1.86382409823917,23.8325290306927));
#22744=CARTESIAN_POINT('Ctrl Pts',(0.648280794056694,1.88646748568779,23.8369763742985));
#22745=CARTESIAN_POINT('Ctrl Pts',(0.582467250313252,1.90908417891011,23.8414184749433));
#22746=CARTESIAN_POINT('Ctrl Pts',(0.515393919675886,1.92827840992859,23.8458605755881));
#22747=CARTESIAN_POINT('Ctrl Pts',(0.447450054273597,1.94391769667097,23.8503026762328));
#22748=CARTESIAN_POINT('Ctrl Pts',(0.379549048162587,1.95954711808198,23.8547419747809));
#22749=CARTESIAN_POINT('Ctrl Pts',(0.310779072626706,1.97162593421012,23.8591812733289));
#22750=CARTESIAN_POINT('Ctrl Pts',(0.241543522004278,1.98007178897074,23.8636205718769));
#22751=CARTESIAN_POINT('Ctrl Pts',(0.172328119068684,1.98851518597035,23.86805857858));
#22752=CARTESIAN_POINT('Ctrl Pts',(0.102647895712263,1.99332766105929,23.872496585283));
#22753=CARTESIAN_POINT('Ctrl Pts',(0.032913628371883,1.99447844199114,23.8769345919861));
#22754=CARTESIAN_POINT('Ctrl Pts',(-0.036824041333096,1.99562927907008,
23.8813728152214));
#22755=CARTESIAN_POINT('Ctrl Pts',(-0.106615270724014,1.99311806160853,
23.8858110384567));
#22756=CARTESIAN_POINT('Ctrl Pts',(-0.176048797512498,1.98696612537668,
23.890249261692));
#22757=CARTESIAN_POINT('Ctrl Pts',(-0.245555881460078,1.9808076718473,23.894692186735));
#22758=CARTESIAN_POINT('Ctrl Pts',(-0.314704017823341,1.97100084457308,
23.8991351117781));
#22759=CARTESIAN_POINT('Ctrl Pts',(-0.383087549361908,1.95761883215908,
23.9035780368211));
#22760=CARTESIAN_POINT('Ctrl Pts',(-0.451510999182559,1.94422900811363,
23.9080235553823));
#22761=CARTESIAN_POINT('Ctrl Pts',(-0.519168480809031,1.92725996416102,
23.9124690739436));
#22762=CARTESIAN_POINT('Ctrl Pts',(-0.585667740268369,1.90683529978573,
23.9169145925048));
#22763=CARTESIAN_POINT('Ctrl Pts',(-0.652283042791804,1.88637499380095,
23.9213678686201));
#22764=CARTESIAN_POINT('Ctrl Pts',(-0.717735628858871,1.86244719819799,
23.9258211447353));
#22765=CARTESIAN_POINT('Ctrl Pts',(-0.781652265790118,1.83522404569175,
23.9302744208505));
#22766=CARTESIAN_POINT('Ctrl Pts',(-0.815877786829699,1.82064683037504,
23.9326590221483));
#22767=CARTESIAN_POINT('Ctrl Pts',(-0.849663306511639,1.80512553783525,
23.9350436234461));
#22768=CARTESIAN_POINT('Ctrl Pts',(-0.882954658214134,1.78869187789232,
23.9374282247439));
#22769=CARTESIAN_POINT('Ctrl Pts',(-0.945137367581059,1.75799653367205,
23.9418822634619));
#22770=CARTESIAN_POINT('Ctrl Pts',(-1.00584066178244,1.72399392269352,23.9463363021799));
#22771=CARTESIAN_POINT('Ctrl Pts',(-1.06469000510462,1.68684995050844,23.9507903408979));
#22772=CARTESIAN_POINT('Ctrl Pts',(-1.1234508887202,1.64976181148471,23.9552376845036));
#22773=CARTESIAN_POINT('Ctrl Pts',(-1.1803629418952,1.6095419423325,23.9596850281094));
#22774=CARTESIAN_POINT('Ctrl Pts',(-1.2350748287984,1.5664027993363,23.9641323717151));
#22775=CARTESIAN_POINT('Ctrl Pts',(-1.28972221601077,1.52331451295543,23.9685744723599));
#22776=CARTESIAN_POINT('Ctrl Pts',(-1.34217420592638,1.47731408968489,23.9730165730047));
#22777=CARTESIAN_POINT('Ctrl Pts',(-1.39210866753241,1.42865706881712,23.9774586736495));
#22778=CARTESIAN_POINT('Ctrl Pts',(-1.44201163025885,1.38003074101367,23.9818979721975));
#22779=CARTESIAN_POINT('Ctrl Pts',(-1.48939986522325,1.32875148086676,23.9863372707455));
#22780=CARTESIAN_POINT('Ctrl Pts',(-1.53398572845433,1.27511385664122,23.9907765692935));
#22781=CARTESIAN_POINT('Ctrl Pts',(-1.57855861710803,1.22149184107403,23.9952145759966));
#22782=CARTESIAN_POINT('Ctrl Pts',(-1.62033044013214,1.16551320010519,23.9996525826996));
#22783=CARTESIAN_POINT('Ctrl Pts',(-1.65905292629981,1.10750663665553,24.0040905894027));
#22784=CARTESIAN_POINT('Ctrl Pts',(-1.69777730175411,1.04949724304087,24.008528812638));
#22785=CARTESIAN_POINT('Ctrl Pts',(-1.73345177515224,0.989460139006743,
24.0129670358733));
#22786=CARTESIAN_POINT('Ctrl Pts',(-1.76587162242856,0.927752647854771,
24.0174052591086));
#22787=CARTESIAN_POINT('Ctrl Pts',(-1.79832581495525,0.86597978442588,24.0218481841516));
#22788=CARTESIAN_POINT('Ctrl Pts',(-1.82751827133476,0.802533436113121,
24.0262911091947));
#22789=CARTESIAN_POINT('Ctrl Pts',(-1.85329089780187,0.737794287470932,
24.0307340342377));
#22790=CARTESIAN_POINT('Ctrl Pts',(-1.87907856881188,0.673017347922943,
24.0351795527989));
#22791=CARTESIAN_POINT('Ctrl Pts',(-1.90144227950406,0.606946569837811,
24.0396250713602));
#22792=CARTESIAN_POINT('Ctrl Pts',(-1.92027357612706,0.539978661919344,
24.0440705899214));
#22793=CARTESIAN_POINT('Ctrl Pts',(-1.93913773388834,0.472893893132154,
24.0485238660367));
#22794=CARTESIAN_POINT('Ctrl Pts',(-1.95445706520358,0.404909346996058,
24.0529771421519));
#22795=CARTESIAN_POINT('Ctrl Pts',(-1.96617421935367,0.336432016385155,
24.0574304182671));
#22796=CARTESIAN_POINT('Ctrl Pts',(-1.97244841845348,0.299764375030206,
24.059815019565));
#22797=CARTESIAN_POINT('Ctrl Pts',(-1.97769065557813,0.262955533534279,
24.0621996208628));
#22798=CARTESIAN_POINT('Ctrl Pts',(-1.98189826454658,0.226068200964329,
24.0645842221607));
#22799=CARTESIAN_POINT('Ctrl Pts',(-1.99040364133292,0.151503129803286,
24.0694045209754));
#22800=CARTESIAN_POINT('Ctrl Pts',(-1.99470208524478,0.0764491906303517,
24.0742248197901));
#22801=CARTESIAN_POINT('Ctrl Pts',(-1.99474960167085,0.00126060858432954,
24.0790451186048));
#22802=CARTESIAN_POINT('',(-1.99474912756561,0.0018398000541739,21.6791185974309));
#22803=CARTESIAN_POINT('Ctrl Pts',(-1.9947492527556,-0.00172659519609434,
23.2784073370651));
#22804=CARTESIAN_POINT('Ctrl Pts',(-1.99489940380178,0.171744110531787,
23.268297843062));
#22805=CARTESIAN_POINT('Ctrl Pts',(-1.9724229427003,0.34448348214041,23.2584065746183));
#22806=CARTESIAN_POINT('Ctrl Pts',(-1.92332896953422,0.529290084831314,
23.246631304765));
#22807=CARTESIAN_POINT('Ctrl Pts',(-1.9185455129571,0.546374782313945,23.2455319505099));
#22808=CARTESIAN_POINT('Ctrl Pts',(-1.90971110003626,0.576380405088859,
23.2435808450283));
#22809=CARTESIAN_POINT('Ctrl Pts',(-1.90575523383637,0.589328288229115,
23.2427321761686));
#22810=CARTESIAN_POINT('Ctrl Pts',(-1.89975144105552,0.608286380862188,
23.2414792501397));
#22811=CARTESIAN_POINT('Ctrl Pts',(-1.89780607460701,0.614328870074552,
23.2410783578602));
#22812=CARTESIAN_POINT('Ctrl Pts',(-1.89432090012929,0.624979596461161,
23.2403689486663));
#22813=CARTESIAN_POINT('Ctrl Pts',(-1.89279302839988,0.629591708662053,
23.2400608271127));
#22814=CARTESIAN_POINT('Ctrl Pts',(-1.8897764060195,0.63858760680647,23.2394580112928));
#22815=CARTESIAN_POINT('Ctrl Pts',(-1.88828921254927,0.642971885457949,
23.2391633701656));
#22816=CARTESIAN_POINT('Ctrl Pts',(-1.88424340314484,0.654763912780786,
23.2383685847191));
#22817=CARTESIAN_POINT('Ctrl Pts',(-1.88165639167996,0.662161766126466,
23.2378675020128));
#22818=CARTESIAN_POINT('Ctrl Pts',(-1.87194155807373,0.689425726641019,
23.2360115650513));
#22819=CARTESIAN_POINT('Ctrl Pts',(-1.86454237218534,0.709193002487699,
23.2346477202322));
#22820=CARTESIAN_POINT('Ctrl Pts',(-1.79906142641129,0.876016041837107,
23.2229778612225));
#22821=CARTESIAN_POINT('Ctrl Pts',(-1.72400944119378,1.01577462395414,23.2120702178011));
#22822=CARTESIAN_POINT('Ctrl Pts',(-1.60078695790284,1.19151625634831,23.1970949015526));
#22823=CARTESIAN_POINT('Ctrl Pts',(-1.56634159124751,1.23644822130391,23.19314549444));
#22824=CARTESIAN_POINT('Ctrl Pts',(-1.48694712872525,1.33136207722755,23.1846095837393));
#22825=CARTESIAN_POINT('Ctrl Pts',(-1.44128408651554,1.38066613017713,23.1800466557328));
#22826=CARTESIAN_POINT('Ctrl Pts',(-1.38659486276273,1.43403899504209,23.1750421574157));
#22827=CARTESIAN_POINT('Ctrl Pts',(-1.37992883832855,1.44045463722598,23.1744394788972));
#22828=CARTESIAN_POINT('Ctrl Pts',(-1.37102780217901,1.44890284305928,23.1736446659523));
#22829=CARTESIAN_POINT('Ctrl Pts',(-1.36883260332173,1.45097690793098,23.1734494396446));
#22830=CARTESIAN_POINT('Ctrl Pts',(-1.36478958420291,1.45477948685112,23.1730913486875));
#22831=CARTESIAN_POINT('Ctrl Pts',(-1.36294317406247,1.45650948124739,23.1729283713201));
#22832=CARTESIAN_POINT('Ctrl Pts',(-1.35911850477873,1.46007936463732,23.1725919430775));
#22833=CARTESIAN_POINT('Ctrl Pts',(-1.3571398246329,1.46191872467962,23.1724185357982));
#22834=CARTESIAN_POINT('Ctrl Pts',(-1.35259735941805,1.46612418191959,23.1720219043132));
#22835=CARTESIAN_POINT('Ctrl Pts',(-1.35003110422235,1.46848757284468,23.1717988875741));
#22836=CARTESIAN_POINT('Ctrl Pts',(-1.34329596290318,1.47465771927889,23.1712163046297));
#22837=CARTESIAN_POINT('Ctrl Pts',(-1.33911705735108,1.47845356421404,23.1708575521151));
#22838=CARTESIAN_POINT('Ctrl Pts',(-1.31169434007647,1.50315091091942,23.1685206146643));
#22839=CARTESIAN_POINT('Ctrl Pts',(-1.2879765415313,1.52352269268791,23.1665800338312));
#22840=CARTESIAN_POINT('Ctrl Pts',(-1.25485206696472,1.55064736521741,23.1639622597975));
#22841=CARTESIAN_POINT('Ctrl Pts',(-1.24585244230854,1.55788724361022,23.1632600706656));
#22842=CARTESIAN_POINT('Ctrl Pts',(-1.20586560996043,1.58948710719907,23.160177205957));
#22843=CARTESIAN_POINT('Ctrl Pts',(-1.1742218390596,1.61300480819376,23.1578346519009));
#22844=CARTESIAN_POINT('Ctrl Pts',(-1.01796422495945,1.72209864162488,23.1466195989385));
#22845=CARTESIAN_POINT('Ctrl Pts',(-0.884597707779442,1.79425837661051,
23.1380571550944));
#22846=CARTESIAN_POINT('Ctrl Pts',(-0.702479546861747,1.8675083986285,23.1263301953977));
#22847=CARTESIAN_POINT('Ctrl Pts',(-0.66004342976242,1.88292521663852,23.1235989852721));
#22848=CARTESIAN_POINT('Ctrl Pts',(-0.599569372779141,1.90259950449145,
23.1196866433448));
#22849=CARTESIAN_POINT('Ctrl Pts',(-0.581937742373893,1.9080662296082,23.1185436625259));
#22850=CARTESIAN_POINT('Ctrl Pts',(-0.550829658827688,1.9172400812361,23.1165215890655));
#22851=CARTESIAN_POINT('Ctrl Pts',(-0.537385210810333,1.9210517852363,23.1156459040899));
#22852=CARTESIAN_POINT('Ctrl Pts',(-0.517697594082466,1.92641068091167,
23.1143605636898));
#22853=CARTESIAN_POINT('Ctrl Pts',(-0.511485028323538,1.92806949425546,
23.1139545301397));
#22854=CARTESIAN_POINT('Ctrl Pts',(-0.500552758359396,1.93093195691401,
23.1132392233061));
#22855=CARTESIAN_POINT('Ctrl Pts',(-0.495836439353296,1.93214841843303,
23.1129303673742));
#22856=CARTESIAN_POINT('Ctrl Pts',(-0.486654093840431,1.93448095010188,
23.1123285145661));
#22857=CARTESIAN_POINT('Ctrl Pts',(-0.482188562561224,1.93559885898617,
23.1120355793078));
#22858=CARTESIAN_POINT('Ctrl Pts',(-0.470241675788623,1.93854575513296,
23.1112512004687));
#22859=CARTESIAN_POINT('Ctrl Pts',(-0.462753588287392,1.94034687418592,
23.1107588622567));
#22860=CARTESIAN_POINT('Ctrl Pts',(-0.435554129207192,1.9467227920117,23.1089678398856));
#22861=CARTESIAN_POINT('Ctrl Pts',(-0.415784414017754,1.95104082460511,
23.1076609571303));
#22862=CARTESIAN_POINT('Ctrl Pts',(-0.225437569174109,1.98959131143251,
23.0950250351925));
#22863=CARTESIAN_POINT('Ctrl Pts',(-0.0511697036647404,2.00166225353009,
23.0829504625356));
#22864=CARTESIAN_POINT('Ctrl Pts',(0.224179776813687,1.98473372414726,23.063712973047));
#22865=CARTESIAN_POINT('Ctrl Pts',(0.325335266638371,1.97068162455681,23.0566362422489));
#22866=CARTESIAN_POINT('Ctrl Pts',(0.439424508758674,1.94580373550329,23.0489285950421));
#22867=CARTESIAN_POINT('Ctrl Pts',(0.453832404026459,1.94249382408422,23.0479604855709));
#22868=CARTESIAN_POINT('Ctrl Pts',(0.472692289274206,1.93793985818632,23.0467013352492));
#22869=CARTESIAN_POINT('Ctrl Pts',(0.477178172348412,1.9368401811095,23.0464024466736));
#22870=CARTESIAN_POINT('Ctrl Pts',(0.484117246615384,1.93511355342052,23.0459410846895));
#22871=CARTESIAN_POINT('Ctrl Pts',(0.48657309400842,1.93449750515866,23.0457779917306));
#22872=CARTESIAN_POINT('Ctrl Pts',(0.491645179992134,1.93321490485597,23.0454415571628));
#22873=CARTESIAN_POINT('Ctrl Pts',(0.494261205674138,1.93254772568213,23.0452682583259));
#22874=CARTESIAN_POINT('Ctrl Pts',(0.500238552677646,1.93101035942966,23.0448727910667));
#22875=CARTESIAN_POINT('Ctrl Pts',(0.503598955437186,1.93013670768135,23.0446508256534));
#22876=CARTESIAN_POINT('Ctrl Pts',(0.513932494918911,1.92742132631619,23.0439693288622));
#22877=CARTESIAN_POINT('Ctrl Pts',(0.520898034804708,1.92555052378309,23.0435114483241));
#22878=CARTESIAN_POINT('Ctrl Pts',(0.577772648559834,1.90994395083988,23.0397838888185));
#22879=CARTESIAN_POINT('Ctrl Pts',(0.627144861339185,1.89430660604481,23.0366179298728));
#22880=CARTESIAN_POINT('Ctrl Pts',(0.846498534727965,1.81531332104591,23.022637599023));
#22881=CARTESIAN_POINT('Ctrl Pts',(1.00796759534284,1.73087643441346,23.0125057537943));
#22882=CARTESIAN_POINT('Ctrl Pts',(1.19198945924644,1.60004977177471,22.9990079625898));
#22883=CARTESIAN_POINT('Ctrl Pts',(1.22729861822341,1.57312931180532,22.9963205015641));
#22884=CARTESIAN_POINT('Ctrl Pts',(1.2758069467884,1.53351782076213,22.9924665092481));
#22885=CARTESIAN_POINT('Ctrl Pts',(1.2897759067463,1.52178787908598,22.9913368281267));
#22886=CARTESIAN_POINT('Ctrl Pts',(1.31405888529558,1.50082257618495,22.9893363654208));
#22887=CARTESIAN_POINT('Ctrl Pts',(1.32444141570741,1.49166822055837,22.9884688904352));
#22888=CARTESIAN_POINT('Ctrl Pts',(1.33948782066421,1.47812075616335,22.987193391538));
#22889=CARTESIAN_POINT('Ctrl Pts',(1.34422729453372,1.47381191832117,22.9867889104323));
#22890=CARTESIAN_POINT('Ctrl Pts',(1.3525312540081,1.46618909311492,22.986075389714));
#22891=CARTESIAN_POINT('Ctrl Pts',(1.35610453573722,1.46288473137947,22.9857667607986));
#22892=CARTESIAN_POINT('Ctrl Pts',(1.3630395892598,1.45642435519384,22.9851646383765));
#22893=CARTESIAN_POINT('Ctrl Pts',(1.36640258384193,1.4532696936815,22.984871203965));
#22894=CARTESIAN_POINT('Ctrl Pts',(1.37538231926807,1.44478751675164,22.9840837715075));
#22895=CARTESIAN_POINT('Ctrl Pts',(1.38097899105617,1.43943895882334,22.9835888660634));
#22896=CARTESIAN_POINT('Ctrl Pts',(1.40127097731044,1.41981929355098,22.9817791982691));
#22897=CARTESIAN_POINT('Ctrl Pts',(1.41577694970131,1.40535502803365,22.9804560145121));
#22898=CARTESIAN_POINT('Ctrl Pts',(1.54887832470058,1.26848393434861,22.9680313866217));
#22899=CARTESIAN_POINT('Ctrl Pts',(1.65152682314986,1.13159648599117,22.9562182900774));
#22900=CARTESIAN_POINT('Ctrl Pts',(1.79182953512,0.8839822124736,22.9363669834231));
#22901=CARTESIAN_POINT('Ctrl Pts',(1.83951143776093,0.779924285922606,22.9284292754728));
#22902=CARTESIAN_POINT('Ctrl Pts',(1.88074322445812,0.664753712432432,22.9204356373407));
#22903=CARTESIAN_POINT('Ctrl Pts',(1.8834149230623,0.657145956000921,22.9199112257996));
#22904=CARTESIAN_POINT('Ctrl Pts',(1.88722373872034,0.646086161423059,22.9191543151094));
#22905=CARTESIAN_POINT('Ctrl Pts',(1.88839762505644,0.642647008992073,22.9189197082477));
#22906=CARTESIAN_POINT('Ctrl Pts',(1.8904338942683,0.636627563955998,22.9185104379808));
#22907=CARTESIAN_POINT('Ctrl Pts',(1.89130040459761,0.634048691915502,22.9183355314295));
#22908=CARTESIAN_POINT('Ctrl Pts',(1.89310615953207,0.628637839473811,22.9179694702294));
#22909=CARTESIAN_POINT('Ctrl Pts',(1.89404432517614,0.625805528124738,22.917778379715));
#22910=CARTESIAN_POINT('Ctrl Pts',(1.89651003194754,0.618305251623333,22.9172737104863));
#22911=CARTESIAN_POINT('Ctrl Pts',(1.89802670573874,0.613633694480815,22.9169607680206));
#22912=CARTESIAN_POINT('Ctrl Pts',(1.90336686457588,0.59697606646518,22.9158496824772));
#22913=CARTESIAN_POINT('Ctrl Pts',(1.90709428842756,0.584959177526419,22.9150569551356));
#22914=CARTESIAN_POINT('Ctrl Pts',(1.96288578613714,0.398888545053495,22.9029063986842));
#22915=CARTESIAN_POINT('Ctrl Pts',(1.99105536719381,0.218527942337301,22.8927409605768));
#22916=CARTESIAN_POINT('Ctrl Pts',(1.99632964599413,-0.0671472086073016,
22.8760074279757));
#22917=CARTESIAN_POINT('Ctrl Pts',(1.99011646855187,-0.171093040492514,
22.8698000834706));
#22918=CARTESIAN_POINT('Ctrl Pts',(1.97379153888453,-0.288782021070179,
22.8623993525615));
#22919=CARTESIAN_POINT('Ctrl Pts',(1.97158699706026,-0.303467936998391,
22.8614693729235));
#22920=CARTESIAN_POINT('Ctrl Pts',(1.96816756465189,-0.324634321716895,
22.8601191420597));
#22921=CARTESIAN_POINT('Ctrl Pts',(1.96708416367084,-0.331135767817606,
22.8597030570557));
#22922=CARTESIAN_POINT('Ctrl Pts',(1.96513981691095,-0.342457350024902,
22.8589760877232));
#22923=CARTESIAN_POINT('Ctrl Pts',(1.96429330374573,-0.34727993428171,22.8586656641692));
#22924=CARTESIAN_POINT('Ctrl Pts',(1.96262447290281,-0.356585919235362,
22.8580651598019));
#22925=CARTESIAN_POINT('Ctrl Pts',(1.96180452575304,-0.361069718476592,
22.8577751562371));
#22926=CARTESIAN_POINT('Ctrl Pts',(1.95982398034336,-0.371694207110537,
22.8570863786607));
#22927=CARTESIAN_POINT('Ctrl Pts',(1.95864988385309,-0.377832302138153,
22.8566871764839));
#22928=CARTESIAN_POINT('Ctrl Pts',(1.95441074102143,-0.399443395158241,
22.8552771021699));
#22929=CARTESIAN_POINT('Ctrl Pts',(1.95119109208131,-0.414885127426448,
22.8542613117072));
#22930=CARTESIAN_POINT('Ctrl Pts',(1.94624691363325,-0.437266054436639,
22.8527766881474));
#22931=CARTESIAN_POINT('Ctrl Pts',(1.94466761536991,-0.444237002862461,
22.8523125252483));
#22932=CARTESIAN_POINT('Ctrl Pts',(1.90638520058454,-0.6090969456747,22.841293411604));
#22933=CARTESIAN_POINT('Ctrl Pts',(1.85061664949302,-0.761905991173004,
22.8300934346233));
#22934=CARTESIAN_POINT('Ctrl Pts',(1.74153493599781,-0.975795969344882,
22.8133413262106));
#22935=CARTESIAN_POINT('Ctrl Pts',(1.70201483118059,-1.04320108220321,22.8078978346983));
#22936=CARTESIAN_POINT('Ctrl Pts',(1.64136094097861,-1.13398841818731,22.800471181571));
#22937=CARTESIAN_POINT('Ctrl Pts',(1.62347421338004,-1.1594512392648,22.7983774952092));
#22938=CARTESIAN_POINT('Ctrl Pts',(1.59437972844739,-1.19887472761427,22.7951311061));
#22939=CARTESIAN_POINT('Ctrl Pts',(1.58356786047875,-1.21312003409577,22.7939570466494));
#22940=CARTESIAN_POINT('Ctrl Pts',(1.56952398704838,-1.23111593934856,22.7924745981308));
#22941=CARTESIAN_POINT('Ctrl Pts',(1.56646802467499,-1.23500199634667,22.7921545206208));
#22942=CARTESIAN_POINT('Ctrl Pts',(1.56154011609277,-1.24122075925653,22.791642434251));
#22943=CARTESIAN_POINT('Ctrl Pts',(1.55967734029929,-1.24356065466187,22.7914497834867));
#22944=CARTESIAN_POINT('Ctrl Pts',(1.55611145585771,-1.24801926619274,22.7910827619239));
#22945=CARTESIAN_POINT('Ctrl Pts',(1.55440929976673,-1.25013866459532,22.790908330469));
#22946=CARTESIAN_POINT('Ctrl Pts',(1.55046984493898,-1.25502329622993,22.7905063750542));
#22947=CARTESIAN_POINT('Ctrl Pts',(1.54822947924408,-1.2577860287917,22.7902790747557));
#22948=CARTESIAN_POINT('Ctrl Pts',(1.54101720620963,-1.26663145824277,22.7895514167534));
#22949=CARTESIAN_POINT('Ctrl Pts',(1.53601667299004,-1.27269087607779,22.7890530811784));
#22950=CARTESIAN_POINT('Ctrl Pts',(1.47057524992667,-1.35104225745904,22.7826087275976));
#22951=CARTESIAN_POINT('Ctrl Pts',(1.40511221180769,-1.41900371886646,22.777009669299));
#22952=CARTESIAN_POINT('Ctrl Pts',(1.20784053647726,-1.59670788465467,22.7614854606171));
#22953=CARTESIAN_POINT('Ctrl Pts',(1.06638254649067,-1.69445589350048,22.7517663922293));
#22954=CARTESIAN_POINT('Ctrl Pts',(0.881410211152412,-1.78983321367631,
22.7390576890241));
#22955=CARTESIAN_POINT('Ctrl Pts',(0.848180547462305,-1.80581737135943,
22.7367781174496));
#22956=CARTESIAN_POINT('Ctrl Pts',(0.806063898861428,-1.82465737695657,
22.7338849767244));
#22957=CARTESIAN_POINT('Ctrl Pts',(0.797572963830665,-1.82838478308745,
22.7333015208749));
#22958=CARTESIAN_POINT('Ctrl Pts',(0.784040115038235,-1.83421331694995,
22.7323711900482));
#22959=CARTESIAN_POINT('Ctrl Pts',(0.779014957207658,-1.83635320391942,
22.7320256389008));
#22960=CARTESIAN_POINT('Ctrl Pts',(0.7695391704228,-1.84034242887845,22.7313738445211));
#22961=CARTESIAN_POINT('Ctrl Pts',(0.765090495865998,-1.84219633123379,
22.7310677591127));
#22962=CARTESIAN_POINT('Ctrl Pts',(0.755074872781552,-1.84632761889957,
22.7303784410754));
#22963=CARTESIAN_POINT('Ctrl Pts',(0.749504273242664,-1.84859597611245,
22.7299949061505));
#22964=CARTESIAN_POINT('Ctrl Pts',(0.735291845640043,-1.85430849844004,
22.7290159778119));
#22965=CARTESIAN_POINT('Ctrl Pts',(0.726636100967313,-1.85771743748934,
22.7284194044127));
#22966=CARTESIAN_POINT('Ctrl Pts',(0.702825541053477,-1.86690301181164,
22.726777139125));
#22967=CARTESIAN_POINT('Ctrl Pts',(0.68762389157369,-1.87255546101241,22.7257273310065));
#22968=CARTESIAN_POINT('Ctrl Pts',(0.521421943171681,-1.93205784487764,
22.7142330279155));
#22969=CARTESIAN_POINT('Ctrl Pts',(0.364554065561413,-1.96769114330824,
22.7031638822829));
#22970=CARTESIAN_POINT('Ctrl Pts',(0.126266568804543,-1.99232873994268,
22.6864494637566));
#22971=CARTESIAN_POINT('Ctrl Pts',(0.0469604868819839,-1.99577379931077,
22.6809167662677));
#22972=CARTESIAN_POINT('Ctrl Pts',(-0.0637430796203894,-1.99397857876174,
22.6733835679092));
#22973=CARTESIAN_POINT('Ctrl Pts',(-0.095128121130232,-1.99272793566527,
22.6712696456375));
#22974=CARTESIAN_POINT('Ctrl Pts',(-0.144438823931425,-1.98959520698629,
22.6679954054893));
#22975=CARTESIAN_POINT('Ctrl Pts',(-0.16238986498644,-1.988210564608,22.6668133067906));
#22976=CARTESIAN_POINT('Ctrl Pts',(-0.185255482074356,-1.98613507194462,
22.6653222201655));
#22977=CARTESIAN_POINT('Ctrl Pts',(-0.190188887105685,-1.98566873021372,
22.6650013797042));
#22978=CARTESIAN_POINT('Ctrl Pts',(-0.19809962093472,-1.98489119681239,
22.6644883639014));
#22979=CARTESIAN_POINT('Ctrl Pts',(-0.20107803616472,-1.98459168260386,
22.6642955425731));
#22980=CARTESIAN_POINT('Ctrl Pts',(-0.206759082776146,-1.98400746703817,
22.6639283996267));
#22981=CARTESIAN_POINT('Ctrl Pts',(-0.209461773434491,-1.98372395083625,
22.6637540165225));
#22982=CARTESIAN_POINT('Ctrl Pts',(-0.215695447291557,-1.98305714766182,
22.6633524424185));
#22983=CARTESIAN_POINT('Ctrl Pts',(-0.219225990961452,-1.98266995292684,
22.6631254737005));
#22984=CARTESIAN_POINT('Ctrl Pts',(-0.230534283410593,-1.98139919754019,
22.6623999455805));
#22985=CARTESIAN_POINT('Ctrl Pts',(-0.238307993341783,-1.98047927053248,
22.6619033917045));
#22986=CARTESIAN_POINT('Ctrl Pts',(-0.331322086997792,-1.96891655200613,
22.6559862032511));
#22987=CARTESIAN_POINT('Ctrl Pts',(-0.41580669748798,-1.95282246036435,
22.6508534983321));
#22988=CARTESIAN_POINT('Ctrl Pts',(-0.594183396951104,-1.90673497566668,
22.6400436085755));
#22989=CARTESIAN_POINT('Ctrl Pts',(-0.687419122200089,-1.87513940891472,
22.6344058274439));
#22990=CARTESIAN_POINT('Ctrl Pts',(-0.871823303580205,-1.79703794755343,
22.6226977915133));
#22991=CARTESIAN_POINT('Ctrl Pts',(-0.962501982539506,-1.75014491569914,
22.6166345067782));
#22992=CARTESIAN_POINT('Ctrl Pts',(-1.06610356363666,-1.68607416129696,
22.6090857557789));
#22993=CARTESIAN_POINT('Ctrl Pts',(-1.08285599885455,-1.67536435641059,
22.6078448309455));
#22994=CARTESIAN_POINT('Ctrl Pts',(-1.10562645089442,-1.66032303942571,
22.6061287763047));
#22995=CARTESIAN_POINT('Ctrl Pts',(-1.11178495434079,-1.65620549965024,
22.6056616556944));
#22996=CARTESIAN_POINT('Ctrl Pts',(-1.12210492745288,-1.64922212683239,
22.6048737645673));
#22997=CARTESIAN_POINT('Ctrl Pts',(-1.12627873728325,-1.64637459195147,
22.6045536874333));
#22998=CARTESIAN_POINT('Ctrl Pts',(-1.13449316927295,-1.64072453262732,
22.60392091027));
#22999=CARTESIAN_POINT('Ctrl Pts',(-1.13853433774948,-1.6379228626968,22.6036082442668));
#23000=CARTESIAN_POINT('Ctrl Pts',(-1.14739679455849,-1.63173003374059,
22.602919523392));
#23001=CARTESIAN_POINT('Ctrl Pts',(-1.1522134807747,-1.62833239870155,22.6025432222784));
#23002=CARTESIAN_POINT('Ctrl Pts',(-1.16892298976981,-1.61643444073414,
22.6012308146831));
#23003=CARTESIAN_POINT('Ctrl Pts',(-1.18073714609981,-1.60782493764149,
22.6002905104766));
#23004=CARTESIAN_POINT('Ctrl Pts',(-1.19992835209821,-1.59351385715911,
22.5987422928034));
#23005=CARTESIAN_POINT('Ctrl Pts',(-1.20736208790122,-1.58788892776655,
22.5981373915182));
#23006=CARTESIAN_POINT('Ctrl Pts',(-1.34300582784669,-1.48374736444706,
22.5870032120367));
#23007=CARTESIAN_POINT('Ctrl Pts',(-1.45878315193137,-1.37007366965008,
22.5758333061371));
#23008=CARTESIAN_POINT('Ctrl Pts',(-1.60840515543387,-1.1824546710807,22.5590898808915));
#23009=CARTESIAN_POINT('Ctrl Pts',(-1.65360654159593,-1.11837063565539,
22.5536259534026));
#23010=CARTESIAN_POINT('Ctrl Pts',(-1.71136257825583,-1.02529887140285,
22.5461748860087));
#23011=CARTESIAN_POINT('Ctrl Pts',(-1.72717988718325,-0.998423514920038,
22.5440765580716));
#23012=CARTESIAN_POINT('Ctrl Pts',(-1.75108126929563,-0.955543150079855,
22.540823777461));
#23013=CARTESIAN_POINT('Ctrl Pts',(-1.7595903382555,-0.939782006625218,
22.5396478711321));
#23014=CARTESIAN_POINT('Ctrl Pts',(-1.77017731447375,-0.919523955079091,
22.5381634376108));
#23015=CARTESIAN_POINT('Ctrl Pts',(-1.77245201926606,-0.915131613110703,
22.5378431843751));
#23016=CARTESIAN_POINT('Ctrl Pts',(-1.77607615698756,-0.908069378160911,
22.5373308839325));
#23017=CARTESIAN_POINT('Ctrl Pts',(-1.7774359447346,-0.905404867243701,
22.5371381938817));
#23018=CARTESIAN_POINT('Ctrl Pts',(-1.78001986208449,-0.90031341289305,
22.5367711444385));
#23019=CARTESIAN_POINT('Ctrl Pts',(-1.78124501000241,-0.897887055965062,
22.5365967241986));
#23020=CARTESIAN_POINT('Ctrl Pts',(-1.78406139681554,-0.892280862686914,
22.5361948569657));
#23021=CARTESIAN_POINT('Ctrl Pts',(-1.78564909528378,-0.889099271462731,
22.5359676333153));
#23022=CARTESIAN_POINT('Ctrl Pts',(-1.7907144497849,-0.878880502161535,
22.5352404680016));
#23023=CARTESIAN_POINT('Ctrl Pts',(-1.79415913260376,-0.871826926368618,
22.5347425446204));
#23024=CARTESIAN_POINT('Ctrl Pts',(-1.83693946489664,-0.782899451156252,
22.5285129520476));
#23025=CARTESIAN_POINT('Ctrl Pts',(-1.87068570914006,-0.698439549331201,
22.523103492427));
#23026=CARTESIAN_POINT('Ctrl Pts',(-1.93625134309907,-0.495027903713703,
22.5105906628112));
#23027=CARTESIAN_POINT('Ctrl Pts',(-1.96305870021421,-0.374863490957609,
22.5035765390543));
#23028=CARTESIAN_POINT('Ctrl Pts',(-1.98936137568163,-0.169154360979053,
22.4913011048295));
#23029=CARTESIAN_POINT('Ctrl Pts',(-1.99474073217265,-0.0847262876506961,
22.4861927592061));
#23030=CARTESIAN_POINT('Ctrl Pts',(-1.99475112955633,0.0102038276302703,
22.4802577665153));
#23031=CARTESIAN_POINT('Ctrl Pts',(-1.99467058831744,0.0206258208173814,
22.4796036818783));
#23032=CARTESIAN_POINT('Ctrl Pts',(-1.99441052938746,0.0373326605575081,
22.4785509509724));
#23033=CARTESIAN_POINT('Ctrl Pts',(-1.99428296314659,0.0436182153457306,
22.4781539306143));
#23034=CARTESIAN_POINT('Ctrl Pts',(-1.99400396820605,0.0547668623345773,
22.4774480020702));
#23035=CARTESIAN_POINT('Ctrl Pts',(-1.99386445633228,0.059630223203031,
22.4771394694905));
#23036=CARTESIAN_POINT('Ctrl Pts',(-1.99353720471725,0.0697467317808887,
22.4764964356248));
#23037=CARTESIAN_POINT('Ctrl Pts',(-1.99334649055535,0.0749997393650962,
22.4761618434785));
#23038=CARTESIAN_POINT('Ctrl Pts',(-1.99279910155984,0.0885946860519297,
22.4752940762535));
#23039=CARTESIAN_POINT('Ctrl Pts',(-1.99241081214924,0.0969351829329676,
22.4747599144674));
#23040=CARTESIAN_POINT('Ctrl Pts',(-1.99053186476983,0.132488562882764,
22.4724751231784));
#23041=CARTESIAN_POINT('Ctrl Pts',(-1.98853601091771,0.159670707486427,
22.4707087513756));
#23042=CARTESIAN_POINT('Ctrl Pts',(-1.98188605987933,0.230369475588433,
22.4660610626453));
#23043=CARTESIAN_POINT('Ctrl Pts',(-1.97635590473971,0.273786974072694,
22.4631535490953));
#23044=CARTESIAN_POINT('Ctrl Pts',(-1.9413764756979,0.491111472763187,22.4483315183634));
#23045=CARTESIAN_POINT('Ctrl Pts',(-1.89037919748841,0.660745567678301,
22.4357970051439));
#23046=CARTESIAN_POINT('Ctrl Pts',(-1.79409402071138,0.873819015165399,
22.4197682710196));
#23047=CARTESIAN_POINT('Ctrl Pts',(-1.76816196099366,0.925169023630686,
22.4158906578821));
#23048=CARTESIAN_POINT('Ctrl Pts',(-1.73679187187874,0.981134962362514,
22.4117032482282));
#23049=CARTESIAN_POINT('Ctrl Pts',(-1.73350998349171,0.986921962846886,
22.4112707450058));
#23050=CARTESIAN_POINT('Ctrl Pts',(-1.72850361193248,0.995647746023252,
22.4106194652532));
#23051=CARTESIAN_POINT('Ctrl Pts',(-1.72680049077688,0.998598636139177,
22.4103993645986));
#23052=CARTESIAN_POINT('Ctrl Pts',(-1.7238256741348,1.00372254465682,22.4100174629333));
#23053=CARTESIAN_POINT('Ctrl Pts',(-1.72255741631258,1.00589753411517,22.4098554418575));
#23054=CARTESIAN_POINT('Ctrl Pts',(-1.71987735310241,1.01047375609972,22.4095147413663));
#23055=CARTESIAN_POINT('Ctrl Pts',(-1.71846463131751,1.01287444066157,22.4093361242915));
#23056=CARTESIAN_POINT('Ctrl Pts',(-1.71501102697897,1.01871523953045,22.4089018131834));
#23057=CARTESIAN_POINT('Ctrl Pts',(-1.71296480278288,1.02215221323185,22.4086464657524));
#23058=CARTESIAN_POINT('Ctrl Pts',(-1.70565529567986,1.03434615105033,22.4077412223584));
#23059=CARTESIAN_POINT('Ctrl Pts',(-1.70033497730051,1.04306899265292,22.4070949435868));
#23060=CARTESIAN_POINT('Ctrl Pts',(-1.66843593103339,1.09447586278817,22.4032914218129));
#23061=CARTESIAN_POINT('Ctrl Pts',(-1.64031559347395,1.13618729273205,22.4002266274959));
#23062=CARTESIAN_POINT('Ctrl Pts',(-1.55172778104536,1.25743495250759,22.3912420917059));
#23063=CARTESIAN_POINT('Ctrl Pts',(-1.48683278847187,1.33354134809347,22.3854943850943));
#23064=CARTESIAN_POINT('Ctrl Pts',(-1.3160535036731,1.50578419587836,22.3714138056933));
#23065=CARTESIAN_POINT('Ctrl Pts',(-1.20503807378247,1.59601307294226,22.3630441238972));
#23066=CARTESIAN_POINT('Ctrl Pts',(-1.07456233244342,1.68062754313318,22.3533364246023));
#23067=CARTESIAN_POINT('Ctrl Pts',(-1.06369868729427,1.68752429177564,22.3525293779118));
#23068=CARTESIAN_POINT('Ctrl Pts',(-1.04748761789267,1.69759710144086,22.3513265585637));
#23069=CARTESIAN_POINT('Ctrl Pts',(-1.04219069416228,1.7008541336746,22.3509337728373));
#23070=CARTESIAN_POINT('Ctrl Pts',(-1.0327428142645,1.70660284787424,22.350233550599));
#23071=CARTESIAN_POINT('Ctrl Pts',(-1.0285978345157,1.70910429609778,22.3499264750104));
#23072=CARTESIAN_POINT('Ctrl Pts',(-1.01986088817699,1.71433364861487,22.3492794537948));
#23073=CARTESIAN_POINT('Ctrl Pts',(-1.01526699569827,1.71705824494605,22.3489393907102));
#23074=CARTESIAN_POINT('Ctrl Pts',(-1.00313538583759,1.72418768697949,22.3480416865375));
#23075=CARTESIAN_POINT('Ctrl Pts',(-0.995579662025072,1.72856151605712,
22.3474829270845));
#23076=CARTESIAN_POINT('Ctrl Pts',(-0.961174433151073,1.74817747608927,
22.3449399319126));
#23077=CARTESIAN_POINT('Ctrl Pts',(-0.934003225952079,1.76284388845325,
22.3429351945449));
#23078=CARTESIAN_POINT('Ctrl Pts',(-0.860300200539954,1.80044481261374,
22.3375032371334));
#23079=CARTESIAN_POINT('Ctrl Pts',(-0.8131984648607,1.82220345600647,22.3340375032315));
#23080=CARTESIAN_POINT('Ctrl Pts',(-0.671797997957731,1.88094866216494,
22.3236547158045));
#23081=CARTESIAN_POINT('Ctrl Pts',(-0.575475403203092,1.91261736277786,
22.3166009573889));
#23082=CARTESIAN_POINT('Ctrl Pts',(-0.41590012443275,1.95193163595939,22.3051349263968));
#23083=CARTESIAN_POINT('Ctrl Pts',(-0.353941300566931,1.96411206290793,
22.3007373953101));
#23084=CARTESIAN_POINT('Ctrl Pts',(-0.235281884923783,1.98164080282252,
22.2925179264074));
#23085=CARTESIAN_POINT('Ctrl Pts',(-0.178720983214047,1.9875406967794,22.2886861387096));
#23086=CARTESIAN_POINT('Ctrl Pts',(-0.114627291754193,1.99146740079931,
22.2844952308409));
#23087=CARTESIAN_POINT('Ctrl Pts',(-0.107272226548183,1.99187712923906,
22.284016553547));
#23088=CARTESIAN_POINT('Ctrl Pts',(-0.0964544870976982,1.99241965939637,
22.2833159936367));
#23089=CARTESIAN_POINT('Ctrl Pts',(-0.0929935734136764,1.99258419219363,
22.2830923862285));
#23090=CARTESIAN_POINT('Ctrl Pts',(-0.0868293905717075,1.99286114404596,
22.2826950735144));
#23091=CARTESIAN_POINT('Ctrl Pts',(-0.084126305969816,1.992977081529,22.2825211725213));
#23092=CARTESIAN_POINT('Ctrl Pts',(-0.0783849786478261,1.99321163007509,
22.2821525075817));
#23093=CARTESIAN_POINT('Ctrl Pts',(-0.0753467073484952,1.99332879403751,
22.2819578259026));
#23094=CARTESIAN_POINT('Ctrl Pts',(-0.0671452677217028,1.99362628544087,
22.2814333935126));
#23095=CARTESIAN_POINT('Ctrl Pts',(-0.0619816028323414,1.99379350368177,
22.2811043708301));
#23096=CARTESIAN_POINT('Ctrl Pts',(-0.0364988061753795,1.99451963518245,
22.2794861154271));
#23097=CARTESIAN_POINT('Ctrl Pts',(-0.0161717109281678,1.99478803175302,
22.2782124501692));
#23098=CARTESIAN_POINT('Ctrl Pts',(0.041415696194476,1.9946680245351,22.2746438133625));
#23099=CARTESIAN_POINT('Ctrl Pts',(0.0786674710410893,1.99354648149933,
22.2723823904248));
#23100=CARTESIAN_POINT('Ctrl Pts',(0.215010420764463,1.98561338880275,22.2642077895884));
#23101=CARTESIAN_POINT('Ctrl Pts',(0.313589617462195,1.9724487477969,22.2584903442219));
#23102=CARTESIAN_POINT('Ctrl Pts',(0.551468306609822,1.92238890172888,22.2443805624144));
#23103=CARTESIAN_POINT('Ctrl Pts',(0.688517929913839,1.87766636357191,22.2359514793444));
#23104=CARTESIAN_POINT('Ctrl Pts',(0.831278386553244,1.81333089533958,22.2261763621779));
#23105=CARTESIAN_POINT('Ctrl Pts',(0.842942442268593,1.80793825078633,22.2253704091527));
#23106=CARTESIAN_POINT('Ctrl Pts',(0.860168933230003,1.79977098314399,22.2241689091766));
#23107=CARTESIAN_POINT('Ctrl Pts',(0.865771973903007,1.79708237797969,22.2237763395186));
#23108=CARTESIAN_POINT('Ctrl Pts',(0.87571689947265,1.79225302583458,22.2230763600458));
#23109=CARTESIAN_POINT('Ctrl Pts',(0.880063747065188,1.79012256481499,22.2227693102396));
#23110=CARTESIAN_POINT('Ctrl Pts',(0.889191862383118,1.78560744324897,22.222122197365));
#23111=CARTESIAN_POINT('Ctrl Pts',(0.893971383646201,1.7832193566189,22.2217820162824));
#23112=CARTESIAN_POINT('Ctrl Pts',(0.90654259092734,1.77687491297745,22.220883667149));
#23113=CARTESIAN_POINT('Ctrl Pts',(0.914317905637967,1.77288654147205,22.2203243778276));
#23114=CARTESIAN_POINT('Ctrl Pts',(0.94951787304008,1.75453746343677,22.2177755058577));
#23115=CARTESIAN_POINT('Ctrl Pts',(0.976630877052434,1.73959128897639,22.2157653053747));
#23116=CARTESIAN_POINT('Ctrl Pts',(1.04837939618225,1.69783349617416,22.2103149144964));
#23117=CARTESIAN_POINT('Ctrl Pts',(1.09232882632352,1.66989666927832,22.206835888048));
#23118=CARTESIAN_POINT('Ctrl Pts',(1.21852016881137,1.58256748347739,22.1964281286322));
#23119=CARTESIAN_POINT('Ctrl Pts',(1.29737946524444,1.51858962973985,22.1893627730914));
#23120=CARTESIAN_POINT('Ctrl Pts',(1.45756737938829,1.3670113913473,22.1739768007585));
#23121=CARTESIAN_POINT('Ctrl Pts',(1.53660883203062,1.27752229590784,22.1656815236915));
#23122=CARTESIAN_POINT('Ctrl Pts',(1.61171713907721,1.1753525802301,22.1574015376432));
#23123=CARTESIAN_POINT('Ctrl Pts',(1.61620292735164,1.16917660190197,22.156905362334));
#23124=CARTESIAN_POINT('Ctrl Pts',(1.62270276408493,1.16011881277242,22.1561841521045));
#23125=CARTESIAN_POINT('Ctrl Pts',(1.62474475266373,1.1572572788599,22.1559572459319));
#23126=CARTESIAN_POINT('Ctrl Pts',(1.62834881367573,1.15217839760242,22.155556195608));
#23127=CARTESIAN_POINT('Ctrl Pts',(1.62991393982904,1.14996324637169,22.1553818422289));
#23128=CARTESIAN_POINT('Ctrl Pts',(1.63320772413744,1.14528126044184,22.1550145223358));
#23129=CARTESIAN_POINT('Ctrl Pts',(1.63493530976434,1.14281370698911,22.1548216291984));
#23130=CARTESIAN_POINT('Ctrl Pts',(1.63953814260921,1.13620756732195,22.1543070451041));
#23131=CARTESIAN_POINT('Ctrl Pts',(1.64240333127733,1.13206194877011,22.1539860358096));
#23132=CARTESIAN_POINT('Ctrl Pts',(1.65593643393266,1.11232148647098,22.152466297353));
#23133=CARTESIAN_POINT('Ctrl Pts',(1.66639856674365,1.09658581167,22.1512809451576));
#23134=CARTESIAN_POINT('Ctrl Pts',(1.69483935913605,1.05246189552209,22.1480218283361));
#23135=CARTESIAN_POINT('Ctrl Pts',(1.71232739913355,1.02376347123415,22.1459749988323));
#23136=CARTESIAN_POINT('Ctrl Pts',(1.77317277487014,0.91798931282505,22.138640469828));
#23137=CARTESIAN_POINT('Ctrl Pts',(1.81212052145354,0.838491164759395,22.133518311605));
#23138=CARTESIAN_POINT('Ctrl Pts',(1.90161886261521,0.620186069472018,22.1198347949095));
#23139=CARTESIAN_POINT('Ctrl Pts',(1.94225405921951,0.477940508038958,22.1112715833456));
#23140=CARTESIAN_POINT('Ctrl Pts',(1.96915222389969,0.3188411085778,22.1012899361543));
#23141=CARTESIAN_POINT('Ctrl Pts',(1.97132262070656,0.305134795598925,22.1004272378053));
#23142=CARTESIAN_POINT('Ctrl Pts',(1.97492353201607,0.280750163991763,22.0988869070206));
#23143=CARTESIAN_POINT('Ctrl Pts',(1.9764108921075,0.270080710512796,22.0982110685707));
#23144=CARTESIAN_POINT('Ctrl Pts',(1.9786426483581,0.253064536842356,22.0971300215973));
#23145=CARTESIAN_POINT('Ctrl Pts',(1.97944310948491,0.246725281395549,22.096726582603));
#23146=CARTESIAN_POINT('Ctrl Pts',(1.98080137446067,0.235536214890278,22.0960132126866));
#23147=CARTESIAN_POINT('Ctrl Pts',(1.98137186105829,0.230687973467998,22.0957036842872));
#23148=CARTESIAN_POINT('Ctrl Pts',(1.98251467891323,0.22065874214856,22.0950624862996));
#23149=CARTESIAN_POINT('Ctrl Pts',(1.98308451013029,0.215477510251902,22.0947307404343));
#23150=CARTESIAN_POINT('Ctrl Pts',(1.98449327061911,0.202189145803423,22.0938786113204));
#23151=CARTESIAN_POINT('Ctrl Pts',(1.9853028251675,0.194079058443926,22.0933573077001));
#23152=CARTESIAN_POINT('Ctrl Pts',(1.98844201081966,0.160553171225484,22.0911970510066));
#23153=CARTESIAN_POINT('Ctrl Pts',(1.99033336811422,0.135099720064538,22.0895444119469));
#23154=CARTESIAN_POINT('Ctrl Pts',(2.00177901562873,-0.0728653863915378,
22.0759329134262));
#23155=CARTESIAN_POINT('Ctrl Pts',(1.98669331201354,-0.255832244915403,
22.0631559690902));
#23156=CARTESIAN_POINT('Ctrl Pts',(1.92596453455098,-0.528177844569036,
22.0437408037614));
#23157=CARTESIAN_POINT('Ctrl Pts',(1.89820549146989,-0.620590021843092,
22.0371051157657));
#23158=CARTESIAN_POINT('Ctrl Pts',(1.86107222929613,-0.717982881631027,
22.0302965103033));
#23159=CARTESIAN_POINT('Ctrl Pts',(1.85823050557929,-0.725305903791294,
22.0297857685802));
#23160=CARTESIAN_POINT('Ctrl Pts',(1.8540392792451,-0.735920215445776,22.0290474239287));
#23161=CARTESIAN_POINT('Ctrl Pts',(1.85272415845232,-0.73922486812476,22.0288178236047));
#23162=CARTESIAN_POINT('Ctrl Pts',(1.8503883465027,-0.745048937041736,22.0284136884696));
#23163=CARTESIAN_POINT('Ctrl Pts',(1.84937133576502,-0.747569805618463,
22.0282389333788));
#23164=CARTESIAN_POINT('Ctrl Pts',(1.84722448041796,-0.752860031488306,
22.0278725607555));
#23165=CARTESIAN_POINT('Ctrl Pts',(1.84609356197069,-0.755628922691078,
22.0276810097483));
#23166=CARTESIAN_POINT('Ctrl Pts',(1.84307666529403,-0.762968159888389,
22.0271738079769));
#23167=CARTESIAN_POINT('Ctrl Pts',(1.84117990044613,-0.767534092147903,
22.0268588049421));
#23168=CARTESIAN_POINT('Ctrl Pts',(1.83234260697776,-0.788586135251535,
22.0254087167105));
#23169=CARTESIAN_POINT('Ctrl Pts',(1.82519723301195,-0.804986109541091,
22.0242855663869));
#23170=CARTESIAN_POINT('Ctrl Pts',(1.80501732476475,-0.849652124632118,
22.0212386167411));
#23171=CARTESIAN_POINT('Ctrl Pts',(1.79153990051543,-0.87771366771119,22.0193376785394));
#23172=CARTESIAN_POINT('Ctrl Pts',(1.74195140755976,-0.975056562181382,
22.0127513654253));
#23173=CARTESIAN_POINT('Ctrl Pts',(1.70243142066826,-1.04252528738825,22.0081988487639));
#23174=CARTESIAN_POINT('Ctrl Pts',(1.56910603169086,-1.24224784100677,21.9942579734009));
#23175=CARTESIAN_POINT('Ctrl Pts',(1.46309281346152,-1.36551296241946,21.9849247614131));
#23176=CARTESIAN_POINT('Ctrl Pts',(1.33792028993777,-1.47954410902969,21.9744464321081));
#23177=CARTESIAN_POINT('Ctrl Pts',(1.33246531706927,-1.48445870585632,21.973990871058));
#23178=CARTESIAN_POINT('Ctrl Pts',(1.31530487183876,-1.49974841777872,21.9725609606724));
#23179=CARTESIAN_POINT('Ctrl Pts',(1.30350464069281,-1.51001584501153,21.9715823204737));
#23180=CARTESIAN_POINT('Ctrl Pts',(1.2868397337514,-1.52417513345275,21.9702060379645));
#23181=CARTESIAN_POINT('Ctrl Pts',(1.28207551594959,-1.52818477540374,21.9698132341926));
#23182=CARTESIAN_POINT('Ctrl Pts',(1.27379594441695,-1.53508702643795,21.9691316782757));
#23183=CARTESIAN_POINT('Ctrl Pts',(1.27028929886817,-1.53799004657729,21.968843352552));
#23184=CARTESIAN_POINT('Ctrl Pts',(1.26298756397207,-1.54399287147642,21.9682436575304));
#23185=CARTESIAN_POINT('Ctrl Pts',(1.25919093226656,-1.54709074372227,21.9679322128274));
#23186=CARTESIAN_POINT('Ctrl Pts',(1.25024316354679,-1.5543369445752,21.9671990651403));
#23187=CARTESIAN_POINT('Ctrl Pts',(1.24508275742025,-1.55847368623881,21.9667769004715));
#23188=CARTESIAN_POINT('Ctrl Pts',(1.22843564821211,-1.57168307159329,21.9654170696229));
#23189=CARTESIAN_POINT('Ctrl Pts',(1.21686983509291,-1.58065480253422,21.9644754058082));
#23190=CARTESIAN_POINT('Ctrl Pts',(1.18947054010425,-1.60142979294396,21.962251376562));
#23191=CARTESIAN_POINT('Ctrl Pts',(1.1735586707043,-1.61312663715536,21.9609649824225));
#23192=CARTESIAN_POINT('Ctrl Pts',(1.11705121195152,-1.65338679037229,21.9564136388948));
#23193=CARTESIAN_POINT('Ctrl Pts',(1.07556837204327,-1.6806675094283,21.9531021070919));
#23194=CARTESIAN_POINT('Ctrl Pts',(0.89032584162857,-1.79282170299353,21.9384452458201));
#23195=CARTESIAN_POINT('Ctrl Pts',(0.737274205600266,-1.86099586565288,
21.9265950596769));
#23196=CARTESIAN_POINT('Ctrl Pts',(0.522204827353338,-1.92605067653363,
21.9111891200183));
#23197=CARTESIAN_POINT('Ctrl Pts',(0.466167120640786,-1.94037592805868,
21.9072897016726));
#23198=CARTESIAN_POINT('Ctrl Pts',(0.403062289609456,-1.95361529297327,
21.9030813074586));
#23199=CARTESIAN_POINT('Ctrl Pts',(0.396536969877108,-1.95495021849559,
21.9026483029122));
#23200=CARTESIAN_POINT('Ctrl Pts',(0.386661744634067,-1.95691897614008,
21.9019963978943));
#23201=CARTESIAN_POINT('Ctrl Pts',(0.38331677988225,-1.95757692840498,21.9017761697802));
#23202=CARTESIAN_POINT('Ctrl Pts',(0.377498005163986,-1.95870599121408,
21.9013941089536));
#23203=CARTESIAN_POINT('Ctrl Pts',(0.375024972632849,-1.95918099572151,
21.9012320557287));
#23204=CARTESIAN_POINT('Ctrl Pts',(0.369815058781727,-1.96017145701136,
21.9008913558898));
#23205=CARTESIAN_POINT('Ctrl Pts',(0.367077988510799,-1.9606858670086,21.9007127714055));
#23206=CARTESIAN_POINT('Ctrl Pts',(0.360409763285189,-1.96192465287333,
21.90027865878));
#23207=CARTESIAN_POINT('Ctrl Pts',(0.356477463871933,-1.96264295261523,
21.9000234764867));
#23208=CARTESIAN_POINT('Ctrl Pts',(0.342994459046092,-1.96506398819669,
21.8991512272462));
#23209=CARTESIAN_POINT('Ctrl Pts',(0.333433316318281,-1.96670890304321,
21.8985373579226));
#23210=CARTESIAN_POINT('Ctrl Pts',(0.209132038555653,-1.98716136380694,
21.8906126699653));
#23211=CARTESIAN_POINT('Ctrl Pts',(0.092954056282022,-1.99597455346449,
21.8838179988577));
#23212=CARTESIAN_POINT('Ctrl Pts',(-0.13839933914818,-1.99326679365454,
21.8703798108761));
#23213=CARTESIAN_POINT('Ctrl Pts',(-0.253114545077029,-1.98196824158015,
21.8637553110501));
#23214=CARTESIAN_POINT('Ctrl Pts',(-0.384208110501742,-1.95748481326619,
21.8557727631345));
#23215=CARTESIAN_POINT('Ctrl Pts',(-0.402155310732573,-1.95387659408648,
21.8546711864521));
#23216=CARTESIAN_POINT('Ctrl Pts',(-0.466372986767495,-1.94004360540612,
21.8506941267411));
#23217=CARTESIAN_POINT('Ctrl Pts',(-0.512322527213875,-1.9284185286809,
21.847781558384));
#23218=CARTESIAN_POINT('Ctrl Pts',(-0.566958514744587,-1.91250525790726,
21.8442194085392));
#23219=CARTESIAN_POINT('Ctrl Pts',(-0.576085736579041,-1.90977578213628,
21.8436209887834));
#23220=CARTESIAN_POINT('Ctrl Pts',(-0.591008981218374,-1.90519630443585,
21.8426369181211));
#23221=CARTESIAN_POINT('Ctrl Pts',(-0.596816782435865,-1.90338495874766,
21.842252532972));
#23222=CARTESIAN_POINT('Ctrl Pts',(-0.607216729445446,-1.90008912867734,
21.8415616567058));
#23223=CARTESIAN_POINT('Ctrl Pts',(-0.611811964410745,-1.89861448771706,
21.8412554910312));
#23224=CARTESIAN_POINT('Ctrl Pts',(-0.62155427073647,-1.89544907659638,
21.8406044578399));
#23225=CARTESIAN_POINT('Ctrl Pts',(-0.626699887532937,-1.89375398704581,
21.8402594500284));
#23226=CARTESIAN_POINT('Ctrl Pts',(-0.639904168049234,-1.88934447051319,
21.8393711262455));
#23227=CARTESIAN_POINT('Ctrl Pts',(-0.647952431057276,-1.88659945826284,
21.8388268032043));
#23228=CARTESIAN_POINT('Ctrl Pts',(-0.685029326964789,-1.87368844557313,
21.836305714693));
#23229=CARTESIAN_POINT('Ctrl Pts',(-0.713836594352723,-1.86290383829853,
21.8343085239392));
#23230=CARTESIAN_POINT('Ctrl Pts',(-0.790478718656267,-1.83217253765312,
21.8288875984377));
#23231=CARTESIAN_POINT('Ctrl Pts',(-0.837802100439806,-1.81102172129554,
21.8254252955133));
#23232=CARTESIAN_POINT('Ctrl Pts',(-0.980442748138354,-1.74048173800657,
21.8146352932242));
#23233=CARTESIAN_POINT('Ctrl Pts',(-1.07263676033614,-1.68522735339636,
21.8071466913429));
#23234=CARTESIAN_POINT('Ctrl Pts',(-1.17425054468235,-1.6125982230581,21.7984354376002));
#23235=CARTESIAN_POINT('Ctrl Pts',(-1.18843416884133,-1.60217402439918,
21.7972086818905));
#23236=CARTESIAN_POINT('Ctrl Pts',(-1.27878421140073,-1.53391162155286,
21.7893307632562));
#23237=CARTESIAN_POINT('Ctrl Pts',(-1.35085598275733,-1.47083880874594,
21.7827466800504));
#23238=CARTESIAN_POINT('Ctrl Pts',(-1.4236556634689,-1.39724508503005,21.7759847301797));
#23239=CARTESIAN_POINT('Ctrl Pts',(-1.42914739877409,-1.39162746211556,
21.7754739266258));
#23240=CARTESIAN_POINT('Ctrl Pts',(-1.43707726103172,-1.38341937226122,
21.7747355093503));
#23241=CARTESIAN_POINT('Ctrl Pts',(-1.43954178635455,-1.38085468444104,
21.7745058976897));
#23242=CARTESIAN_POINT('Ctrl Pts',(-1.44387767942877,-1.37631834923807,
21.7741017495179));
#23243=CARTESIAN_POINT('Ctrl Pts',(-1.44575189273671,-1.37434945214526,
21.7739269926804));
#23244=CARTESIAN_POINT('Ctrl Pts',(-1.44967977958317,-1.3702062049999,21.7735606237776));
#23245=CARTESIAN_POINT('Ctrl Pts',(-1.45173258486281,-1.36803107051301,
21.7733690782093));
#23246=CARTESIAN_POINT('Ctrl Pts',(-1.45590620702771,-1.36358876372386,
21.7729794720103));
#23247=CARTESIAN_POINT('Ctrl Pts',(-1.45802663978856,-1.361321239898,21.7727814408053));
#23248=CARTESIAN_POINT('Ctrl Pts',(-1.46705016042496,-1.35162650342268,
21.7719382861313));
#23249=CARTESIAN_POINT('Ctrl Pts',(-1.47390201309046,-1.34415149596916,
21.7712969706654));
#23250=CARTESIAN_POINT('Ctrl Pts',(-1.55687083527858,-1.25223961221706,
21.7635131944535));
#23251=CARTESIAN_POINT('Ctrl Pts',(-1.62570413458052,-1.16148387067856,
21.7568613529895));
#23252=CARTESIAN_POINT('Ctrl Pts',(-1.71020123021507,-1.02772530334523,
21.7476691445891));
#23253=CARTESIAN_POINT('Ctrl Pts',(-1.73270050868412,-0.989321230798476,
21.745094368668));
#23254=CARTESIAN_POINT('Ctrl Pts',(-1.77380547893419,-0.913448674272355,
21.7400788966662));
#23255=CARTESIAN_POINT('Ctrl Pts',(-1.79255400984957,-0.87608465676867,
21.7376408523234));
#23256=CARTESIAN_POINT('Ctrl Pts',(-1.84922249582413,-0.753701777756611,
21.7296964005963));
#23257=CARTESIAN_POINT('Ctrl Pts',(-1.88236647669968,-0.666620718928333,
21.7240995234148));
#23258=CARTESIAN_POINT('Ctrl Pts',(-1.91296509429747,-0.565465780779629,
21.7175005481069));
#23259=CARTESIAN_POINT('Ctrl Pts',(-1.91650612760227,-0.553345509072535,
21.7167084626777));
#23260=CARTESIAN_POINT('Ctrl Pts',(-1.92160594335428,-0.535253433520577,
21.7155237045835));
#23261=CARTESIAN_POINT('Ctrl Pts',(-1.92325251424397,-0.529306531882967,
21.7151338882961));
#23262=CARTESIAN_POINT('Ctrl Pts',(-1.92614013589272,-0.518685957228025,
21.7144369919139));
#23263=CARTESIAN_POINT('Ctrl Pts',(-1.9273918406919,-0.514015210944063,
21.7141302601834));
#23264=CARTESIAN_POINT('Ctrl Pts',(-1.92999691070707,-0.504151058822975,
21.7134819284136));
#23265=CARTESIAN_POINT('Ctrl Pts',(-1.93134632271255,-0.49895665770441,
21.713140203132));
#23266=CARTESIAN_POINT('Ctrl Pts',(-1.93404538683843,-0.488391918446066,
21.7124445080554));
#23267=CARTESIAN_POINT('Ctrl Pts',(-1.93539367155762,-0.483021282579187,
21.7120904973733));
#23268=CARTESIAN_POINT('Ctrl Pts',(-1.93868131223518,-0.469690804783977,
21.7112109066444));
#23269=CARTESIAN_POINT('Ctrl Pts',(-1.94059401121295,-0.461724552977374,
21.7106844725305));
#23270=CARTESIAN_POINT('Ctrl Pts',(-1.94955530046714,-0.423361918956064,
21.7081453760436));
#23271=CARTESIAN_POINT('Ctrl Pts',(-1.95593876719981,-0.392816165863748,
21.7061115732804));
#23272=CARTESIAN_POINT('Ctrl Pts',(-1.98377047680234,-0.242057975678065,
21.6960092438615));
#23273=CARTESIAN_POINT('Ctrl Pts',(-1.99486174452552,-0.120222041741954,
21.6876218107719));
#23274=CARTESIAN_POINT('Ctrl Pts',(-1.99474915136507,0.00184000770332437,
21.6791186215938));
#23275=CARTESIAN_POINT('',(-1.99474949799968,-0.00141517844896885,20.0802123525403));
#23276=CARTESIAN_POINT('Ctrl Pts',(-1.99474915155411,0.00183980275410899,
21.6791186358711));
#23277=CARTESIAN_POINT('Ctrl Pts',(-1.99462759772053,0.133630781894563,
21.6699377018992));
#23278=CARTESIAN_POINT('Ctrl Pts',(-1.98144558057616,0.265099377212311,
21.6606648776704));
#23279=CARTESIAN_POINT('Ctrl Pts',(-1.95303028307935,0.406007963953111,
21.6511398820363));
#23280=CARTESIAN_POINT('Ctrl Pts',(-1.9505682576785,0.41767600052295,21.6503545061792));
#23281=CARTESIAN_POINT('Ctrl Pts',(-1.94671784351141,0.43514685143171,21.6491842770525));
#23282=CARTESIAN_POINT('Ctrl Pts',(-1.94540786422072,0.440966425620485,
21.6487954298911));
#23283=CARTESIAN_POINT('Ctrl Pts',(-1.94325117019873,0.450350835919816,
21.6481700354034));
#23284=CARTESIAN_POINT('Ctrl Pts',(-1.94242071682887,0.453919315783123,
21.6479326100637));
#23285=CARTESIAN_POINT('Ctrl Pts',(-1.94080367432097,0.460782086162704,
21.6474767699827));
#23286=CARTESIAN_POINT('Ctrl Pts',(-1.9400185186105,0.464076697380762,21.6472582758597));
#23287=CARTESIAN_POINT('Ctrl Pts',(-1.93865430964199,0.469737120445104,
21.6468834900377));
#23288=CARTESIAN_POINT('Ctrl Pts',(-1.93807931257185,0.472103879499661,
21.6467269660816));
#23289=CARTESIAN_POINT('Ctrl Pts',(-1.93686976671853,0.477043068363232,
21.6464007020923));
#23290=CARTESIAN_POINT('Ctrl Pts',(-1.93623442988505,0.479615278145238,
21.646231008808));
#23291=CARTESIAN_POINT('Ctrl Pts',(-1.93445094332048,0.486774557272059,
21.6457592836481));
#23292=CARTESIAN_POINT('Ctrl Pts',(-1.93329159566434,0.491358859654482,
21.6454578935852));
#23293=CARTESIAN_POINT('Ctrl Pts',(-1.9285656395357,0.509770588137588,21.6442499687596));
#23294=CARTESIAN_POINT('Ctrl Pts',(-1.92486679127725,0.523564076647532,
21.6433507844798));
#23295=CARTESIAN_POINT('Ctrl Pts',(-1.88703483710921,0.65882114891643,21.6345794691881));
#23296=CARTESIAN_POINT('Ctrl Pts',(-1.841593303974,0.776845759596387,21.6272805479765));
#23297=CARTESIAN_POINT('Ctrl Pts',(-1.75721828361801,0.946136240089996,
21.6163102568148));
#23298=CARTESIAN_POINT('Ctrl Pts',(-1.72648908104309,1.00111189485545,21.6126629290317));
#23299=CARTESIAN_POINT('Ctrl Pts',(-1.64525247806218,1.13154856728356,21.6036318904546));
#23300=CARTESIAN_POINT('Ctrl Pts',(-1.59210035721319,1.20518515254058,21.5981991448856));
#23301=CARTESIAN_POINT('Ctrl Pts',(-1.52279643770028,1.28857783195248,21.5914664353033));
#23302=CARTESIAN_POINT('Ctrl Pts',(-1.51128509631546,1.3020595782912,21.5903586761523));
#23303=CARTESIAN_POINT('Ctrl Pts',(-1.49598191381535,1.31950585898312,21.5888987743151));
#23304=CARTESIAN_POINT('Ctrl Pts',(-1.49235100810189,1.32361099496857,21.5885533090356));
#23305=CARTESIAN_POINT('Ctrl Pts',(-1.48515745745297,1.33167686343929,21.587870643137));
#23306=CARTESIAN_POINT('Ctrl Pts',(-1.4815957705789,1.33563839183819,21.5875334842059));
#23307=CARTESIAN_POINT('Ctrl Pts',(-1.47476481155392,1.34317526185204,21.5868884254635));
#23308=CARTESIAN_POINT('Ctrl Pts',(-1.47149829490288,1.34675305860667,21.586580643552));
#23309=CARTESIAN_POINT('Ctrl Pts',(-1.46399139605767,1.35491540460037,21.5858748488138));
#23310=CARTESIAN_POINT('Ctrl Pts',(-1.45974247003781,1.35949199374472,21.5854764730848));
#23311=CARTESIAN_POINT('Ctrl Pts',(-1.44657949648695,1.37353719917973,21.5842456582888));
#23312=CARTESIAN_POINT('Ctrl Pts',(-1.43759443334741,1.38293850516904,21.5834101677385));
#23313=CARTESIAN_POINT('Ctrl Pts',(-1.34398365286598,1.47898778041756,21.5747517918442));
#23314=CARTESIAN_POINT('Ctrl Pts',(-1.25174131841775,1.55782889500527,21.5665805912205));
#23315=CARTESIAN_POINT('Ctrl Pts',(-1.06112392158137,1.69283842659526,21.5504230932594));
#23316=CARTESIAN_POINT('Ctrl Pts',(-0.963976243073012,1.74998151417476,
21.5424977399265));
#23317=CARTESIAN_POINT('Ctrl Pts',(-0.823115605134974,1.81753102802609,
21.5317570132323));
#23318=CARTESIAN_POINT('Ctrl Pts',(-0.783087369271146,1.83513297866075,
21.5287849896786));
#23319=CARTESIAN_POINT('Ctrl Pts',(-0.728556341170191,1.8570027612317,21.5248706935772));
#23320=CARTESIAN_POINT('Ctrl Pts',(-0.714538960654169,1.86244132843294,
21.5238762144651));
#23321=CARTESIAN_POINT('Ctrl Pts',(-0.690828942538745,1.87133341752682,
21.5222152715546));
#23322=CARTESIAN_POINT('Ctrl Pts',(-0.681168869294488,1.87487129421083,
21.5215444259801));
#23323=CARTESIAN_POINT('Ctrl Pts',(-0.668558241381134,1.87937943977441,
21.5206766900429));
#23324=CARTESIAN_POINT('Ctrl Pts',(-0.665632410930428,1.8804176915253,21.5204759228869));
#23325=CARTESIAN_POINT('Ctrl Pts',(-0.659883136138226,1.88244276262535,
21.5200825273207));
#23326=CARTESIAN_POINT('Ctrl Pts',(-0.65705987365359,1.88343007054796,21.5198898706161));
#23327=CARTESIAN_POINT('Ctrl Pts',(-0.651666434277915,1.88530257787059,
21.5195228448407));
#23328=CARTESIAN_POINT('Ctrl Pts',(-0.649096700003978,1.88618886271008,
21.5193484150846));
#23329=CARTESIAN_POINT('Ctrl Pts',(-0.643160385905131,1.88822269100933,
21.5189464730168));
#23330=CARTESIAN_POINT('Ctrl Pts',(-0.639792543807331,1.88936648488526,
21.5187191843183));
#23331=CARTESIAN_POINT('Ctrl Pts',(-0.628977040069291,1.89300743482387,
21.5179916008935));
#23332=CARTESIAN_POINT('Ctrl Pts',(-0.621517564887757,1.89546964804969,
21.5174933277134));
#23333=CARTESIAN_POINT('Ctrl Pts',(-0.525362643226921,1.9265796610077,21.5111135710746));
#23334=CARTESIAN_POINT('Ctrl Pts',(-0.434766279784053,1.94902498030959,
21.5055714981401));
#23335=CARTESIAN_POINT('Ctrl Pts',(-0.210135339865238,1.98822523236754,
21.4922336607228));
#23336=CARTESIAN_POINT('Ctrl Pts',(-0.0753480564502597,1.99787856835567,
21.4845497530724));
#23337=CARTESIAN_POINT('Ctrl Pts',(0.127077534222631,1.99184976507782,21.4724709923917));
#23338=CARTESIAN_POINT('Ctrl Pts',(0.194618998963505,1.98638770982028,21.4683552932056));
#23339=CARTESIAN_POINT('Ctrl Pts',(0.274603870970788,1.97580071609844,21.4633203341471));
#23340=CARTESIAN_POINT('Ctrl Pts',(0.287443516497159,1.97397364923387,21.4625071843974));
#23341=CARTESIAN_POINT('Ctrl Pts',(0.306530047981177,1.97106749333816,21.4612907473473));
#23342=CARTESIAN_POINT('Ctrl Pts',(0.312791257224153,1.97008359251791,21.4608904722861));
#23343=CARTESIAN_POINT('Ctrl Pts',(0.323842302991212,1.96829299594639,21.4601817676285));
#23344=CARTESIAN_POINT('Ctrl Pts',(0.328634104398711,1.96749860987008,21.4598737307615));
#23345=CARTESIAN_POINT('Ctrl Pts',(0.337990731419987,1.96591233084261,21.4592707853869));
#23346=CARTESIAN_POINT('Ctrl Pts',(0.34255579679748,1.96512201976582,21.4589759289756));
#23347=CARTESIAN_POINT('Ctrl Pts',(0.354852389765219,1.96294906511074,21.4581798356736));
#23348=CARTESIAN_POINT('Ctrl Pts',(0.362578510546136,1.96153666076045,21.4576776548471));
#23349=CARTESIAN_POINT('Ctrl Pts',(0.391142134159139,1.95614045110115,21.4558136008388));
#23350=CARTESIAN_POINT('Ctrl Pts',(0.411923414949782,1.95187004586243,21.4544426357739));
#23351=CARTESIAN_POINT('Ctrl Pts',(0.582951299979936,1.91387214823501,21.4430331003788));
#23352=CARTESIAN_POINT('Ctrl Pts',(0.728868893390707,1.86318835959631,21.4324270674748));
#23353=CARTESIAN_POINT('Ctrl Pts',(0.97475916852336,1.74443854889997,21.4133776461433));
#23354=CARTESIAN_POINT('Ctrl Pts',(1.07719425592596,1.68311596531382,21.4050433423637));
#23355=CARTESIAN_POINT('Ctrl Pts',(1.18219795034365,1.60672023660532,21.3964589178389));
#23356=CARTESIAN_POINT('Ctrl Pts',(1.19079447555452,1.60035947246432,21.3957559180322));
#23357=CARTESIAN_POINT('Ctrl Pts',(1.20563218159969,1.58919495946227,21.3945427639548));
#23358=CARTESIAN_POINT('Ctrl Pts',(1.21189674950765,1.58442287600956,21.3940306361421));
#23359=CARTESIAN_POINT('Ctrl Pts',(1.22101616044616,1.5773903620465,21.3932854333068));
#23360=CARTESIAN_POINT('Ctrl Pts',(1.22389323897372,1.57515908988853,21.3930503748909));
#23361=CARTESIAN_POINT('Ctrl Pts',(1.22891025291307,1.57124618048337,21.3926405861212));
#23362=CARTESIAN_POINT('Ctrl Pts',(1.23105287549119,1.56956802576634,21.3924656107257));
#23363=CARTESIAN_POINT('Ctrl Pts',(1.23553471527144,1.56604291535272,21.392099683946));
#23364=CARTESIAN_POINT('Ctrl Pts',(1.23787322491147,1.5641951044229,21.3919087956394));
#23365=CARTESIAN_POINT('Ctrl Pts',(1.24404320656702,1.55929729207249,21.3914052385379));
#23366=CARTESIAN_POINT('Ctrl Pts',(1.2478676335518,1.55623838637607,21.3910932009757));
#23367=CARTESIAN_POINT('Ctrl Pts',(1.26382983014862,1.54337460815747,21.3897910242636));
#23368=CARTESIAN_POINT('Ctrl Pts',(1.27586401227092,1.53344125386396,21.388809751128));
#23369=CARTESIAN_POINT('Ctrl Pts',(1.44891848972545,1.38714939549097,21.374684755799));
#23370=CARTESIAN_POINT('Ctrl Pts',(1.58744919667585,1.22620795374632,21.3630788430112));
#23371=CARTESIAN_POINT('Ctrl Pts',(1.72510128599185,1.00283842887616,21.3474864507092));
#23372=CARTESIAN_POINT('Ctrl Pts',(1.7503189590019,0.958145238245635,21.3443965305516));
#23373=CARTESIAN_POINT('Ctrl Pts',(1.78779648616265,0.885296228959564,21.3393682580237));
#23374=CARTESIAN_POINT('Ctrl Pts',(1.8011783755114,0.857742379244277,21.3374683670956));
#23375=CARTESIAN_POINT('Ctrl Pts',(1.8175420926116,0.821975728509637,21.335000032784));
#23376=CARTESIAN_POINT('Ctrl Pts',(1.82111220174292,0.814035442389179,21.3344519293608));
#23377=CARTESIAN_POINT('Ctrl Pts',(1.82678630487332,0.801191505402095,21.333565025075));
#23378=CARTESIAN_POINT('Ctrl Pts',(1.82892282846319,0.796302278425035,21.3332273403366));
#23379=CARTESIAN_POINT('Ctrl Pts',(1.83296096734602,0.786959405261308,21.3325818916934));
#23380=CARTESIAN_POINT('Ctrl Pts',(1.8348660337925,0.782507284757336,21.3322742482807));
#23381=CARTESIAN_POINT('Ctrl Pts',(1.83918429535329,0.772313074634138,21.331569641413));
#23382=CARTESIAN_POINT('Ctrl Pts',(1.84158683632246,0.766566553114736,21.3311723193739));
#23383=CARTESIAN_POINT('Ctrl Pts',(1.84889046704608,0.748864841194824,21.3299479377961));
#23384=CARTESIAN_POINT('Ctrl Pts',(1.85370226684932,0.736873396404387,21.3291178727971));
#23385=CARTESIAN_POINT('Ctrl Pts',(1.89849228752855,0.622036917646174,21.3211612599407));
#23386=CARTESIAN_POINT('Ctrl Pts',(1.92998181685044,0.516106215679385,21.3137484108569));
#23387=CARTESIAN_POINT('Ctrl Pts',(1.98774568646514,0.239756896093602,21.2942944754034));
#23388=CARTESIAN_POINT('Ctrl Pts',(2.00101357841623,0.0675416382083606,
21.2820223710285));
#23389=CARTESIAN_POINT('Ctrl Pts',(1.99105200394158,-0.122824311525504,
21.2693810509212));
#23390=CARTESIAN_POINT('Ctrl Pts',(1.98981942828649,-0.141395184833082,
21.2681584811593));
#23391=CARTESIAN_POINT('Ctrl Pts',(1.98792511663006,-0.164943695799032,
21.2666240010388));
#23392=CARTESIAN_POINT('Ctrl Pts',(1.98750431918883,-0.169939032133866,
21.266299395568));
#23393=CARTESIAN_POINT('Ctrl Pts',(1.98680104824651,-0.177927499136992,
21.2657817936845));
#23394=CARTESIAN_POINT('Ctrl Pts',(1.98653063528956,-0.180921628372104,
21.2655881309913));
#23395=CARTESIAN_POINT('Ctrl Pts',(1.98600323401925,-0.186617475299121,
21.2652203767007));
#23396=CARTESIAN_POINT('Ctrl Pts',(1.98574750424957,-0.189319246431959,
21.2650462195482));
#23397=CARTESIAN_POINT('Ctrl Pts',(1.985146785305,-0.195530661356432,21.2646464696675));
#23398=CARTESIAN_POINT('Ctrl Pts',(1.98479800262249,-0.199039915570191,
21.2644210926037));
#23399=CARTESIAN_POINT('Ctrl Pts',(1.98365882239871,-0.210200883880464,
21.2637057346359));
#23400=CARTESIAN_POINT('Ctrl Pts',(1.98283345749588,-0.21784907554564,21.2632176809555));
#23401=CARTESIAN_POINT('Ctrl Pts',(1.96892322175888,-0.340112967079147,
21.2554473958506));
#23402=CARTESIAN_POINT('Ctrl Pts',(1.94596178663907,-0.453405713915335,
21.2486874262964));
#23403=CARTESIAN_POINT('Ctrl Pts',(1.88430469459147,-0.662538632997183,
21.2360149422177));
#23404=CARTESIAN_POINT('Ctrl Pts',(1.84772715469179,-0.758594137701845,
21.2301083824523));
#23405=CARTESIAN_POINT('Ctrl Pts',(1.7810072939806,-0.899957090405861,21.2208365044465));
#23406=CARTESIAN_POINT('Ctrl Pts',(1.75614376346414,-0.947559046685419,
21.2176084702422));
#23407=CARTESIAN_POINT('Ctrl Pts',(1.71361803042075,-1.02153936378006,21.2123755073278));
#23408=CARTESIAN_POINT('Ctrl Pts',(1.69719374588583,-1.04860032397429,21.210413202833));
#23409=CARTESIAN_POINT('Ctrl Pts',(1.67538616342487,-1.08267553855334,21.2078747119729));
#23410=CARTESIAN_POINT('Ctrl Pts',(1.67059002181998,-1.09006150898332,21.2073203357143));
#23411=CARTESIAN_POINT('Ctrl Pts',(1.66279743383105,-1.10188972476269,21.2064257267486));
#23412=CARTESIAN_POINT('Ctrl Pts',(1.6598316857201,-1.10635213456587,21.2060866459606));
#23413=CARTESIAN_POINT('Ctrl Pts',(1.65415421708014,-1.11482051901102,21.2054401389211));
#23414=CARTESIAN_POINT('Ctrl Pts',(1.65144582860549,-1.11882869019175,21.2051328399763));
#23415=CARTESIAN_POINT('Ctrl Pts',(1.64524054119214,-1.12794033431591,21.2044312743641));
#23416=CARTESIAN_POINT('Ctrl Pts',(1.64173443928362,-1.13303745110376,21.2040366601949));
#23417=CARTESIAN_POINT('Ctrl Pts',(1.63095449358012,-1.14855408109221,21.2028287236886));
#23418=CARTESIAN_POINT('Ctrl Pts',(1.62360486005962,-1.15892030929244,21.2020125119208));
#23419=CARTESIAN_POINT('Ctrl Pts',(1.60896633975525,-1.17915451440288,21.2004008141663));
#23420=CARTESIAN_POINT('Ctrl Pts',(1.60168445985505,-1.18902688412987,21.1996056227899));
#23421=CARTESIAN_POINT('Ctrl Pts',(1.49754528885855,-1.32752038600383,21.1883234883692));
#23422=CARTESIAN_POINT('Ctrl Pts',(1.38557209789052,-1.44399505643734,21.1772032650752));
#23423=CARTESIAN_POINT('Ctrl Pts',(1.19977609088203,-1.59554929898323,21.160474158432));
#23424=CARTESIAN_POINT('Ctrl Pts',(1.13579576672833,-1.64170932126844,21.1549763778008));
#23425=CARTESIAN_POINT('Ctrl Pts',(1.04283439308263,-1.70073602086015,21.147484875551));
#23426=CARTESIAN_POINT('Ctrl Pts',(1.01602744180602,-1.7168852761824,21.1453788666931));
#23427=CARTESIAN_POINT('Ctrl Pts',(0.973256065471496,-1.7412991120906,21.1421155135832));
#23428=CARTESIAN_POINT('Ctrl Pts',(0.957541837256029,-1.74998961487602,
21.1409365548075));
#23429=CARTESIAN_POINT('Ctrl Pts',(0.937347408219849,-1.76080433576715,
21.139448841269));
#23430=CARTESIAN_POINT('Ctrl Pts',(0.932974331977045,-1.76312534146083,
21.1391282981912));
#23431=CARTESIAN_POINT('Ctrl Pts',(0.925944222278671,-1.76682308512656,
21.1386156446599));
#23432=CARTESIAN_POINT('Ctrl Pts',(0.923292688525903,-1.768210148289,21.1384228898119));
#23433=CARTESIAN_POINT('Ctrl Pts',(0.918226948231438,-1.77084562307642,
21.1380557942818));
#23434=CARTESIAN_POINT('Ctrl Pts',(0.915813341110429,-1.77209505206391,
21.1378813924368));
#23435=CARTESIAN_POINT('Ctrl Pts',(0.910237887162976,-1.77496681099306,
21.1374796701835));
#23436=CARTESIAN_POINT('Ctrl Pts',(0.90707425423622,-1.77658562673838,21.1372525725932));
#23437=CARTESIAN_POINT('Ctrl Pts',(0.896918523092782,-1.78174806620431,
21.1365262171337));
#23438=CARTESIAN_POINT('Ctrl Pts',(0.889909748127897,-1.78525898780979,
21.1360289712314));
#23439=CARTESIAN_POINT('Ctrl Pts',(0.804656508339471,-1.82733826626339,
21.130027154693));
#23440=CARTESIAN_POINT('Ctrl Pts',(0.723972819034145,-1.86078069982627,
21.124819563072));
#23441=CARTESIAN_POINT('Ctrl Pts',(0.474973529853891,-1.94532763661055,
21.1093997423195));
#23442=CARTESIAN_POINT('Ctrl Pts',(0.30187637386104,-1.97958816458617,21.0994639507241));
#23443=CARTESIAN_POINT('Ctrl Pts',(0.0874915008619739,-1.99321419909783,
21.0863690198997));
#23444=CARTESIAN_POINT('Ctrl Pts',(0.0483922330984359,-1.99454643307504,
21.0839532755294));
#23445=CARTESIAN_POINT('Ctrl Pts',(-0.000171845794752117,-1.99477239096135,
21.0809087559399));
#23446=CARTESIAN_POINT('Ctrl Pts',(-0.00962477993409601,-1.9947491771997,
21.0803140891755));
#23447=CARTESIAN_POINT('Ctrl Pts',(-0.0245785091961187,-1.99460615863495,
21.079369990997));
#23448=CARTESIAN_POINT('Ctrl Pts',(-0.0300796686829023,-1.99453078284649,
21.0790219523416));
#23449=CARTESIAN_POINT('Ctrl Pts',(-0.0403944688794591,-1.99434676824405,
21.0783679838135));
#23450=CARTESIAN_POINT('Ctrl Pts',(-0.0452081745988543,-1.99424345690376,
21.0780622231253));
#23451=CARTESIAN_POINT('Ctrl Pts',(-0.0559766656579116,-1.99397333548177,
21.0773769320759));
#23452=CARTESIAN_POINT('Ctrl Pts',(-0.0619311534704512,-1.9937972767231,
21.0769971145785));
#23453=CARTESIAN_POINT('Ctrl Pts',(-0.0769963065174997,-1.99328428698191,
21.0760338822824));
#23454=CARTESIAN_POINT('Ctrl Pts',(-0.0861055402092911,-1.99291156635405,
21.0754493516363));
#23455=CARTESIAN_POINT('Ctrl Pts',(-0.111777499128371,-1.99168481518693,
21.073795923307));
#23456=CARTESIAN_POINT('Ctrl Pts',(-0.12833227512816,-1.990686668436,21.072722546437));
#23457=CARTESIAN_POINT('Ctrl Pts',(-0.304700458161688,-1.97784369888403,
21.0612084888847));
#23458=CARTESIAN_POINT('Ctrl Pts',(-0.462512780334678,-1.94698992303224,
21.0501439821441));
#23459=CARTESIAN_POINT('Ctrl Pts',(-0.690386557842399,-1.87314987845886,
21.0334308960687));
#23460=CARTESIAN_POINT('Ctrl Pts',(-0.764350001830473,-1.84420563727078,
21.027895021836));
#23461=CARTESIAN_POINT('Ctrl Pts',(-0.864914836788747,-1.79775880778824,
21.0203580303438));
#23462=CARTESIAN_POINT('Ctrl Pts',(-0.893120643696821,-1.78391427880746,
21.0182433884816));
#23463=CARTESIAN_POINT('Ctrl Pts',(-0.936962053657687,-1.76109452492476,
21.0149681586175));
#23464=CARTESIAN_POINT('Ctrl Pts',(-0.95282226985633,-1.75256429090815,
21.0137857746432));
#23465=CARTESIAN_POINT('Ctrl Pts',(-0.97289778490481,-1.74141379972355,
21.012294381605));
#23466=CARTESIAN_POINT('Ctrl Pts',(-0.977221180689317,-1.73899134185101,
21.0119735141634));
#23467=CARTESIAN_POINT('Ctrl Pts',(-0.984141587061875,-1.73507978495682,
21.0114604654936));
#23468=CARTESIAN_POINT('Ctrl Pts',(-0.986744316557314,-1.73360092800587,
21.0112676381339));
#23469=CARTESIAN_POINT('Ctrl Pts',(-0.991703454122104,-1.73076838615294,
21.0109004908793));
#23470=CARTESIAN_POINT('Ctrl Pts',(-0.994060396106565,-1.72941576157809,
21.0107261094687));
#23471=CARTESIAN_POINT('Ctrl Pts',(-0.999491271377177,-1.72628426801765,
21.0103245487756));
#23472=CARTESIAN_POINT('Ctrl Pts',(-1.0025632222725,-1.72450200388051,21.0100975917262));
#23473=CARTESIAN_POINT('Ctrl Pts',(-1.0123897695024,-1.71876577078851,21.0093721384879));
#23474=CARTESIAN_POINT('Ctrl Pts',(-1.019125965867,-1.71478018730684,21.0088756472427));
#23475=CARTESIAN_POINT('Ctrl Pts',(-1.11528037265996,-1.65712207192996,
21.0017977001473));
#23476=CARTESIAN_POINT('Ctrl Pts',(-1.20039270675749,-1.59654873091424,
20.9956420182105));
#23477=CARTESIAN_POINT('Ctrl Pts',(-1.29377619001345,-1.51837927406437,
20.9885452433897));
#23478=CARTESIAN_POINT('Ctrl Pts',(-1.30701776024503,-1.5069960291394,20.9875303175385));
#23479=CARTESIAN_POINT('Ctrl Pts',(-1.3899443047319,-1.43379216216006,20.9811081521863));
#23480=CARTESIAN_POINT('Ctrl Pts',(-1.45537482442311,-1.36732893258698,
20.9757342648897));
#23481=CARTESIAN_POINT('Ctrl Pts',(-1.55205386191034,-1.25429143651024,
20.9669245740612));
#23482=CARTESIAN_POINT('Ctrl Pts',(-1.5864038286869,-1.21055373530019,20.9635863570589));
#23483=CARTESIAN_POINT('Ctrl Pts',(-1.6378434426487,-1.13910045151353,20.9581907134116));
#23484=CARTESIAN_POINT('Ctrl Pts',(-1.65615962067804,-1.11230216370038,
20.9561794040305));
#23485=CARTESIAN_POINT('Ctrl Pts',(-1.67864536384126,-1.07761598895925,
20.9535859272684));
#23486=CARTESIAN_POINT('Ctrl Pts',(-1.68342768934117,-1.07012975281281,
20.9530267616563));
#23487=CARTESIAN_POINT('Ctrl Pts',(-1.69102317021305,-1.05806289645685,
20.9521262694408));
#23488=CARTESIAN_POINT('Ctrl Pts',(-1.69386812959824,-1.05350235579467,
20.9517861223918));
#23489=CARTESIAN_POINT('Ctrl Pts',(-1.69923646171272,-1.0448188244254,20.9511387854643));
#23490=CARTESIAN_POINT('Ctrl Pts',(-1.70176335234649,-1.04069804488252,
20.9508317280353));
#23491=CARTESIAN_POINT('Ctrl Pts',(-1.70747406450607,-1.03130876813957,
20.9501323809005));
#23492=CARTESIAN_POINT('Ctrl Pts',(-1.71064851455176,-1.02603465558443,
20.9497397518054));
#23493=CARTESIAN_POINT('Ctrl Pts',(-1.72022151452973,-1.00996190778892,
20.9485437920162));
#23494=CARTESIAN_POINT('Ctrl Pts',(-1.72654250038892,-0.99911765904418,
20.947737654936));
#23495=CARTESIAN_POINT('Ctrl Pts',(-1.81033636397372,-0.852191380164005,
20.9368241495545));
#23496=CARTESIAN_POINT('Ctrl Pts',(-1.87160893655554,-0.707536373281423,
20.9261124747945));
#23497=CARTESIAN_POINT('Ctrl Pts',(-1.95127313492434,-0.433717375003955,
20.9062345092853));
#23498=CARTESIAN_POINT('Ctrl Pts',(-1.97518037440777,-0.306994850058432,
20.8971983706322));
#23499=CARTESIAN_POINT('Ctrl Pts',(-1.9877100826093,-0.167806434641161,
20.8879527101568));
#23500=CARTESIAN_POINT('Ctrl Pts',(-1.98861169041916,-0.156760739973835,
20.8872237365665));
#23501=CARTESIAN_POINT('Ctrl Pts',(-1.99001844698862,-0.137553594038412,
20.8859650277712));
#23502=CARTESIAN_POINT('Ctrl Pts',(-1.9905655464046,-0.129395601328476,
20.8854331896449));
#23503=CARTESIAN_POINT('Ctrl Pts',(-1.99128459973133,-0.117586401925617,
20.8846675682353));
#23504=CARTESIAN_POINT('Ctrl Pts',(-1.99149669446991,-0.113937857985663,
20.8844316097618));
#23505=CARTESIAN_POINT('Ctrl Pts',(-1.99184935179946,-0.10756923578421,
20.8840207856241));
#23506=CARTESIAN_POINT('Ctrl Pts',(-1.99199437218206,-0.104849426857585,
20.8838456711378));
#23507=CARTESIAN_POINT('Ctrl Pts',(-1.99228609676488,-0.0991590471834062,
20.8834800033512));
#23508=CARTESIAN_POINT('Ctrl Pts',(-1.99243172798125,-0.0961884484689376,
20.8832895110457));
#23509=CARTESIAN_POINT('Ctrl Pts',(-1.99279825623071,-0.0883537246479702,
20.8827881321422));
#23510=CARTESIAN_POINT('Ctrl Pts',(-1.99300799016818,-0.0834890593249809,
20.8824778669979));
#23511=CARTESIAN_POINT('Ctrl Pts',(-1.99380596780158,-0.0632593994759704,
20.881191802085));
#23512=CARTESIAN_POINT('Ctrl Pts',(-1.99423437709987,-0.0478881272889963,
20.8802245984657));
#23513=CARTESIAN_POINT('Ctrl Pts',(-1.99465762594903,-0.0219241560307305,
20.8786054361783));
#23514=CARTESIAN_POINT('Ctrl Pts',(-1.99474591466741,-0.0113339883133201,
20.8779491026436));
#23515=CARTESIAN_POINT('Ctrl Pts',(-1.99476839307396,0.0489829932903482,
20.8742316625552));
#23516=CARTESIAN_POINT('Ctrl Pts',(-1.99292749800584,0.0986965464004528,
20.8712478548543));
#23517=CARTESIAN_POINT('Ctrl Pts',(-1.97716860906682,0.310089536787109,
20.8587101942019));
#23518=CARTESIAN_POINT('Ctrl Pts',(-1.94541358639662,0.469808908423853,
20.8495614641394));
#23519=CARTESIAN_POINT('Ctrl Pts',(-1.87426142568092,0.685876115117961,
20.8359556299183));
#23520=CARTESIAN_POINT('Ctrl Pts',(-1.85083560043257,0.746785209467117,
20.8319809491297));
#23521=CARTESIAN_POINT('Ctrl Pts',(-1.82023019411856,0.816026726300142,
20.8272483949835));
#23522=CARTESIAN_POINT('Ctrl Pts',(-1.81591426640882,0.825586426708788,
20.8265901799074));
#23523=CARTESIAN_POINT('Ctrl Pts',(-1.80888297791147,0.840838692181028,
20.825532067556));
#23524=CARTESIAN_POINT('Ctrl Pts',(-1.80621562482331,0.846553276059964,
20.8251338230302));
#23525=CARTESIAN_POINT('Ctrl Pts',(-1.80144122255652,0.856656748938176,
20.8244264813752));
#23526=CARTESIAN_POINT('Ctrl Pts',(-1.79934511091369,0.861050773746821,
20.82411776497));
#23527=CARTESIAN_POINT('Ctrl Pts',(-1.79495618607249,0.87016515167175,20.8234751114212));
#23528=CARTESIAN_POINT('Ctrl Pts',(-1.7926607915261,0.874884213345639,20.8231410862755));
#23529=CARTESIAN_POINT('Ctrl Pts',(-1.7866825027129,0.887052564697577,20.8222764291821));
#23530=CARTESIAN_POINT('Ctrl Pts',(-1.78297166095314,0.89448793776662,20.8217448238506));
#23531=CARTESIAN_POINT('Ctrl Pts',(-1.7670515179887,0.925894252489792,20.8194853286888));
#23532=CARTESIAN_POINT('Ctrl Pts',(-1.75440491070679,0.949639155452578,
20.8177421267536));
#23533=CARTESIAN_POINT('Ctrl Pts',(-1.72030565117904,1.01065571662531,20.8131686401678));
#23534=CARTESIAN_POINT('Ctrl Pts',(-1.69812200845352,1.04750069154125,20.810313186436));
#23535=CARTESIAN_POINT('Ctrl Pts',(-1.58360842852719,1.22448839014269,20.7961285278988));
#23536=CARTESIAN_POINT('Ctrl Pts',(-1.47503968637752,1.35330402724302,20.7842427318938));
#23537=CARTESIAN_POINT('Ctrl Pts',(-1.33863747803025,1.47898301608038,20.7714649813158));
#23538=CARTESIAN_POINT('Ctrl Pts',(-1.32545672513084,1.49080701554177,20.7702502186491));
#23539=CARTESIAN_POINT('Ctrl Pts',(-1.27455623573207,1.53525931890152,20.7656395087198));
#23540=CARTESIAN_POINT('Ctrl Pts',(-1.2357715660454,1.56664749845943,20.7622910888135));
#23541=CARTESIAN_POINT('Ctrl Pts',(-1.19012835875964,1.60083512877261,20.758570727107));
#23542=CARTESIAN_POINT('Ctrl Pts',(-1.18438623236307,1.60508812100165,20.758106534246));
#23543=CARTESIAN_POINT('Ctrl Pts',(-1.17583070523126,1.61135398944276,20.7574207439316));
#23544=CARTESIAN_POINT('Ctrl Pts',(-1.17303480173822,1.61339049241423,20.7571975491157));
#23545=CARTESIAN_POINT('Ctrl Pts',(-1.16804832328875,1.61700277005376,20.7568011344654));
#23546=CARTESIAN_POINT('Ctrl Pts',(-1.16585984014542,1.61858137804516,20.7566277193502));
#23547=CARTESIAN_POINT('Ctrl Pts',(-1.16116721392099,1.62195183186857,20.7562570880976));
#23548=CARTESIAN_POINT('Ctrl Pts',(-1.1586621317819,1.62374231584814,20.7560599659928));
#23549=CARTESIAN_POINT('Ctrl Pts',(-1.15180117775299,1.62862215593435,20.7555220570549));
#23550=CARTESIAN_POINT('Ctrl Pts',(-1.14743699056448,1.63169986031115,20.7551820637712));
#23551=CARTESIAN_POINT('Ctrl Pts',(-1.12464448547164,1.64763688477039,20.7534173536551));
#23552=CARTESIAN_POINT('Ctrl Pts',(-1.10601130715639,1.66020228136474,20.7520117899838));
#23553=CARTESIAN_POINT('Ctrl Pts',(-1.05106997858262,1.69591663626929,20.7479618943836));
#23554=CARTESIAN_POINT('Ctrl Pts',(-1.01421825613947,1.71820929582388,20.7453630016253));
#23555=CARTESIAN_POINT('Ctrl Pts',(-0.904317707491192,1.77992213952994,
20.7378636936592));
#23556=CARTESIAN_POINT('Ctrl Pts',(-0.829495670003397,1.81599879998697,
20.733068334897));
#23557=CARTESIAN_POINT('Ctrl Pts',(-0.611778883570966,1.9047020594815,20.7194317446622));
#23558=CARTESIAN_POINT('Ctrl Pts',(-0.464838532057203,1.9457850376763,20.7105528282108));
#23559=CARTESIAN_POINT('Ctrl Pts',(-0.302143524173006,1.9717752702888,20.7002656777771));
#23560=CARTESIAN_POINT('Ctrl Pts',(-0.289600578998553,1.97365648442812,
20.6994700978053));
#23561=CARTESIAN_POINT('Ctrl Pts',(-0.270918873800382,1.97627648397204,
20.6982811187106));
#23562=CARTESIAN_POINT('Ctrl Pts',(-0.264793072890843,1.97710657386833,
20.6978906062086));
#23563=CARTESIAN_POINT('Ctrl Pts',(-0.253867515447367,1.97853537815539,
20.6971929321118));
#23564=CARTESIAN_POINT('Ctrl Pts',(-0.249069232536893,1.97914513736109,
20.6968861218239));
#23565=CARTESIAN_POINT('Ctrl Pts',(-0.238948475413551,1.98039388140843,
20.6962381073448));
#23566=CARTESIAN_POINT('Ctrl Pts',(-0.233625555871817,1.98102887362625,
20.6958967797632));
#23567=CARTESIAN_POINT('Ctrl Pts',(-0.219539843419446,1.98265165417861,
20.6949921641047));
#23568=CARTESIAN_POINT('Ctrl Pts',(-0.210773025808216,1.9836027959536,20.6944277263706));
#23569=CARTESIAN_POINT('Ctrl Pts',(-0.170390079741878,1.98771334512583,
20.6918210112972));
#23570=CARTESIAN_POINT('Ctrl Pts',(-0.138709114305952,1.99017504498136,
20.6897569537459));
#23571=CARTESIAN_POINT('Ctrl Pts',(-0.0530896116608339,1.99477369023793,
20.6841237031214));
#23572=CARTESIAN_POINT('Ctrl Pts',(0.000895923536202471,1.9954796182546,
20.6805123946312));
#23573=CARTESIAN_POINT('Ctrl Pts',(0.157708187939494,1.99116689184892,20.6698571293759));
#23574=CARTESIAN_POINT('Ctrl Pts',(0.260195852412431,1.98038186095124,20.6626775326176));
#23575=CARTESIAN_POINT('Ctrl Pts',(0.474134462384115,1.94097089468312,20.6475040564342));
#23576=CARTESIAN_POINT('Ctrl Pts',(0.584898793153921,1.91051605508487,20.6395384356151));
#23577=CARTESIAN_POINT('Ctrl Pts',(0.699578850912882,1.86806714959347,20.6315527121247));
#23578=CARTESIAN_POINT('Ctrl Pts',(0.706698718336567,1.86538531409833,20.63105808478));
#23579=CARTESIAN_POINT('Ctrl Pts',(0.717131907084739,1.86138714344612,20.6303351702207));
#23580=CARTESIAN_POINT('Ctrl Pts',(0.720457215266392,1.8601025970093,20.6301050437164));
#23581=CARTESIAN_POINT('Ctrl Pts',(0.726313246717226,1.85782238810294,20.6297003030155));
#23582=CARTESIAN_POINT('Ctrl Pts',(0.728845399198117,1.85683045605249,20.6295254663805));
#23583=CARTESIAN_POINT('Ctrl Pts',(0.734154485792772,1.85473816893816,20.6291592641874));
#23584=CARTESIAN_POINT('Ctrl Pts',(0.73693097329095,1.8536367565459,20.6289679638558));
#23585=CARTESIAN_POINT('Ctrl Pts',(0.744280144748954,1.85070227154632,20.628462140696));
#23586=CARTESIAN_POINT('Ctrl Pts',(0.748848566360184,1.84885847421659,20.6281482593375));
#23587=CARTESIAN_POINT('Ctrl Pts',(0.769803995391451,1.84031053020935,20.6267108055312));
#23588=CARTESIAN_POINT('Ctrl Pts',(0.786108748360493,1.83340506353455,20.6255989157678));
#23589=CARTESIAN_POINT('Ctrl Pts',(0.830413390364009,1.81394121223263,20.6225898718312));
#23590=CARTESIAN_POINT('Ctrl Pts',(0.858219814201922,1.80095199397567,20.6207148897967));
#23591=CARTESIAN_POINT('Ctrl Pts',(0.954049267081981,1.75346329264872,20.6142633617162));
#23592=CARTESIAN_POINT('Ctrl Pts',(1.02038839779694,1.71570763020122,20.6098139422606));
#23593=CARTESIAN_POINT('Ctrl Pts',(1.22263834661753,1.58471046030953,20.595819758751));
#23594=CARTESIAN_POINT('Ctrl Pts',(1.34923259786795,1.4784167294981,20.5863451595544));
#23595=CARTESIAN_POINT('Ctrl Pts',(1.47549067428435,1.34253050423435,20.5748652196335));
#23596=CARTESIAN_POINT('Ctrl Pts',(1.48941989450352,1.3270603646162,20.5735673037745));
#23597=CARTESIAN_POINT('Ctrl Pts',(1.50822859696124,1.30550175172249,20.5717693601583));
#23598=CARTESIAN_POINT('Ctrl Pts',(1.51331859777057,1.29959806990368,20.571278093037));
#23599=CARTESIAN_POINT('Ctrl Pts',(1.52137097679652,1.29014699598195,20.5704932838955));
#23600=CARTESIAN_POINT('Ctrl Pts',(1.52435589162585,1.28661883841277,20.570200670987));
#23601=CARTESIAN_POINT('Ctrl Pts',(1.53045599836644,1.27935751080579,20.5695991651803));
#23602=CARTESIAN_POINT('Ctrl Pts',(1.53356985316342,1.27562326263333,20.569290220531));
#23603=CARTESIAN_POINT('Ctrl Pts',(1.54073341918444,1.26696831329434,20.5685750462435));
#23604=CARTESIAN_POINT('Ctrl Pts',(1.54477324709192,1.26203953559078,20.5681684197521));
#23605=CARTESIAN_POINT('Ctrl Pts',(1.55740397678857,1.24647794827303,20.5668865474606));
#23606=CARTESIAN_POINT('Ctrl Pts',(1.5659090940346,1.23577632126464,20.5660078722085));
#23607=CARTESIAN_POINT('Ctrl Pts',(1.65082204766596,1.12664977283399,20.557074940533));
#23608=CARTESIAN_POINT('Ctrl Pts',(1.71794396909565,1.02137709226249,20.5486515452287));
#23609=CARTESIAN_POINT('Ctrl Pts',(1.83576437377644,0.791727453541646,20.5307727742091));
#23610=CARTESIAN_POINT('Ctrl Pts',(1.88463965623471,0.667081514609771,20.5213313932871));
#23611=CARTESIAN_POINT('Ctrl Pts',(1.9311279464309,0.50126505474854,20.5096788883549));
#23612=CARTESIAN_POINT('Ctrl Pts',(1.94047977290186,0.463746200616541,20.5071016419899));
#23613=CARTESIAN_POINT('Ctrl Pts',(1.95014580237329,0.419526519009288,20.5041512691031));
#23614=CARTESIAN_POINT('Ctrl Pts',(1.95152367408803,0.41306961049691,20.5037226188492));
#23615=CARTESIAN_POINT('Ctrl Pts',(1.95356127096199,0.403283325922952,20.5030763332975));
#23616=CARTESIAN_POINT('Ctrl Pts',(1.95424458204713,0.39995899080945,20.5028573853821));
#23617=CARTESIAN_POINT('Ctrl Pts',(1.95545480467101,0.393994060232259,20.5024656012927));
#23618=CARTESIAN_POINT('Ctrl Pts',(1.95598485445028,0.391354138935763,20.5022925877211));
#23619=CARTESIAN_POINT('Ctrl Pts',(1.95711824032035,0.385649468091649,20.5019195410964));
#23620=CARTESIAN_POINT('Ctrl Pts',(1.95771972172431,0.382584383284932,20.5017196151784));
#23621=CARTESIAN_POINT('Ctrl Pts',(1.95936828162208,0.374077806464852,20.5011661392954));
#23622=CARTESIAN_POINT('Ctrl Pts',(1.96039989938741,0.368633292800868,20.5008134616092));
#23623=CARTESIAN_POINT('Ctrl Pts',(1.9660075460108,0.33834871726512,20.4988600707724));
#23624=CARTESIAN_POINT('Ctrl Pts',(1.97013439630459,0.313426436307198,20.4972837169013));
#23625=CARTESIAN_POINT('Ctrl Pts',(1.99733693981883,0.127274438934472,20.4856956322969));
#23626=CARTESIAN_POINT('Ctrl Pts',(2.00106448360066,-0.0361804509339467,
20.4765163451083));
#23627=CARTESIAN_POINT('Ctrl Pts',(1.98378470925755,-0.209153196562604,
20.4663531028269));
#23628=CARTESIAN_POINT('Ctrl Pts',(1.98260989290247,-0.220011003369011,
20.4657134456306));
#23629=CARTESIAN_POINT('Ctrl Pts',(1.96965121070298,-0.331229036817398,
20.4591406867822));
#23630=CARTESIAN_POINT('Ctrl Pts',(1.95034846566181,-0.430552195970423,
20.4530876079861));
#23631=CARTESIAN_POINT('Ctrl Pts',(1.92021939793493,-0.540322974101999,
20.4459812336882));
#23632=CARTESIAN_POINT('Ctrl Pts',(1.91671222826163,-0.55263520916391,20.4451782800329));
#23633=CARTESIAN_POINT('Ctrl Pts',(1.91132953098247,-0.570863811689611,
20.443980399156));
#23634=CARTESIAN_POINT('Ctrl Pts',(1.90954446543396,-0.576806727266043,
20.443588422871));
#23635=CARTESIAN_POINT('Ctrl Pts',(1.90631785433562,-0.587369750298536,
20.4428891094832));
#23636=CARTESIAN_POINT('Ctrl Pts',(1.90488716289222,-0.591993142947174,
20.4425821298778));
#23637=CARTESIAN_POINT('Ctrl Pts',(1.90184013570277,-0.601714435377332,
20.441934762351));
#23638=CARTESIAN_POINT('Ctrl Pts',(1.90022009778173,-0.606811125952121,
20.441594254879));
#23639=CARTESIAN_POINT('Ctrl Pts',(1.89589202236301,-0.620240084236888,
20.4406941217714));
#23640=CARTESIAN_POINT('Ctrl Pts',(1.89314957491207,-0.628561059485576,
20.4401333668126));
#23641=CARTESIAN_POINT('Ctrl Pts',(1.88039524767662,-0.666418732549545,
20.4375681658284));
#23642=CARTESIAN_POINT('Ctrl Pts',(1.86974680414694,-0.695734805670041,
20.435542777292));
#23643=CARTESIAN_POINT('Ctrl Pts',(1.83930489877027,-0.773790364627192,
20.4300410282625));
#23644=CARTESIAN_POINT('Ctrl Pts',(1.81826469385884,-0.822013826381631,
20.4265249259601));
#23645=CARTESIAN_POINT('Ctrl Pts',(1.7087984447378,-1.04807990322145,20.4094829484785));
#23646=CARTESIAN_POINT('Ctrl Pts',(1.596062681537,-1.21286214527536,20.3952207082234));
#23647=CARTESIAN_POINT('Ctrl Pts',(1.45746392762335,-1.36192928909657,20.3816285451081));
#23648=CARTESIAN_POINT('Ctrl Pts',(1.45405057768791,-1.36557292276706,20.381295918343));
#23649=CARTESIAN_POINT('Ctrl Pts',(1.4368148253314,-1.38383360048671,20.3796270793348));
#23650=CARTESIAN_POINT('Ctrl Pts',(1.42278490794068,-1.39825443273459,20.3783032452223));
#23651=CARTESIAN_POINT('Ctrl Pts',(1.40476520045535,-1.41622409659852,20.3766488773825));
#23652=CARTESIAN_POINT('Ctrl Pts',(1.40097671208021,-1.41997190605658,20.376303570256));
#23653=CARTESIAN_POINT('Ctrl Pts',(1.39495503138068,-1.42588137016206,20.3757587407628));
#23654=CARTESIAN_POINT('Ctrl Pts',(1.39273176216352,-1.42805303134533,20.3755584451444));
#23655=CARTESIAN_POINT('Ctrl Pts',(1.3885899436377,-1.43207983475016,20.37518691942));
#23656=CARTESIAN_POINT('Ctrl Pts',(1.38667276724863,-1.43393630310631,20.375015586868));
#23657=CARTESIAN_POINT('Ctrl Pts',(1.3823027627939,-1.43815096966422,20.3746264987679));
#23658=CARTESIAN_POINT('Ctrl Pts',(1.3798476291947,-1.44050673729787,20.3744089331239));
#23659=CARTESIAN_POINT('Ctrl Pts',(1.37242243489901,-1.44759501250875,20.3737539921292));
#23660=CARTESIAN_POINT('Ctrl Pts',(1.36743390309245,-1.45230822624932,20.3733180862744));
#23661=CARTESIAN_POINT('Ctrl Pts',(1.31845255320753,-1.4981101619401,20.3690767800569));
#23662=CARTESIAN_POINT('Ctrl Pts',(1.27264042127202,-1.53721799577438,20.3654133496719));
#23663=CARTESIAN_POINT('Ctrl Pts',(1.11777788709031,-1.65774028460213,20.3537152904472));
#23664=CARTESIAN_POINT('Ctrl Pts',(1.00216337446197,-1.73008756024586,20.34599524919));
#23665=CARTESIAN_POINT('Ctrl Pts',(0.788899591332623,-1.83493551619263,
20.3320483638324));
#23666=CARTESIAN_POINT('Ctrl Pts',(0.69444015082306,-1.87272515311601,20.3259635917708));
#23667=CARTESIAN_POINT('Ctrl Pts',(0.585316550302441,-1.9069860392324,20.3188231148549));
#23668=CARTESIAN_POINT('Ctrl Pts',(0.573074841999933,-1.91070050798264,
20.3180207303827));
#23669=CARTESIAN_POINT('Ctrl Pts',(0.554845239319503,-1.91604091958289,
20.3168235364142));
#23670=CARTESIAN_POINT('Ctrl Pts',(0.548883955707449,-1.91775713969889,
20.3164316728657));
#23671=CARTESIAN_POINT('Ctrl Pts',(0.538258022312406,-1.92076268305258,
20.3157324859282));
#23672=CARTESIAN_POINT('Ctrl Pts',(0.533596482817148,-1.92206289596355,
20.3154255195595));
#23673=CARTESIAN_POINT('Ctrl Pts',(0.528922010563834,-1.92334840039834,
20.3151174546899));
#23674=CARTESIAN_POINT('Ctrl Pts',(0.528913729745517,-1.92335067760937,
20.3151169089528));
#23675=CARTESIAN_POINT('Ctrl Pts',(0.52889718726741,-1.92335522664796,20.3151158187397));
#23676=CARTESIAN_POINT('Ctrl Pts',(0.52888892554063,-1.92335749849421,20.3151152742593));
#23677=CARTESIAN_POINT('Ctrl Pts',(0.528872420928399,-1.92336203689124,
20.3151141865386));
#23678=CARTESIAN_POINT('Ctrl Pts',(0.528864178114277,-1.92336430342267,
20.3151136433031));
#23679=CARTESIAN_POINT('Ctrl Pts',(0.528847711516913,-1.92336883113876,
20.3151125580847));
#23680=CARTESIAN_POINT('Ctrl Pts',(0.528839487629902,-1.9233710923522,20.315112016095));
#23681=CARTESIAN_POINT('Ctrl Pts',(0.523767067259621,-1.92476575370058,
20.3147777211988));
#23682=CARTESIAN_POINT('Ctrl Pts',(0.518697431709371,-1.92613813648773,
20.3144433197822));
#23683=CARTESIAN_POINT('Ctrl Pts',(0.505457657848107,-1.92966616711681,
20.3135692166355));
#23684=CARTESIAN_POINT('Ctrl Pts',(0.497279205034542,-1.93178993397027,
20.313028487511));
#23685=CARTESIAN_POINT('Ctrl Pts',(0.479334254635,-1.93632834181821,20.3118402354014));
#23686=CARTESIAN_POINT('Ctrl Pts',(0.469562531243437,-1.93872117594944,
20.3111920237576));
#23687=CARTESIAN_POINT('Ctrl Pts',(0.440789658567927,-1.945536593528,20.3092797784676));
#23688=CARTESIAN_POINT('Ctrl Pts',(0.421741682996167,-1.94975436091704,
20.3080092606781));
#23689=CARTESIAN_POINT('Ctrl Pts',(0.354850016223437,-1.96354003302606,
20.3035305146353));
#23690=CARTESIAN_POINT('Ctrl Pts',(0.306722968757956,-1.97163088840184,
20.3002773240443));
#23691=CARTESIAN_POINT('Ctrl Pts',(0.140755785821808,-1.99330878218816,
20.2889567147697));
#23692=CARTESIAN_POINT('Ctrl Pts',(0.0220349285774205,-1.99814947960201,
20.280666795027));
#23693=CARTESIAN_POINT('Ctrl Pts',(-0.168616295561586,-1.9889252680014,
20.2673631480476));
#23694=CARTESIAN_POINT('Ctrl Pts',(-0.240595802031494,-1.98150706759378,
20.2623478731941));
#23695=CARTESIAN_POINT('Ctrl Pts',(-0.347871859377439,-1.96451787710126,
20.2550130235649));
#23696=CARTESIAN_POINT('Ctrl Pts',(-0.383567143313866,-1.95786158239877,
20.2525964775362));
#23697=CARTESIAN_POINT('Ctrl Pts',(-0.424841584467101,-1.94899259072776,
20.2498453854307));
#23698=CARTESIAN_POINT('Ctrl Pts',(-0.43061423656448,-1.94772530712237,
20.2494616083487));
#23699=CARTESIAN_POINT('Ctrl Pts',(-0.439825434810796,-1.94566019848988,
20.2488509078089));
#23700=CARTESIAN_POINT('Ctrl Pts',(-0.443267588076611,-1.94487888232808,
20.2486230687879));
#23701=CARTESIAN_POINT('Ctrl Pts',(-0.449353041137022,-1.94348058244005,
20.2482209534395));
#23702=CARTESIAN_POINT('Ctrl Pts',(-0.451997175836633,-1.94286733548465,
20.2480464640574));
#23703=CARTESIAN_POINT('Ctrl Pts',(-0.457565648197978,-1.94156387170542,
20.2476794867065));
#23704=CARTESIAN_POINT('Ctrl Pts',(-0.46048967322923,-1.94087244595429,
20.2474870697029));
#23705=CARTESIAN_POINT('Ctrl Pts',(-0.468280741678794,-1.93901154326947,
20.2469751049772));
#23706=CARTESIAN_POINT('Ctrl Pts',(-0.473145004033291,-1.93783033943265,
20.2466562267975));
#23707=CARTESIAN_POINT('Ctrl Pts',(-0.495995807457831,-1.93219023791108,
20.2451615946121));
#23708=CARTESIAN_POINT('Ctrl Pts',(-0.513924815307466,-1.92749897545502,
20.2439986876174));
#23709=CARTESIAN_POINT('Ctrl Pts',(-0.69758776825939,-1.87669713630335,
20.2321624478231));
#23710=CARTESIAN_POINT('Ctrl Pts',(-0.856784875385627,-1.80957429655429,
20.2224976794698));
#23711=CARTESIAN_POINT('Ctrl Pts',(-1.10075895629859,-1.66719678253958,
20.2059745180876));
#23712=CARTESIAN_POINT('Ctrl Pts',(-1.19131131641182,-1.60374173462483,
20.1993914283463));
#23713=CARTESIAN_POINT('Ctrl Pts',(-1.28607029642266,-1.52486641012604,
20.1916954683965));
#23714=CARTESIAN_POINT('Ctrl Pts',(-1.29591634532761,-1.5165075632808,20.1908854579668));
#23715=CARTESIAN_POINT('Ctrl Pts',(-1.31038844883627,-1.50397754574264,
20.1896790639482));
#23716=CARTESIAN_POINT('Ctrl Pts',(-1.31507739280921,-1.49987925995224,
20.1892856934848));
#23717=CARTESIAN_POINT('Ctrl Pts',(-1.32337814949308,-1.49255528726999,
20.1885848136784));
#23718=CARTESIAN_POINT('Ctrl Pts',(-1.3269975680024,-1.48933826444883,20.1882776677347));
#23719=CARTESIAN_POINT('Ctrl Pts',(-1.33396468447799,-1.48310017088257,
20.1876834355184));
#23720=CARTESIAN_POINT('Ctrl Pts',(-1.33731392619724,-1.48008086216766,
20.1873964245369));
#23721=CARTESIAN_POINT('Ctrl Pts',(-1.34613466737381,-1.47207466731663,
20.1866369381957));
#23722=CARTESIAN_POINT('Ctrl Pts',(-1.35158865232037,-1.4670686696032,20.1861636538531));
#23723=CARTESIAN_POINT('Ctrl Pts',(-1.37260448857279,-1.44756240238564,
20.1843254945044));
#23724=CARTESIAN_POINT('Ctrl Pts',(-1.38796142418423,-1.43284438008474,
20.1829513084693));
#23725=CARTESIAN_POINT('Ctrl Pts',(-1.42564730543416,-1.39555198626953,
20.1794993852665));
#23726=CARTESIAN_POINT('Ctrl Pts',(-1.44767750056089,-1.37268541596079,
20.1774090697715));
#23727=CARTESIAN_POINT('Ctrl Pts',(-1.51759834108046,-1.29655407288879,
20.170531412078));
#23728=CARTESIAN_POINT('Ctrl Pts',(-1.56316425510684,-1.24123845635288,
20.1656569067693));
#23729=CARTESIAN_POINT('Ctrl Pts',(-1.66315172134245,-1.10559670011308,
20.1540240149303));
#23730=CARTESIAN_POINT('Ctrl Pts',(-1.71488863749726,-1.02351049239724,
20.147219639307));
#23731=CARTESIAN_POINT('Ctrl Pts',(-1.79990051468839,-0.863957834649184,
20.1346810595498));
#23732=CARTESIAN_POINT('Ctrl Pts',(-1.83464356822001,-0.787497024447547,
20.1289402964422));
#23733=CARTESIAN_POINT('Ctrl Pts',(-1.8672508331969,-0.701757111122103,
20.1229486288768));
#23734=CARTESIAN_POINT('Ctrl Pts',(-1.86998767853476,-0.694431281061299,
20.1224401652213));
#23735=CARTESIAN_POINT('Ctrl Pts',(-1.87390431070599,-0.683756390259391,
20.1217044969201));
#23736=CARTESIAN_POINT('Ctrl Pts',(-1.87511830784384,-0.680420090069961,
20.1214753148594));
#23737=CARTESIAN_POINT('Ctrl Pts',(-1.87724574121125,-0.674524553558618,
20.1210716603941));
#23738=CARTESIAN_POINT('Ctrl Pts',(-1.8781628629766,-0.671966670859111,
20.1208969694257));
#23739=CARTESIAN_POINT('Ctrl Pts',(-1.88007954767483,-0.666586394718117,
20.1205304580266));
#23740=CARTESIAN_POINT('Ctrl Pts',(-1.88107798144244,-0.663763629035798,
20.1203387051626));
#23741=CARTESIAN_POINT('Ctrl Pts',(-1.88371299589392,-0.656260236447226,
20.1198303932575));
#23742=CARTESIAN_POINT('Ctrl Pts',(-1.88533849955046,-0.651575699536349,
20.119514487004));
#23743=CARTESIAN_POINT('Ctrl Pts',(-1.89279531171783,-0.629824377485894,
20.118054141564));
#23744=CARTESIAN_POINT('Ctrl Pts',(-1.8984126836074,-0.612684401991071,
20.116921844109));
#23745=CARTESIAN_POINT('Ctrl Pts',(-1.9495871232946,-0.44907285613511,20.1062669395526));
#23746=CARTESIAN_POINT('Ctrl Pts',(-1.97834520572389,-0.297860487836512,
20.0975545876577));
#23747=CARTESIAN_POINT('Ctrl Pts',(-1.9929598869966,-0.0971002446200696,
20.0858436778963));
#23748=CARTESIAN_POINT('Ctrl Pts',(-1.99471555080441,-0.0492650808880827,
20.0830456991473));
#23749=CARTESIAN_POINT('Ctrl Pts',(-1.99474949799968,-0.00141517844896885,
20.0802123525403));
#23750=CARTESIAN_POINT('',(-1.9947498118588,0.000866365563832799,18.4790451186048));
#23751=CARTESIAN_POINT('Ctrl Pts',(-1.99474949974525,-0.00141271585688734,
20.0802122067223));
#23752=CARTESIAN_POINT('Ctrl Pts',(-1.99479157143496,0.0579923524695157,
20.0766946401339));
#23753=CARTESIAN_POINT('Ctrl Pts',(-1.99217996997649,0.117366413478714,
20.0731252228154));
#23754=CARTESIAN_POINT('Ctrl Pts',(-1.98462482765162,0.202401326950034,
20.0678812145986));
#23755=CARTESIAN_POINT('Ctrl Pts',(-1.98182164648267,0.228221095170741,
20.0662715292149));
#23756=CARTESIAN_POINT('Ctrl Pts',(-1.97754983490082,0.261498970957234,
20.064171466487));
#23757=CARTESIAN_POINT('Ctrl Pts',(-1.97654150200027,0.269014404190812,
20.0636955134407));
#23758=CARTESIAN_POINT('Ctrl Pts',(-1.97475763923998,0.281758346576112,
20.0628855115214));
#23759=CARTESIAN_POINT('Ctrl Pts',(-1.97400412832825,0.286989895422397,
20.0625521569281));
#23760=CARTESIAN_POINT('Ctrl Pts',(-1.97256852378058,0.296683940159797,
20.0619328696202));
#23761=CARTESIAN_POINT('Ctrl Pts',(-1.97189205527009,0.30114724500578,20.0616471162348));
#23762=CARTESIAN_POINT('Ctrl Pts',(-1.97046024938845,0.310382522488708,
20.0610545403539));
#23763=CARTESIAN_POINT('Ctrl Pts',(-1.96970271482704,0.315154119780667,
20.0607476500414));
#23764=CARTESIAN_POINT('Ctrl Pts',(-1.96794411801215,0.325977197581678,
20.0600498874106));
#23765=CARTESIAN_POINT('Ctrl Pts',(-1.96693246733654,0.332026885222133,
20.0596586815144));
#23766=CARTESIAN_POINT('Ctrl Pts',(-1.96425073004043,0.347621232672551,
20.0586471653638));
#23767=CARTESIAN_POINT('Ctrl Pts',(-1.96253898574749,0.357158474328952,
20.0580255367881));
#23768=CARTESIAN_POINT('Ctrl Pts',(-1.95157086246802,0.41580817921827,20.0541839222342));
#23769=CARTESIAN_POINT('Ctrl Pts',(-1.94054169223333,0.464566970840847,
20.0509078124423));
#23770=CARTESIAN_POINT('Ctrl Pts',(-1.92434694564427,0.525438773852179,
20.0467091832994));
#23771=CARTESIAN_POINT('Ctrl Pts',(-1.92087652530502,0.537987392652589,
20.0458377796828));
#23772=CARTESIAN_POINT('Ctrl Pts',(-1.90906629775885,0.579120031182964,
20.0429622371476));
#23773=CARTESIAN_POINT('Ctrl Pts',(-1.9002095833829,0.607550448750966,20.0409439823474));
#23774=CARTESIAN_POINT('Ctrl Pts',(-1.8550898910222,0.741731967202147,20.0312772633244));
#23775=CARTESIAN_POINT('Ctrl Pts',(-1.8106167829739,0.844504880364251,20.0234362259177));
#23776=CARTESIAN_POINT('Ctrl Pts',(-1.71323201346121,1.02603195526923,20.0091069977932));
#23777=CARTESIAN_POINT('Ctrl Pts',(-1.66285586473625,1.10581211996945,20.002621886709));
#23778=CARTESIAN_POINT('Ctrl Pts',(-1.60206958213234,1.18847401564678,19.995913648131));
#23779=CARTESIAN_POINT('Ctrl Pts',(-1.59707524053649,1.19517702198866,19.9953698050596));
#23780=CARTESIAN_POINT('Ctrl Pts',(-1.58981689601905,1.20479184897804,19.9945901300848));
#23781=CARTESIAN_POINT('Ctrl Pts',(-1.58758680638758,1.20772898240941,19.9943520118123));
#23782=CARTESIAN_POINT('Ctrl Pts',(-1.58369238853638,1.2128286883807,19.9939386934998));
#23783=CARTESIAN_POINT('Ctrl Pts',(-1.58203175133413,1.21499405225157,19.993763235557));
#23784=CARTESIAN_POINT('Ctrl Pts',(-1.57878391994185,1.2192110665583,19.9934216190243));
#23785=CARTESIAN_POINT('Ctrl Pts',(-1.57719717225079,1.22126302274253,19.9932554298611));
#23786=CARTESIAN_POINT('Ctrl Pts',(-1.57287736067164,1.22682687189651,19.9928048957413));
#23787=CARTESIAN_POINT('Ctrl Pts',(-1.57013651944046,1.23033275034268,19.9925210989883));
#23788=CARTESIAN_POINT('Ctrl Pts',(-1.55978582814503,1.24348165599816,19.9914569347669));
#23789=CARTESIAN_POINT('Ctrl Pts',(-1.55209849417305,1.25306374177308,19.9906818951945));
#23790=CARTESIAN_POINT('Ctrl Pts',(-1.54252308387722,1.26477594219974,19.9897342668684));
#23791=CARTESIAN_POINT('Ctrl Pts',(-1.54071854731388,1.26697356185253,19.9895564455782));
#23792=CARTESIAN_POINT('Ctrl Pts',(-1.44341994067265,1.38495148938827,19.9800090486742));
#23793=CARTESIAN_POINT('Ctrl Pts',(-1.3351531459121,1.48960804179835,19.9714545660136));
#23794=CARTESIAN_POINT('Ctrl Pts',(-1.14510025738833,1.63578985610729,19.9575242873846));
#23795=CARTESIAN_POINT('Ctrl Pts',(-1.07044784642207,1.68558670192604,19.9522779572911));
#23796=CARTESIAN_POINT('Ctrl Pts',(-0.963364394474653,1.74702629618186,
19.944820631185));
#23797=CARTESIAN_POINT('Ctrl Pts',(-0.933601571033613,1.76311081517892,
19.9427554660563));
#23798=CARTESIAN_POINT('Ctrl Pts',(-0.883517736577203,1.78855348389122,
19.9392826660378));
#23799=CARTESIAN_POINT('Ctrl Pts',(-0.863421987155416,1.79834078095296,
19.9378898853884));
#23800=CARTESIAN_POINT('Ctrl Pts',(-0.836164322159506,1.81105397147456,
19.9359998281854));
#23801=CARTESIAN_POINT('Ctrl Pts',(-0.829143171850048,1.814279156885,19.9355129020865));
#23802=CARTESIAN_POINT('Ctrl Pts',(-0.817995593756372,1.81932160409208,
19.9347396096534));
#23803=CARTESIAN_POINT('Ctrl Pts',(-0.813881387141164,1.82116582925369,
19.9344541713745));
#23804=CARTESIAN_POINT('Ctrl Pts',(-0.80533365341709,1.8249626675538,19.9338610380314));
#23805=CARTESIAN_POINT('Ctrl Pts',(-0.800899199043685,1.82691310783573,
19.9335532709729));
#23806=CARTESIAN_POINT('Ctrl Pts',(-0.790733790151156,1.83134011389263,
19.9328476027526));
#23807=CARTESIAN_POINT('Ctrl Pts',(-0.784998248123695,1.83380595718764,
19.9324493391482));
#23808=CARTESIAN_POINT('Ctrl Pts',(-0.76728841705765,1.84132151742653,19.9312192098373));
#23809=CARTESIAN_POINT('Ctrl Pts',(-0.755276473047177,1.84628109492061,
19.9303842975684));
#23810=CARTESIAN_POINT('Ctrl Pts',(-0.627497203455606,1.89758387336553,
19.9214953793794));
#23811=CARTESIAN_POINT('Ctrl Pts',(-0.50769808320323,1.93308287286196,19.9130708865235));
#23812=CARTESIAN_POINT('Ctrl Pts',(-0.230437029749444,1.98767902824605,
19.8935022627038));
#23813=CARTESIAN_POINT('Ctrl Pts',(-0.0724058547523233,1.99968255789331,
19.8822860173317));
#23814=CARTESIAN_POINT('Ctrl Pts',(0.103631904175656,1.99213989303651,19.8706063160622));
#23815=CARTESIAN_POINT('Ctrl Pts',(0.121862603145181,1.99110785474312,19.8694071947563));
#23816=CARTESIAN_POINT('Ctrl Pts',(0.145044833564224,1.98947590009342,19.867897837713));
#23817=CARTESIAN_POINT('Ctrl Pts',(0.150011067178842,1.98910759935675,19.8675753983959));
#23818=CARTESIAN_POINT('Ctrl Pts',(0.157965748569112,1.9884877113156,19.8670604349542));
#23819=CARTESIAN_POINT('Ctrl Pts',(0.160955058130292,1.98824797883173,19.866867256255));
#23820=CARTESIAN_POINT('Ctrl Pts',(0.166650600758536,1.98777828646641,19.8664998561568));
#23821=CARTESIAN_POINT('Ctrl Pts',(0.169356871456463,1.98754954379765,19.8663255715384));
#23822=CARTESIAN_POINT('Ctrl Pts',(0.17559035852282,1.98700984548761,19.8659247836223));
#23823=CARTESIAN_POINT('Ctrl Pts',(0.179117218275992,1.98669502507574,19.8656984997581));
#23824=CARTESIAN_POINT('Ctrl Pts',(0.188566409893344,1.98582618875558,19.8650934770131));
#23825=CARTESIAN_POINT('Ctrl Pts',(0.194487189884171,1.98525506623446,19.8647156799015));
#23826=CARTESIAN_POINT('Ctrl Pts',(0.237300289343633,1.98093191365155,19.8619927018668));
#23827=CARTESIAN_POINT('Ctrl Pts',(0.27408699710948,1.97617798229358,19.8597006549321));
#23828=CARTESIAN_POINT('Ctrl Pts',(0.32219531135202,1.96859153769233,19.8567408622568));
#23829=CARTESIAN_POINT('Ctrl Pts',(0.33365230809027,1.96668213197125,19.8560388145315));
#23830=CARTESIAN_POINT('Ctrl Pts',(0.377995416626657,1.95889332325865,19.8533303504125));
#23831=CARTESIAN_POINT('Ctrl Pts',(0.410749608172277,1.95228802240549,19.8513483611052));
#23832=CARTESIAN_POINT('Ctrl Pts',(0.576764093016468,1.91444569063303,19.8413301455033));
#23833=CARTESIAN_POINT('Ctrl Pts',(0.706718720786841,1.8703767146194,19.8335526180792));
#23834=CARTESIAN_POINT('Ctrl Pts',(0.880394668499987,1.79077314887592,19.8222249415291));
#23835=CARTESIAN_POINT('Ctrl Pts',(0.928705719902529,1.7662016396177,19.8189682357586));
#23836=CARTESIAN_POINT('Ctrl Pts',(0.994274895496613,1.72941790086039,19.8143585047188));
#23837=CARTESIAN_POINT('Ctrl Pts',(1.01243156762269,1.71885168471277,19.8130611367147));
#23838=CARTESIAN_POINT('Ctrl Pts',(1.03950541482379,1.70251834205102,19.8110929985837));
#23839=CARTESIAN_POINT('Ctrl Pts',(1.04854930467336,1.69696333528007,19.810429802151));
#23840=CARTESIAN_POINT('Ctrl Pts',(1.0650587620294,1.68664040516485,19.8092083021186));
#23841=CARTESIAN_POINT('Ctrl Pts',(1.07253776448059,1.68189439698195,19.8086508079343));
#23842=CARTESIAN_POINT('Ctrl Pts',(1.08446750711907,1.67421211796774,19.8077547809032));
#23843=CARTESIAN_POINT('Ctrl Pts',(1.08893857363858,1.67130750368955,19.8074174275886));
#23844=CARTESIAN_POINT('Ctrl Pts',(1.0934037171669,1.66838121358215,19.8070789639158));
#23845=CARTESIAN_POINT('Ctrl Pts',(1.09340952810014,1.66837740526779,19.8070785234369));
#23846=CARTESIAN_POINT('Ctrl Pts',(1.09342116748771,1.66836977706933,19.8070776411456));
#23847=CARTESIAN_POINT('Ctrl Pts',(1.0934269959196,1.66836595719968,19.8070771993349));
#23848=CARTESIAN_POINT('Ctrl Pts',(1.09343867034859,1.66835830586093,19.8070763143767));
#23849=CARTESIAN_POINT('Ctrl Pts',(1.09344451631787,1.66835447440981,19.8070758712313));
#23850=CARTESIAN_POINT('Ctrl Pts',(1.09345622602696,1.66834679977276,19.8070749835881));
#23851=CARTESIAN_POINT('Ctrl Pts',(1.09346208966169,1.66834295665544,19.8070745390982));
#23852=CARTESIAN_POINT('Ctrl Pts',(1.09347383460968,1.66833525874551,19.8070736487729));
#23853=CARTESIAN_POINT('Ctrl Pts',(1.09347971593568,1.66833140394427,19.8070732029365));
#23854=CARTESIAN_POINT('Ctrl Pts',(1.09349149631307,1.66832368263498,19.8070723099146));
#23855=CARTESIAN_POINT('Ctrl Pts',(1.0934973953828,1.66831981611463,19.8070718627277));
#23856=CARTESIAN_POINT('Ctrl Pts',(1.09350921136434,1.66831207128983,19.8070709669958));
#23857=CARTESIAN_POINT('Ctrl Pts',(1.09351512826697,1.66830819299112,19.8070705184516));
#23858=CARTESIAN_POINT('Ctrl Pts',(1.09352697988898,1.66830042462538,19.807069620007));
#23859=CARTESIAN_POINT('Ctrl Pts',(1.09353291464791,1.66829653453215,19.8070691701036));
#23860=CARTESIAN_POINT('Ctrl Pts',(1.09354480215066,1.66828874246634,19.8070682689279));
#23861=CARTESIAN_POINT('Ctrl Pts',(1.093550754861,1.66828484051543,19.807067817658));
#23862=CARTESIAN_POINT('Ctrl Pts',(1.09356267832501,1.66827702469512,19.807066913745));
#23863=CARTESIAN_POINT('Ctrl Pts',(1.09356864906477,1.66827311083456,19.8070664611028));
#23864=CARTESIAN_POINT('Ctrl Pts',(1.09358060852437,1.66826527123559,19.8070655544498));
#23865=CARTESIAN_POINT('Ctrl Pts',(1.0935865972904,1.66826134546661,19.8070651004354));
#23866=CARTESIAN_POINT('Ctrl Pts',(1.09359859308495,1.66825348186485,19.8070641910165));
#23867=CARTESIAN_POINT('Ctrl Pts',(1.09360460001615,1.66824954409558,19.8070637356194));
#23868=CARTESIAN_POINT('Ctrl Pts',(1.09361663211126,1.66824165651189,19.8070628234371));
#23869=CARTESIAN_POINT('Ctrl Pts',(1.093622657256,1.66823770670976,19.8070623666535));
#23870=CARTESIAN_POINT('Ctrl Pts',(1.09363472582534,1.66822979502859,19.8070614516947));
#23871=CARTESIAN_POINT('Ctrl Pts',(1.09364076925832,1.66822583314379,19.8070609935188));
#23872=CARTESIAN_POINT('Ctrl Pts',(1.09365287435609,1.66821789732792,19.8070600757792));
#23873=CARTESIAN_POINT('Ctrl Pts',(1.09365893608432,1.66821392335499,19.8070596162105));
#23874=CARTESIAN_POINT('Ctrl Pts',(1.09367107797674,1.66820596322817,19.8070586956698));
#23875=CARTESIAN_POINT('Ctrl Pts',(1.09367715808327,1.66820197711181,19.807058234702));
#23876=CARTESIAN_POINT('Ctrl Pts',(1.09368933694926,1.66819399255502,19.8070573113464));
#23877=CARTESIAN_POINT('Ctrl Pts',(1.0936954355811,1.66818999419798,19.8070568489683));
#23878=CARTESIAN_POINT('Ctrl Pts',(1.09370765132625,1.66818198527137,19.8070559228051));
#23879=CARTESIAN_POINT('Ctrl Pts',(1.09371376848406,1.66817797467233,19.8070554590165));
#23880=CARTESIAN_POINT('Ctrl Pts',(1.09372602140024,1.6681699411828,19.8070545300233));
#23881=CARTESIAN_POINT('Ctrl Pts',(1.09373215717773,1.66816591827947,19.8070540648171));
#23882=CARTESIAN_POINT('Ctrl Pts',(1.09374444728044,1.66815786021508,19.8070531329926));
#23883=CARTESIAN_POINT('Ctrl Pts',(1.09375060168012,1.66815382500492,19.8070526663687));
#23884=CARTESIAN_POINT('Ctrl Pts',(1.09376292930712,1.66814574214245,19.8070517316872));
#23885=CARTESIAN_POINT('Ctrl Pts',(1.09376910247076,1.66814169453161,19.8070512636346));
#23886=CARTESIAN_POINT('Ctrl Pts',(1.09378146754851,1.6681335869175,19.8070503261016));
#23887=CARTESIAN_POINT('Ctrl Pts',(1.09378765948411,1.66812952689984,19.8070498566197));
#23888=CARTESIAN_POINT('Ctrl Pts',(1.09380006232053,1.66812139433039,19.8070489162118));
#23889=CARTESIAN_POINT('Ctrl Pts',(1.09380627314936,1.6681173218255,19.8070484452913));
#23890=CARTESIAN_POINT('Ctrl Pts',(1.09381871373432,1.66810916430553,19.8070475020091));
#23891=CARTESIAN_POINT('Ctrl Pts',(1.09382494348527,1.66810507929355,19.8070470296478));
#23892=CARTESIAN_POINT('Ctrl Pts',(1.09383742204899,1.66809689667029,19.8070460834737));
#23893=CARTESIAN_POINT('Ctrl Pts',(1.09384367080592,1.66809279909532,19.8070456096652));
#23894=CARTESIAN_POINT('Ctrl Pts',(1.09385618753842,1.66808459124233,19.8070446605848));
#23895=CARTESIAN_POINT('Ctrl Pts',(1.09386245545394,1.66808048100337,19.8070441853174));
#23896=CARTESIAN_POINT('Ctrl Pts',(1.09387501015858,1.66807224804775,19.8070432333454));
#23897=CARTESIAN_POINT('Ctrl Pts',(1.09388129713543,1.66806812520767,19.8070427566265));
#23898=CARTESIAN_POINT('Ctrl Pts',(1.09389389036947,1.66805986678213,19.8070418017205));
#23899=CARTESIAN_POINT('Ctrl Pts',(1.09390019656389,1.66805573123752,19.8070413235382));
#23900=CARTESIAN_POINT('Ctrl Pts',(1.09391282823227,1.66804744740253,19.8070403657053));
#23901=CARTESIAN_POINT('Ctrl Pts',(1.09391915365422,1.66804329914594,19.8070398860588));
#23902=CARTESIAN_POINT('Ctrl Pts',(1.09796816187908,1.66538789788568,19.8067328542644));
#23903=CARTESIAN_POINT('Ctrl Pts',(1.10200116314678,1.66272197636024,19.8064257534902));
#23904=CARTESIAN_POINT('Ctrl Pts',(1.11115195608395,1.65662514042144,19.805726002304));
#23905=CARTESIAN_POINT('Ctrl Pts',(1.11626360378344,1.65318513507896,19.8053330110232));
#23906=CARTESIAN_POINT('Ctrl Pts',(1.13176342872066,1.64264949576233,19.8041348709326));
#23907=CARTESIAN_POINT('Ctrl Pts',(1.14210033438136,1.6354793299428,19.8033269007101));
#23908=CARTESIAN_POINT('Ctrl Pts',(1.27951916456512,1.5382210272217,19.7924638250715));
#23909=CARTESIAN_POINT('Ctrl Pts',(1.39566344971092,1.43366554211868,19.7818112632814));
#23910=CARTESIAN_POINT('Ctrl Pts',(1.55895069241756,1.24783916483241,19.7645695358436));
#23911=CARTESIAN_POINT('Ctrl Pts',(1.61464019877761,1.17489068577311,19.7581467393732));
#23912=CARTESIAN_POINT('Ctrl Pts',(1.68415777014259,1.06950267054128,19.7495304071077));
#23913=CARTESIAN_POINT('Ctrl Pts',(1.70244608518529,1.04014469324449,19.7471961918098));
#23914=CARTESIAN_POINT('Ctrl Pts',(1.72973041537877,0.993696206687807,19.7436210377723));
#23915=CARTESIAN_POINT('Ctrl Pts',(1.73925674948538,0.976926552352003,19.7423534636509));
#23916=CARTESIAN_POINT('Ctrl Pts',(1.75098119170168,0.955572175605586,19.7407709043396));
#23917=CARTESIAN_POINT('Ctrl Pts',(1.75340662556756,0.951114358672792,19.7404422548359));
#23918=CARTESIAN_POINT('Ctrl Pts',(1.75724830381259,0.943988920647067,19.7399197281302));
#23919=CARTESIAN_POINT('Ctrl Pts',(1.75867552758812,0.941327292984444,19.7397251625747));
#23920=CARTESIAN_POINT('Ctrl Pts',(1.76137208005775,0.936270956357053,19.739356730193));
#23921=CARTESIAN_POINT('Ctrl Pts',(1.76264255735098,0.933876931519931,19.7391827934883));
#23922=CARTESIAN_POINT('Ctrl Pts',(1.76554288860533,0.928384686433786,19.7387849018384));
#23923=CARTESIAN_POINT('Ctrl Pts',(1.76716946692051,0.925284763275979,19.7385611557832));
#23924=CARTESIAN_POINT('Ctrl Pts',(1.77228065763994,0.915481246707695,19.7378561287058));
#23925=CARTESIAN_POINT('Ctrl Pts',(1.77573540232728,0.908762030357327,19.7373766970123));
#23926=CARTESIAN_POINT('Ctrl Pts',(1.83477626388655,0.792309746267034,19.7291299761734));
#23927=CARTESIAN_POINT('Ctrl Pts',(1.8801426111822,0.677666914298953,19.7219575789469));
#23928=CARTESIAN_POINT('Ctrl Pts',(1.94273573170084,0.463489822721087,19.7090039508161));
#23929=CARTESIAN_POINT('Ctrl Pts',(1.96354075558599,0.365446936121691,19.7032307645136));
#23930=CARTESIAN_POINT('Ctrl Pts',(1.98363512103785,0.216253246808749,19.6942783748981));
#23931=CARTESIAN_POINT('Ctrl Pts',(1.98847018085168,0.166010602037781,19.6912372655598));
#23932=CARTESIAN_POINT('Ctrl Pts',(1.99314958321106,0.0854292211807199,
19.6862815434851));
#23933=CARTESIAN_POINT('Ctrl Pts',(1.9942161759429,0.0551824483347266,19.6844039778784));
#23934=CARTESIAN_POINT('Ctrl Pts',(1.99470260121952,0.0162557870631466,
19.6819607743806));
#23935=CARTESIAN_POINT('Ctrl Pts',(1.99475440981777,0.00758673939837224,
19.6814149634779));
#23936=CARTESIAN_POINT('Ctrl Pts',(1.99474681594471,-0.0064097607796518,
19.6805308746529));
#23937=CARTESIAN_POINT('Ctrl Pts',(1.99472258280768,-0.0117371842216121,
19.6801936998861));
#23938=CARTESIAN_POINT('Ctrl Pts',(1.99463556452769,-0.0219088464717725,
19.6795486294732));
#23939=CARTESIAN_POINT('Ctrl Pts',(1.99457647247869,-0.0267530855502447,
19.6792408518053));
#23940=CARTESIAN_POINT('Ctrl Pts',(1.99440082234015,-0.0378406527751516,
19.6785350931934));
#23941=CARTESIAN_POINT('Ctrl Pts',(1.99427259401908,-0.0440837207153039,
19.6781367494784));
#23942=CARTESIAN_POINT('Ctrl Pts',(1.99378702809095,-0.0633237524418409,
19.6769061304251));
#23943=CARTESIAN_POINT('Ctrl Pts',(1.9933319358954,-0.0763176980658115,
19.6760708050093));
#23944=CARTESIAN_POINT('Ctrl Pts',(1.98700944955615,-0.217395919012639,
19.6669541803501));
#23945=CARTESIAN_POINT('Ctrl Pts',(1.96893395600265,-0.344608745056516,
19.6582798602198));
#23946=CARTESIAN_POINT('Ctrl Pts',(1.9024249421722,-0.619439137984203,19.6386786546724));
#23947=CARTESIAN_POINT('Ctrl Pts',(1.84872032789869,-0.764959432134436,
19.6277122284852));
#23948=CARTESIAN_POINT('Ctrl Pts',(1.7705574685612,-0.918956594275065,19.6162668674067));
#23949=CARTESIAN_POINT('Ctrl Pts',(1.76214841711091,-0.934980205399458,
19.6150786590688));
#23950=CARTESIAN_POINT('Ctrl Pts',(1.75115574934955,-0.9552516666789,19.6135810118025));
#23951=CARTESIAN_POINT('Ctrl Pts',(1.74877305555854,-0.959606693709444,
19.6132595949053));
#23952=CARTESIAN_POINT('Ctrl Pts',(1.74492659525316,-0.966575249003801,
19.6127458769035));
#23953=CARTESIAN_POINT('Ctrl Pts',(1.74347317568109,-0.969194418463121,
19.612552926721));
#23954=CARTESIAN_POINT('Ctrl Pts',(1.74069018800519,-0.974183049423307,
19.6121856914928));
#23955=CARTESIAN_POINT('Ctrl Pts',(1.73936169498908,-0.976553039258202,
19.6120113443352));
#23956=CARTESIAN_POINT('Ctrl Pts',(1.73628729209446,-0.982011501101211,
19.611610055672));
#23957=CARTESIAN_POINT('Ctrl Pts',(1.7345379827498,-0.985098033627859,19.6113833354147));
#23958=CARTESIAN_POINT('Ctrl Pts',(1.7298220860889,-0.993367391619987,19.6107763824562));
#23959=CARTESIAN_POINT('Ctrl Pts',(1.72684041544024,-0.998541639609193,
19.6103971009775));
#23960=CARTESIAN_POINT('Ctrl Pts',(1.70493005716401,-1.03617216623934,19.6076417653366));
#23961=CARTESIAN_POINT('Ctrl Pts',(1.6851094953953,-1.06810378153494,19.6053202724379));
#23962=CARTESIAN_POINT('Ctrl Pts',(1.61760687655192,-1.1702914838794,19.597881117897));
#23963=CARTESIAN_POINT('Ctrl Pts',(1.56633846232174,-1.23807124751812,19.5929286551491));
#23964=CARTESIAN_POINT('Ctrl Pts',(1.44511601339076,-1.37870225203595,19.5821473603529));
#23965=CARTESIAN_POINT('Ctrl Pts',(1.37364234597441,-1.44992613011785,19.5763389418498));
#23966=CARTESIAN_POINT('Ctrl Pts',(1.25812265930164,-1.54880173355664,19.5673026416673));
#23967=CARTESIAN_POINT('Ctrl Pts',(1.21787804872935,-1.58064287192584,19.5642126794812));
#23968=CARTESIAN_POINT('Ctrl Pts',(1.1517180177734,-1.62896019463947,19.5591843445321));
#23969=CARTESIAN_POINT('Ctrl Pts',(1.12657123985685,-1.64645157545625,19.5572844344416));
#23970=CARTESIAN_POINT('Ctrl Pts',(1.09377309736181,-1.66816179332454,19.554816078568));
#23971=CARTESIAN_POINT('Ctrl Pts',(1.08648214965273,-1.67291957123913,19.5542679731884));
#23972=CARTESIAN_POINT('Ctrl Pts',(1.07467294820859,-1.68051601791366,19.5533810664996));
#23973=CARTESIAN_POINT('Ctrl Pts',(1.07017398654208,-1.68338458757999,19.5530433813259));
#23974=CARTESIAN_POINT('Ctrl Pts',(1.06156997405131,-1.68882213495668,19.5523979323579));
#23975=CARTESIAN_POINT('Ctrl Pts',(1.0574669654597,-1.69139428567346,19.5520902890578));
#23976=CARTESIAN_POINT('Ctrl Pts',(1.04806534420248,-1.69724052262482,19.5513856831637));
#23977=CARTESIAN_POINT('Ctrl Pts',(1.04276070179288,-1.70050477056073,19.550988361989));
#23978=CARTESIAN_POINT('Ctrl Pts',(1.02640513071954,-1.71046397663756,19.5497639856811));
#23979=CARTESIAN_POINT('Ctrl Pts',(1.01530454588711,-1.71707634477404,19.5489339251251));
#23980=CARTESIAN_POINT('Ctrl Pts',(0.908727680369466,-1.77916696609252,
19.540971996476));
#23981=CARTESIAN_POINT('Ctrl Pts',(0.808880720206796,-1.8267253765563,19.5335533776178));
#23982=CARTESIAN_POINT('Ctrl Pts',(0.544645531775835,-1.92665793510056,
19.5140864951871));
#23983=CARTESIAN_POINT('Ctrl Pts',(0.376465286938706,-1.96644969776647,
19.5018072687979));
#23984=CARTESIAN_POINT('Ctrl Pts',(0.186905103903939,-1.98606011123713,
19.4891718365038));
#23985=CARTESIAN_POINT('Ctrl Pts',(0.168518165702547,-1.98770469921553,
19.487959357438));
#23986=CARTESIAN_POINT('Ctrl Pts',(0.145125675942604,-1.98947005210635,
19.4864356824495));
#23987=CARTESIAN_POINT('Ctrl Pts',(0.140139633368759,-1.98982748863274,
19.4861120040694));
#23988=CARTESIAN_POINT('Ctrl Pts',(0.132156018878052,-1.99036965609028,
19.485595531373));
#23989=CARTESIAN_POINT('Ctrl Pts',(0.129159322958782,-1.99056636432869,
19.4854020757962));
#23990=CARTESIAN_POINT('Ctrl Pts',(0.123452854956208,-1.99092800597406,
19.4850344738957));
#23991=CARTESIAN_POINT('Ctrl Pts',(0.120743223897487,-1.99109417314495,
19.4848602630147));
#23992=CARTESIAN_POINT('Ctrl Pts',(0.114506810000172,-1.99146384154836,
19.4844600726191));
#23993=CARTESIAN_POINT('Ctrl Pts',(0.110979822084166,-1.99166350603977,
19.4842343103695));
#23994=CARTESIAN_POINT('Ctrl Pts',(0.101540914186302,-1.99217269615232,
19.4836315920804));
#23995=CARTESIAN_POINT('Ctrl Pts',(0.0956280593895489,-1.99246527822371,
19.4832555665839));
#23996=CARTESIAN_POINT('Ctrl Pts',(0.0532467157259226,-1.99437331027754,
19.4805708004221));
#23997=CARTESIAN_POINT('Ctrl Pts',(0.016738509186272,-1.99501387047296,
19.478313533195));
#23998=CARTESIAN_POINT('Ctrl Pts',(-0.025042684057217,-1.99459976855038,
19.475772774299));
#23999=CARTESIAN_POINT('Ctrl Pts',(-0.0303157837360414,-1.9945265921917,
19.4754528874787));
#24000=CARTESIAN_POINT('Ctrl Pts',(-0.0562843266006999,-1.99406321050778,
19.4738810893639));
#24001=CARTESIAN_POINT('Ctrl Pts',(-0.0769736919264156,-1.99337179522832,
19.4726399389276));
#24002=CARTESIAN_POINT('Ctrl Pts',(-0.117953404069742,-1.99136330454254,
19.4701972135433));
#24003=CARTESIAN_POINT('Ctrl Pts',(-0.138241716373127,-1.9900578080192,
19.4689954774902));
#24004=CARTESIAN_POINT('Ctrl Pts',(-0.290718815688208,-1.97790322979042,
19.4599988095077));
#24005=CARTESIAN_POINT('Ctrl Pts',(-0.421549135273346,-1.9542047333214,
19.4524539155032));
#24006=CARTESIAN_POINT('Ctrl Pts',(-0.603446190942141,-1.9021252370702,
19.4412558505582));
#24007=CARTESIAN_POINT('Ctrl Pts',(-0.65714014702683,-1.8842488615606,19.437861326509));
#24008=CARTESIAN_POINT('Ctrl Pts',(-0.740710073361018,-1.85241899800003,
19.4323827522007));
#24009=CARTESIAN_POINT('Ctrl Pts',(-0.771125909358189,-1.83996526954877,
19.4303466638326));
#24010=CARTESIAN_POINT('Ctrl Pts',(-0.80938916826633,-1.82318302168074,
19.4277254151994));
#24011=CARTESIAN_POINT('Ctrl Pts',(-0.817535152294955,-1.81954484057154,
19.4271638718119));
#24012=CARTESIAN_POINT('Ctrl Pts',(-0.830557190515278,-1.81362380324245,
19.426260458601));
#24013=CARTESIAN_POINT('Ctrl Pts',(-0.835448948732386,-1.81137560973404,
19.4259197821513));
#24014=CARTESIAN_POINT('Ctrl Pts',(-0.844713972374017,-1.80707200113342,
19.4252720266124));
#24015=CARTESIAN_POINT('Ctrl Pts',(-0.849088994313327,-1.80502044073333,
19.4249650825078));
#24016=CARTESIAN_POINT('Ctrl Pts',(-0.859006929183904,-1.80032562851777,
19.4242668050363));
#24017=CARTESIAN_POINT('Ctrl Pts',(-0.864545156779075,-1.7976726463903,
19.4238751362015));
#24018=CARTESIAN_POINT('Ctrl Pts',(-0.878811447988021,-1.79075747837467,
19.4228616443093));
#24019=CARTESIAN_POINT('Ctrl Pts',(-0.887520708249872,-1.78645707878797,
19.4222384943168));
#24020=CARTESIAN_POINT('Ctrl Pts',(-0.941188485771207,-1.7594680544678,
19.4183706474784));
#24021=CARTESIAN_POINT('Ctrl Pts',(-0.985302229741203,-1.73514908758266,
19.4150689417449));
#24022=CARTESIAN_POINT('Ctrl Pts',(-1.03949759437698,-1.70253889354015,
19.4108517883081));
#24023=CARTESIAN_POINT('Ctrl Pts',(-1.05048459455819,-1.69578183665368,
19.4099882975104));
#24024=CARTESIAN_POINT('Ctrl Pts',(-1.21378403095503,-1.59315591259754,
19.3970262251595));
#24025=CARTESIAN_POINT('Ctrl Pts',(-1.35249488239145,-1.47721307504617,
19.3842306262316));
#24026=CARTESIAN_POINT('Ctrl Pts',(-1.50040696629637,-1.3150556292171,19.3691873195122));
#24027=CARTESIAN_POINT('Ctrl Pts',(-1.52619187384494,-1.28504130596986,
19.3665062562997));
#24028=CARTESIAN_POINT('Ctrl Pts',(-1.5643955915988,-1.23779772350961,19.3624651413257));
#24029=CARTESIAN_POINT('Ctrl Pts',(-1.57745967271579,-1.22110517232585,
19.3610699616955));
#24030=CARTESIAN_POINT('Ctrl Pts',(-1.59341847787732,-1.20003023397758,
19.3593520096872));
#24031=CARTESIAN_POINT('Ctrl Pts',(-1.59656469005466,-1.19584121022814,
19.3590126415179));
#24032=CARTESIAN_POINT('Ctrl Pts',(-1.60152041240154,-1.1891884940077,19.358477069564));
#24033=CARTESIAN_POINT('Ctrl Pts',(-1.60334079786851,-1.18673299095385,
19.3582801175319));
#24034=CARTESIAN_POINT('Ctrl Pts',(-1.6067599080722,-1.1820987534504,19.3579097942538));
#24035=CARTESIAN_POINT('Ctrl Pts',(-1.60835983042557,-1.1799209808587,19.3577363418937));
#24036=CARTESIAN_POINT('Ctrl Pts',(-1.61201908326103,-1.17491882922439,
19.3573392419842));
#24037=CARTESIAN_POINT('Ctrl Pts',(-1.61407541557882,-1.17209228874836,
19.3571158036888));
#24038=CARTESIAN_POINT('Ctrl Pts',(-1.62042168983933,-1.16332061665698,
19.3564252859873));
#24039=CARTESIAN_POINT('Ctrl Pts',(-1.62468635515522,-1.15735714514718,
19.3559599214556));
#24040=CARTESIAN_POINT('Ctrl Pts',(-1.66100861095637,-1.10596969260325,
19.3519835329336));
#24041=CARTESIAN_POINT('Ctrl Pts',(-1.691190436754,-1.05924254363261,19.3485923049423));
#24042=CARTESIAN_POINT('Ctrl Pts',(-1.79926534056818,-0.875498635045534,
19.3358488056662));
#24043=CARTESIAN_POINT('Ctrl Pts',(-1.86277848868227,-0.730695713326674,
19.3269721050195));
#24044=CARTESIAN_POINT('Ctrl Pts',(-1.92526121514925,-0.525056752820484,
19.3142592322411));
#24045=CARTESIAN_POINT('Ctrl Pts',(-1.93955657242489,-0.46950488603592,
19.3108203998264));
#24046=CARTESIAN_POINT('Ctrl Pts',(-1.95831577760277,-0.380956545213267,
19.305276662275));
#24047=CARTESIAN_POINT('Ctrl Pts',(-1.96438137454597,-0.348330573188435,
19.3032211990962));
#24048=CARTESIAN_POINT('Ctrl Pts',(-1.97104627070201,-0.306731612706796,
19.3005782496893));
#24049=CARTESIAN_POINT('Ctrl Pts',(-1.97240280100466,-0.29788398726114,
19.3000148671833));
#24050=CARTESIAN_POINT('Ctrl Pts',(-1.97448073327285,-0.283694291599757,
19.2991091946587));
#24051=CARTESIAN_POINT('Ctrl Pts',(-1.97524011983714,-0.278357836619679,
19.2987681087472));
#24052=CARTESIAN_POINT('Ctrl Pts',(-1.97663906170083,-0.268232958463942,
19.2981200265467));
#24053=CARTESIAN_POINT('Ctrl Pts',(-1.97728287060039,-0.263445154071275,
19.297813167195));
#24054=CARTESIAN_POINT('Ctrl Pts',(-1.97870408228964,-0.252577292333428,
19.2971157030705));
#24055=CARTESIAN_POINT('Ctrl Pts',(-1.97947086238014,-0.246495917763622,
19.2967247658164));
#24056=CARTESIAN_POINT('Ctrl Pts',(-1.9813757684695,-0.230805659066627,
19.2957143956943));
#24057=CARTESIAN_POINT('Ctrl Pts',(-1.98247201927359,-0.221191942553078,
19.2950936494894));
#24058=CARTESIAN_POINT('Ctrl Pts',(-1.98877561114035,-0.162095104333968,
19.2912671989161));
#24059=CARTESIAN_POINT('Ctrl Pts',(-1.99219954051521,-0.112443369334408,
19.2880058791133));
#24060=CARTESIAN_POINT('Ctrl Pts',(-1.99417609289829,-0.049611094148558,
19.2838163002837));
#24061=CARTESIAN_POINT('Ctrl Pts',(-1.99445915274093,-0.0364996679966243,
19.2829386585307));
#24062=CARTESIAN_POINT('Ctrl Pts',(-1.99470984793476,-0.015118232770998,
19.2815019836021));
#24063=CARTESIAN_POINT('Ctrl Pts',(-1.99475537897725,-0.0068493957490642,
19.2809450477984));
#24064=CARTESIAN_POINT('Ctrl Pts',(-1.99461006220623,0.197369450072887,
19.267157738017));
#24065=CARTESIAN_POINT('Ctrl Pts',(-1.96560205707574,0.392193566079999,
19.2531195237202));
#24066=CARTESIAN_POINT('Ctrl Pts',(-1.89853482476783,0.613033893187592,
19.2375520550565));
#24067=CARTESIAN_POINT('Ctrl Pts',(-1.88752055048928,0.646151354663908,
19.2352314493102));
#24068=CARTESIAN_POINT('Ctrl Pts',(-1.87365455818853,0.68445617931814,19.2325771609461));
#24069=CARTESIAN_POINT('Ctrl Pts',(-1.87164272395583,0.689938534037558,
19.2321979911347));
#24070=CARTESIAN_POINT('Ctrl Pts',(-1.86838349219207,0.698700938786822,
19.2315932171183));
#24071=CARTESIAN_POINT('Ctrl Pts',(-1.8671514840325,0.701986618031553,19.2313667246304));
#24072=CARTESIAN_POINT('Ctrl Pts',(-1.86495215544196,0.707805320714476,
19.2309661455131));
#24073=CARTESIAN_POINT('Ctrl Pts',(-1.86398833392307,0.710339640925739,
19.2307918513531));
#24074=CARTESIAN_POINT('Ctrl Pts',(-1.86194163956103,0.715688470714734,
19.2304243744203));
#24075=CARTESIAN_POINT('Ctrl Pts',(-1.86085755392363,0.718502484718369,
19.2302312661074));
#24076=CARTESIAN_POINT('Ctrl Pts',(-1.85793931853889,0.726026583394934,
19.229715498019));
#24077=CARTESIAN_POINT('Ctrl Pts',(-1.85609362545229,0.730732212284432,
19.2293935254134));
#24078=CARTESIAN_POINT('Ctrl Pts',(-1.8472025353795,0.753149175914821,19.2278622921471));
#24079=CARTESIAN_POINT('Ctrl Pts',(-1.83992111112095,0.770766668630898,
19.226666654914));
#24080=CARTESIAN_POINT('Ctrl Pts',(-1.81894526820849,0.819525975530581,
19.2233719970962));
#24081=CARTESIAN_POINT('Ctrl Pts',(-1.80470463389051,0.850427056715048,
19.221300630423));
#24082=CARTESIAN_POINT('Ctrl Pts',(-1.74995615012824,0.961650383299276,
19.213853071179));
#24083=CARTESIAN_POINT('Ctrl Pts',(-1.70481689534721,1.03957662077931,19.2086471321123));
#24084=CARTESIAN_POINT('Ctrl Pts',(-1.57339007178949,1.23474434592281,19.1950011373688));
#24085=CARTESIAN_POINT('Ctrl Pts',(-1.47929198794705,1.3460453583392,19.186554212404));
#24086=CARTESIAN_POINT('Ctrl Pts',(-1.36524161323755,1.45440264437956,19.1768226476289));
#24087=CARTESIAN_POINT('Ctrl Pts',(-1.35646305430518,1.46259347978206,19.1760767531766));
#24088=CARTESIAN_POINT('Ctrl Pts',(-1.33790116351703,1.47960180040547,19.174505696094));
#24089=CARTESIAN_POINT('Ctrl Pts',(-1.32810340846043,1.48840261162717,19.1736798991539));
#24090=CARTESIAN_POINT('Ctrl Pts',(-1.31355887954949,1.50120924355131,19.1724587285113));
#24091=CARTESIAN_POINT('Ctrl Pts',(-1.3088792584224,1.50529107099677,19.1720665288867));
#24092=CARTESIAN_POINT('Ctrl Pts',(-1.30050788916851,1.51252449688049,19.1713661343983));
#24093=CARTESIAN_POINT('Ctrl Pts',(-1.296823537006,1.51568460988363,19.1710582950493));
#24094=CARTESIAN_POINT('Ctrl Pts',(-1.28909763732421,1.52226241448382,19.1704136127561));
#24095=CARTESIAN_POINT('Ctrl Pts',(-1.28505395263735,1.52567752655203,19.1700766673073));
#24096=CARTESIAN_POINT('Ctrl Pts',(-1.27447067911,1.5345437534886,19.1691960107829));
#24097=CARTESIAN_POINT('Ctrl Pts',(-1.26790975353078,1.53996912191667,19.1686512570793));
#24098=CARTESIAN_POINT('Ctrl Pts',(-1.23903347662685,1.56353789934106,19.1662586704155));
#24099=CARTESIAN_POINT('Ctrl Pts',(-1.21636290925108,1.58123870686895,19.1643931900431));
#24100=CARTESIAN_POINT('Ctrl Pts',(-1.15560330552658,1.62659883882741,19.1594240963888));
#24101=CARTESIAN_POINT('Ctrl Pts',(-1.11690611935303,1.6534094807499,19.1562895636654));
#24102=CARTESIAN_POINT('Ctrl Pts',(-0.910374383655349,1.78594059534205,
19.1397166619385));
#24103=CARTESIAN_POINT('Ctrl Pts',(-0.728439497648743,1.86754500433499,
19.1254933413746));
#24104=CARTESIAN_POINT('Ctrl Pts',(-0.506480137557737,1.92964803793909,
19.1099846034438));
#24105=CARTESIAN_POINT('Ctrl Pts',(-0.47527420373088,1.93757023199523,19.1078476939812));
#24106=CARTESIAN_POINT('Ctrl Pts',(-0.438333702445592,1.94600194919867,
19.1053796566277));
#24107=CARTESIAN_POINT('Ctrl Pts',(-0.432773830374164,1.94724596151668,
19.1050098254619));
#24108=CARTESIAN_POINT('Ctrl Pts',(-0.42382216271563,1.94920864873533,19.1044170828593));
#24109=CARTESIAN_POINT('Ctrl Pts',(-0.42043374060486,1.94994232020364,19.104193337312));
#24110=CARTESIAN_POINT('Ctrl Pts',(-0.414397369740995,1.95123286767823,
19.1037958690282));
#24111=CARTESIAN_POINT('Ctrl Pts',(-0.411750185403053,1.95179319322462,
19.1036219500371));
#24112=CARTESIAN_POINT('Ctrl Pts',(-0.40612716640827,1.95297146018727,19.1032533458392));
#24113=CARTESIAN_POINT('Ctrl Pts',(-0.403151066177744,1.95358798566721,
19.1030587425155));
#24114=CARTESIAN_POINT('Ctrl Pts',(-0.395117745364777,1.95523302006747,
19.1025347419746));
#24115=CARTESIAN_POINT('Ctrl Pts',(-0.390057880004449,1.95624871811876,
19.102206070726));
#24116=CARTESIAN_POINT('Ctrl Pts',(-0.365113371823572,1.96115535402875,
19.1005922780309));
#24117=CARTESIAN_POINT('Ctrl Pts',(-0.345173315211025,1.96476297719361,
19.0993226209827));
#24118=CARTESIAN_POINT('Ctrl Pts',(-0.288587915204649,1.97411250321723,
19.0957682478155));
#24119=CARTESIAN_POINT('Ctrl Pts',(-0.251831096599224,1.97913734026269,
19.093516757889));
#24120=CARTESIAN_POINT('Ctrl Pts',(-0.116506031913427,1.99380531516961,
19.0853679186858));
#24121=CARTESIAN_POINT('Ctrl Pts',(-0.0173946315439436,1.99713124639425,
19.0796659123627));
#24122=CARTESIAN_POINT('Ctrl Pts',(0.225767770818578,1.9871807813714,19.0655408954649));
#24123=CARTESIAN_POINT('Ctrl Pts',(0.368886777911649,1.96564813038824,19.0570812090882));
#24124=CARTESIAN_POINT('Ctrl Pts',(0.520827983858679,1.92559871343667,19.0472719488605));
#24125=CARTESIAN_POINT('Ctrl Pts',(0.533203014934197,1.92220881450737,19.0464671995945));
#24126=CARTESIAN_POINT('Ctrl Pts',(0.551518390679827,1.91700120053913,19.0452671519696));
#24127=CARTESIAN_POINT('Ctrl Pts',(0.557484504398185,1.91527469676413,19.0448748203123));
#24128=CARTESIAN_POINT('Ctrl Pts',(0.568085704878433,1.91215313821748,19.0441751081117));
#24129=CARTESIAN_POINT('Ctrl Pts',(0.572723980589902,1.91076901625044,19.0438680865696));
#24130=CARTESIAN_POINT('Ctrl Pts',(0.582473317147373,1.90782099944126,19.0432208720734));
#24131=CARTESIAN_POINT('Ctrl Pts',(0.587583214849239,1.90625341856959,19.0428805604902));
#24132=CARTESIAN_POINT('Ctrl Pts',(0.60103932313367,1.90206619658716,19.0419814980655));
#24133=CARTESIAN_POINT('Ctrl Pts',(0.609374636300733,1.89941218084499,19.0414216227364));
#24134=CARTESIAN_POINT('Ctrl Pts',(0.647214929698922,1.88708887816328,19.0388662349133));
#24135=CARTESIAN_POINT('Ctrl Pts',(0.676507759714877,1.87678679386743,19.0368499753536));
#24136=CARTESIAN_POINT('Ctrl Pts',(0.754442624496422,1.84731603909029,19.0313791154287));
#24137=CARTESIAN_POINT('Ctrl Pts',(0.80258868846046,1.82691292122322,19.027885319443));
#24138=CARTESIAN_POINT('Ctrl Pts',(0.941771155316311,1.76136667329637,19.0174498386052));
#24139=CARTESIAN_POINT('Ctrl Pts',(1.03022058744348,1.71113637966265,19.010371626379));
#24140=CARTESIAN_POINT('Ctrl Pts',(1.2128522065243,1.58810997310483,18.9950090905732));
#24141=CARTESIAN_POINT('Ctrl Pts',(1.30515473629979,1.51316950178545,18.9867505880825));
#24142=CARTESIAN_POINT('Ctrl Pts',(1.39573411221792,1.4251358515359,18.978502861267));
#24143=CARTESIAN_POINT('Ctrl Pts',(1.40118117169572,1.41978069996848,18.9780063288439));
#24144=CARTESIAN_POINT('Ctrl Pts',(1.4090907674789,1.41191470581817,18.9772846979359));
#24145=CARTESIAN_POINT('Ctrl Pts',(1.41157755612636,1.40942851220125,18.9770577251521));
#24146=CARTESIAN_POINT('Ctrl Pts',(1.41597089706986,1.40501293172964,18.9766565988912));
#24147=CARTESIAN_POINT('Ctrl Pts',(1.41788010241651,1.40308621802148,18.9764822359132));
#24148=CARTESIAN_POINT('Ctrl Pts',(1.42190083927048,1.39901202128495,18.9761149410083));
#24149=CARTESIAN_POINT('Ctrl Pts',(1.42401143370464,1.39686365454584,18.9759220822845));
#24150=CARTESIAN_POINT('Ctrl Pts',(1.4296389010258,1.3911094655672,18.9754076875339));
#24151=CARTESIAN_POINT('Ctrl Pts',(1.4331470247017,1.38749505924799,18.9750868322905));
#24152=CARTESIAN_POINT('Ctrl Pts',(1.44973118123455,1.37027846197375,18.9735689235499));
#24153=CARTESIAN_POINT('Ctrl Pts',(1.46262801538567,1.35650393020353,18.97238520801));
#24154=CARTESIAN_POINT('Ctrl Pts',(1.49789735416319,1.31774639711915,18.9691317346888));
#24155=CARTESIAN_POINT('Ctrl Pts',(1.51983908278505,1.29237822784512,18.9670887988578));
#24156=CARTESIAN_POINT('Ctrl Pts',(1.59710989032198,1.19834934614082,18.9597729581381));
#24157=CARTESIAN_POINT('Ctrl Pts',(1.64851391667944,1.1265900598515,18.9546647941645));
#24158=CARTESIAN_POINT('Ctrl Pts',(1.77294945459313,0.926032284283776,18.9409762194831));
#24159=CARTESIAN_POINT('Ctrl Pts',(1.83667716449269,0.792146101301501,18.9323948795123));
#24160=CARTESIAN_POINT('Ctrl Pts',(1.88919017415651,0.64042956496315,18.9224634004611));
#24161=CARTESIAN_POINT('Ctrl Pts',(1.89323776887667,0.628363175833703,18.9216725170902));
#24162=CARTESIAN_POINT('Ctrl Pts',(1.90109239201868,0.604182515390935,18.9200850961987));
#24163=CARTESIAN_POINT('Ctrl Pts',(1.90489976053855,0.592068986955557,18.9192886131363));
#24164=CARTESIAN_POINT('Ctrl Pts',(1.91038918202794,0.574002601069587,18.9180985434496));
#24165=CARTESIAN_POINT('Ctrl Pts',(1.9121596666601,0.568076773546139,18.9177078512868));
#24166=CARTESIAN_POINT('Ctrl Pts',(1.91526573475889,0.557501683026,18.9170099762887));
#24167=CARTESIAN_POINT('Ctrl Pts',(1.91661202436701,0.552855594793642,18.9167031455198));
#24168=CARTESIAN_POINT('Ctrl Pts',(1.91941420156649,0.543051936148847,18.9160552119053));
#24169=CARTESIAN_POINT('Ctrl Pts',(1.92086622844552,0.537893311004489,18.9157139861444));
#24170=CARTESIAN_POINT('Ctrl Pts',(1.92465060806694,0.524237767392702,18.9148099270281));
#24171=CARTESIAN_POINT('Ctrl Pts',(1.9269474594287,0.515731213290482,18.914245946548));
#24172=CARTESIAN_POINT('Ctrl Pts',(1.93724832997663,0.47655154249783,18.9116444239032));
#24173=CARTESIAN_POINT('Ctrl Pts',(1.94457643436697,0.44570703750624,18.909585207267));
#24174=CARTESIAN_POINT('Ctrl Pts',(1.96235091474038,0.362078484325791,18.9039684778908));
#24175=CARTESIAN_POINT('Ctrl Pts',(1.97140123123206,0.309027931035628,18.9003691522594));
#24176=CARTESIAN_POINT('Ctrl Pts',(1.99146903999612,0.15375560306599,18.8897362459326));
#24177=CARTESIAN_POINT('Ctrl Pts',(1.99674440567768,0.0509728397950796,
18.8825669248224));
#24178=CARTESIAN_POINT('Ctrl Pts',(1.99109407008832,-0.166755160266121,
18.8673747184937));
#24179=CARTESIAN_POINT('Ctrl Pts',(1.97816540034085,-0.281302786902861,
18.8593799506066));
#24180=CARTESIAN_POINT('Ctrl Pts',(1.95392706126697,-0.401565012017354,
18.8513683713491));
#24181=CARTESIAN_POINT('Ctrl Pts',(1.95238157855035,-0.409012953193088,
18.8508738493201));
#24182=CARTESIAN_POINT('Ctrl Pts',(1.95004933951711,-0.419937901509884,
18.8501510599525));
#24183=CARTESIAN_POINT('Ctrl Pts',(1.94929582944013,-0.423421819805583,
18.8499209542114));
#24184=CARTESIAN_POINT('Ctrl Pts',(1.94795098143183,-0.429560160825977,
18.8495162374245));
#24185=CARTESIAN_POINT('Ctrl Pts',(1.94736354889718,-0.432215416915608,
18.8493414040255));
#24186=CARTESIAN_POINT('Ctrl Pts',(1.94611946991086,-0.437784757717157,
18.8489751951939));
#24187=CARTESIAN_POINT('Ctrl Pts',(1.94546170880826,-0.440698564899252,
18.8487838850386));
#24188=CARTESIAN_POINT('Ctrl Pts',(1.94370166973369,-0.448414604701606,
18.848278007853));
#24189=CARTESIAN_POINT('Ctrl Pts',(1.94258813162305,-0.453214287904757,
18.8479640825371));
#24190=CARTESIAN_POINT('Ctrl Pts',(1.93738991134168,-0.475249010483119,
18.8465261357435));
#24191=CARTESIAN_POINT('Ctrl Pts',(1.93309341349026,-0.492433952564051,
18.8454138067364));
#24192=CARTESIAN_POINT('Ctrl Pts',(1.92072558088926,-0.539243370099406,
18.8424032870651));
#24193=CARTESIAN_POINT('Ctrl Pts',(1.91219805498775,-0.568743335661869,
18.8405272951433));
#24194=CARTESIAN_POINT('Ctrl Pts',(1.88010699102037,-0.670859298463815,
18.8340705385269));
#24195=CARTESIAN_POINT('Ctrl Pts',(1.85305859298422,-0.742313937661483,
18.8296171210869));
#24196=CARTESIAN_POINT('Ctrl Pts',(1.75497613771495,-0.962380372455703,
18.8156250605066));
#24197=CARTESIAN_POINT('Ctrl Pts',(1.66963537035923,-1.10382417610636,18.8061559707903));
#24198=CARTESIAN_POINT('Ctrl Pts',(1.5550256090783,-1.2495425009449,18.7946822542834));
#24199=CARTESIAN_POINT('Ctrl Pts',(1.54189833058624,-1.26570557138382,18.7933840105735));
#24200=CARTESIAN_POINT('Ctrl Pts',(1.5235118748498,-1.28763345119319,18.7915856821536));
#24201=CARTESIAN_POINT('Ctrl Pts',(1.51846800873429,-1.29357769040101,18.7910943629948));
#24202=CARTESIAN_POINT('Ctrl Pts',(1.51037870863932,-1.3029984951137,18.7903094914647));
#24203=CARTESIAN_POINT('Ctrl Pts',(1.5073557766421,-1.30649434894155,18.7900168684755));
#24204=CARTESIAN_POINT('Ctrl Pts',(1.50112772443305,-1.31364635942377,18.7894153573153));
#24205=CARTESIAN_POINT('Ctrl Pts',(1.49792133310086,-1.31730136333421,18.7891064174451));
#24206=CARTESIAN_POINT('Ctrl Pts',(1.49048178673474,-1.32571950764206,18.7883912799448));
#24207=CARTESIAN_POINT('Ctrl Pts',(1.48623912395737,-1.33047413894105,18.7879846855945));
#24208=CARTESIAN_POINT('Ctrl Pts',(1.47282560273044,-1.34536206819126,18.7867030146092));
#24209=CARTESIAN_POINT('Ctrl Pts',(1.46357349766461,-1.35542131902214,18.7858245100569));
#24210=CARTESIAN_POINT('Ctrl Pts',(1.36899728609609,-1.45615083413938,18.7768980821716));
#24211=CARTESIAN_POINT('Ctrl Pts',(1.27548158567696,-1.53872189519491,18.7684816303936));
#24212=CARTESIAN_POINT('Ctrl Pts',(1.07045483877802,-1.6881520385075,18.7509086163256));
#24213=CARTESIAN_POINT('Ctrl Pts',(0.958860150551927,-1.75394382086196,
18.741778678217));
#24214=CARTESIAN_POINT('Ctrl Pts',(0.802919105054839,-1.82652039212361,
18.7301026545817));
#24215=CARTESIAN_POINT('Ctrl Pts',(0.763580023330528,-1.84331278477983,
18.727244406527));
#24216=CARTESIAN_POINT('Ctrl Pts',(0.717405499615434,-1.8612906676147,18.7240134497637));
#24217=CARTESIAN_POINT('Ctrl Pts',(0.711070091785226,-1.8637201850121,18.7235728061334));
#24218=CARTESIAN_POINT('Ctrl Pts',(0.701510634610369,-1.86733022731593,
18.7229120555581));
#24219=CARTESIAN_POINT('Ctrl Pts',(0.698295813288188,-1.86853480189628,
18.7226905481327));
#24220=CARTESIAN_POINT('Ctrl Pts',(0.692620798080142,-1.87064450500476,
18.7223007845031));
#24221=CARTESIAN_POINT('Ctrl Pts',(0.690161921447034,-1.87155308674783,
18.7221323230139));
#24222=CARTESIAN_POINT('Ctrl Pts',(0.684878408046122,-1.87349357398586,
18.7217712372957));
#24223=CARTESIAN_POINT('Ctrl Pts',(0.682053236102053,-1.87452393662761,
18.7215787059357));
#24224=CARTESIAN_POINT('Ctrl Pts',(0.676223443005217,-1.87663518390325,
18.7211825186632));
#24225=CARTESIAN_POINT('Ctrl Pts',(0.67321853247528,-1.87771525163079,18.7209789113052));
#24226=CARTESIAN_POINT('Ctrl Pts',(0.665659937021267,-1.88041159291514,
18.7204682391235));
#24227=CARTESIAN_POINT('Ctrl Pts',(0.661102918091184,-1.88201855552993,
18.7201617103954));
#24228=CARTESIAN_POINT('Ctrl Pts',(0.648149342013863,-1.88653358048644,
18.7192940971228));
#24229=CARTESIAN_POINT('Ctrl Pts',(0.639739008739433,-1.88940216132828,
18.718735199416));
#24230=CARTESIAN_POINT('Ctrl Pts',(0.553880700907586,-1.91804752617227,
18.7130717745536));
#24231=CARTESIAN_POINT('Ctrl Pts',(0.474929194967297,-1.93910692519503,
18.7082111276932));
#24232=CARTESIAN_POINT('Ctrl Pts',(0.291248040574525,-1.97620449762924,
18.6972312546363));
#24233=CARTESIAN_POINT('Ctrl Pts',(0.186095166723978,-1.98886367971497,
18.6911757432887));
#24234=CARTESIAN_POINT('Ctrl Pts',(-0.0210114533441814,-1.99722154622232,
18.679010748956));
#24235=CARTESIAN_POINT('Ctrl Pts',(-0.122606996735743,-1.99356430198719,
18.6729303255419));
#24236=CARTESIAN_POINT('Ctrl Pts',(-0.23618474553309,-1.98075943428324,
18.665794719991));
#24237=CARTESIAN_POINT('Ctrl Pts',(-0.248880837784266,-1.97920425599955,
18.664992450444));
#24238=CARTESIAN_POINT('Ctrl Pts',(-0.26771037722805,-1.97671373610716,
18.6637953951755));
#24239=CARTESIAN_POINT('Ctrl Pts',(-0.273856005556042,-1.97587168798964,
18.6634035543951));
#24240=CARTESIAN_POINT('Ctrl Pts',(-0.284789085921504,-1.97432169600112,
18.6627043929912));
#24241=CARTESIAN_POINT('Ctrl Pts',(-0.289578098481244,-1.97362496613828,
18.6623974292919));
#24242=CARTESIAN_POINT('Ctrl Pts',(-0.299655081873104,-1.97212144855169,
18.6617500030035));
#24243=CARTESIAN_POINT('Ctrl Pts',(-0.304942430259469,-1.97131080482971,
18.6614094205114));
#24244=CARTESIAN_POINT('Ctrl Pts',(-0.318886241762849,-1.96911553210243,
18.6605088773625));
#24245=CARTESIAN_POINT('Ctrl Pts',(-0.327536872891857,-1.96769510005466,
18.6599477855285));
#24246=CARTESIAN_POINT('Ctrl Pts',(-0.366971436970498,-1.96095270177919,
18.6573788159813));
#24247=CARTESIAN_POINT('Ctrl Pts',(-0.397635637482324,-1.95496528099559,
18.6553499204388));
#24248=CARTESIAN_POINT('Ctrl Pts',(-0.479637898766279,-1.93694465454788,
18.6498362892341));
#24249=CARTESIAN_POINT('Ctrl Pts',(-0.530657549781949,-1.92359269514701,
18.6463116005113));
#24250=CARTESIAN_POINT('Ctrl Pts',(-0.67620728268537,-1.87927075147409,
18.6359874324675));
#24251=CARTESIAN_POINT('Ctrl Pts',(-0.769023283211464,-1.84323491135177,
18.6290610423482));
#24252=CARTESIAN_POINT('Ctrl Pts',(-0.894923591927749,-1.78318391182548,
18.6193291659809));
#24253=CARTESIAN_POINT('Ctrl Pts',(-0.930562084471992,-1.76484770213853,
18.6165354953556));
#24254=CARTESIAN_POINT('Ctrl Pts',(-1.03542380158946,-1.70683570473254,
18.6082354042682));
#24255=CARTESIAN_POINT('Ctrl Pts',(-1.10285314113458,-1.6640639145745,18.602788488158));
#24256=CARTESIAN_POINT('Ctrl Pts',(-1.17385887229917,-1.61280610191208,
18.5970687043649));
#24257=CARTESIAN_POINT('Ctrl Pts',(-1.18014471967242,-1.60821224342719,
18.5965625235583));
#24258=CARTESIAN_POINT('Ctrl Pts',(-1.18925251748062,-1.60147387454476,
18.5958295384597));
#24259=CARTESIAN_POINT('Ctrl Pts',(-1.19209580591436,-1.59935853115591,
18.5956007766812));
#24260=CARTESIAN_POINT('Ctrl Pts',(-1.19706405034536,-1.59564165836322,
18.5952011801115));
#24261=CARTESIAN_POINT('Ctrl Pts',(-1.19919145713552,-1.59404344106643,
18.5950301157123));
#24262=CARTESIAN_POINT('Ctrl Pts',(-1.20364684836035,-1.59068235479456,
18.594671956812));
#24263=CARTESIAN_POINT('Ctrl Pts',(-1.2059741566668,-1.5889186332671,18.5944849241815));
#24264=CARTESIAN_POINT('Ctrl Pts',(-1.21200616676444,-1.58432646221614,
18.5940002828221));
#24265=CARTESIAN_POINT('Ctrl Pts',(-1.21570486977454,-1.58149010677236,
18.5937032260741));
#24266=CARTESIAN_POINT('Ctrl Pts',(-1.22383104042245,-1.57521318743955,
18.5930507531277));
#24267=CARTESIAN_POINT('Ctrl Pts',(-1.22825402925024,-1.57176685382326,
18.5926957312136));
#24268=CARTESIAN_POINT('Ctrl Pts',(-1.24126494099582,-1.56154046616931,
18.5916515147872));
#24269=CARTESIAN_POINT('Ctrl Pts',(-1.24981183389738,-1.55470822767957,
18.5909657428702));
#24270=CARTESIAN_POINT('Ctrl Pts',(-1.2798047220425,-1.53032524696298,18.5885581026482));
#24271=CARTESIAN_POINT('Ctrl Pts',(-1.30094170527475,-1.51239754366509,
18.5868593029022));
#24272=CARTESIAN_POINT('Ctrl Pts',(-1.40677906570725,-1.41876838842703,
18.5783018875312));
#24273=CARTESIAN_POINT('Ctrl Pts',(-1.48528173685675,-1.33636589834739,
18.5717737066171));
#24274=CARTESIAN_POINT('Ctrl Pts',(-1.64618998778756,-1.13565679721318,
18.5568419694347));
#24275=CARTESIAN_POINT('Ctrl Pts',(-1.7236523006194,-1.01423474826733,18.5484201721396));
#24276=CARTESIAN_POINT('Ctrl Pts',(-1.79311044995909,-0.874041015284506,
18.5386532471053));
#24277=CARTESIAN_POINT('Ctrl Pts',(-1.79870524800957,-0.862468666454245,
18.5378470762196));
#24278=CARTESIAN_POINT('Ctrl Pts',(-1.80683884768547,-0.845221611485181,
18.5366453134103));
#24279=CARTESIAN_POINT('Ctrl Pts',(-1.80946366991463,-0.839587648709466,
18.5362527006984));
#24280=CARTESIAN_POINT('Ctrl Pts',(-1.81408594877558,-0.829543951768758,
18.5355526728614));
#24281=CARTESIAN_POINT('Ctrl Pts',(-1.8160937731473,-0.825139020965405,
18.5352456179272));
#24282=CARTESIAN_POINT('Ctrl Pts',(-1.82028369669915,-0.815857444135958,
18.5345985233619));
#24283=CARTESIAN_POINT('Ctrl Pts',(-1.82246227531362,-0.810979259761785,
18.5342583658277));
#24284=CARTESIAN_POINT('Ctrl Pts',(-1.8281518787571,-0.79810062343403,18.5333601454061));
#24285=CARTESIAN_POINT('Ctrl Pts',(-1.83162995298638,-0.790085823327649,
18.5328009618283));
#24286=CARTESIAN_POINT('Ctrl Pts',(-1.84718554666243,-0.753585053916015,
18.5302532637896));
#24287=CARTESIAN_POINT('Ctrl Pts',(-1.85865138710598,-0.724844617589241,
18.5282441547314));
#24288=CARTESIAN_POINT('Ctrl Pts',(-1.88759139078703,-0.647095572828773,
18.52279744819));
#24289=CARTESIAN_POINT('Ctrl Pts',(-1.90382342613669,-0.597653339737001,
18.519321079174));
#24290=CARTESIAN_POINT('Ctrl Pts',(-1.96903110870473,-0.369262700635089,
18.5032132497618));
#24291=CARTESIAN_POINT('Ctrl Pts',(-1.9948202059118,-0.184693437491307,
18.4899526768026));
#24292=CARTESIAN_POINT('Ctrl Pts',(-1.99474985647572,0.000756696823254535,
18.4774220616698));
#24293=CARTESIAN_POINT('',(-1.99474917376081,-0.00181556617865773,17.6790451186048));
#24294=CARTESIAN_POINT('Ctrl Pts',(-1.99474917376081,-0.00181556617865773,
17.6790451186048));
#24295=CARTESIAN_POINT('Ctrl Pts',(-1.9946619313494,-0.0976681603296343,
17.6851684928657));
#24296=CARTESIAN_POINT('Ctrl Pts',(-1.98766217964683,-0.193217564775626,
17.6912918671266));
#24297=CARTESIAN_POINT('Ctrl Pts',(-1.97390131051665,-0.287647664410234,
17.6974152413876));
#24298=CARTESIAN_POINT('Ctrl Pts',(-1.96688300708852,-0.335808800579352,
17.700538278033));
#24299=CARTESIAN_POINT('Ctrl Pts',(-1.95810674035759,-0.383679286233765,
17.7036613146785));
#24300=CARTESIAN_POINT('Ctrl Pts',(-1.94759707343738,-0.431153339356385,
17.706784351324));
#24301=CARTESIAN_POINT('Ctrl Pts',(-1.93260830811386,-0.498860284458797,
17.711238390042));
#24302=CARTESIAN_POINT('Ctrl Pts',(-1.9140549686818,-0.565918774422324,
17.71569242876));
#24303=CARTESIAN_POINT('Ctrl Pts',(-1.89200890460737,-0.631925523607358,
17.7201464674779));
#24304=CARTESIAN_POINT('Ctrl Pts',(-1.86999597919259,-0.697833054392723,
17.7245938110837));
#24305=CARTESIAN_POINT('Ctrl Pts',(-1.84450090312234,-0.762691521591686,
17.7290411546895));
#24306=CARTESIAN_POINT('Ctrl Pts',(-1.81564626477699,-0.826109074941892,
17.7334884982952));
#24307=CARTESIAN_POINT('Ctrl Pts',(-1.78682564308431,-0.889451865515344,
17.73793059894));
#24308=CARTESIAN_POINT('Ctrl Pts',(-1.75465352709317,-0.951356672597149,
17.7423726995848));
#24309=CARTESIAN_POINT('Ctrl Pts',(-1.71930130765783,-1.01144973972317,
17.7468148002296));
#24310=CARTESIAN_POINT('Ctrl Pts',(-1.68397138855911,-1.07150489987627,
17.7512540987776));
#24311=CARTESIAN_POINT('Ctrl Pts',(-1.64546559316361,-1.12975016625242,
17.7556933973256));
#24312=CARTESIAN_POINT('Ctrl Pts',(-1.60400143668215,-1.18583597247748,
17.7601326958736));
#24313=CARTESIAN_POINT('Ctrl Pts',(-1.56254934635505,-1.24190545761819,
17.7645707025767));
#24314=CARTESIAN_POINT('Ctrl Pts',(-1.51814089482739,-1.29581633663531,
17.7690087092798));
#24315=CARTESIAN_POINT('Ctrl Pts',(-1.47103613297335,-1.34724914473411,
17.7734467159828));
#24316=CARTESIAN_POINT('Ctrl Pts',(-1.42392907285789,-1.39868446226157,
17.7778849392181));
#24317=CARTESIAN_POINT('Ctrl Pts',(-1.37412577364437,-1.44764110941488,
17.7823231624534));
#24318=CARTESIAN_POINT('Ctrl Pts',(-1.32192446154567,-1.49383509145661,
17.7867613856887));
#24319=CARTESIAN_POINT('Ctrl Pts',(-1.26966784791765,-1.54007801092443,
17.7912043107318));
#24320=CARTESIAN_POINT('Ctrl Pts',(-1.2150085181826,-1.58355209857006,17.7956472357748));
#24321=CARTESIAN_POINT('Ctrl Pts',(-1.15827850124395,-1.62401307755081,
17.8000901608178));
#24322=CARTESIAN_POINT('Ctrl Pts',(-1.10151536865938,-1.66449767527039,
17.8045356793791));
#24323=CARTESIAN_POINT('Ctrl Pts',(-1.04267955606598,-1.70196540043725,
17.8089811979403));
#24324=CARTESIAN_POINT('Ctrl Pts',(-0.982130486825968,-1.73621636593686,
17.8134267165016));
#24325=CARTESIAN_POINT('Ctrl Pts',(-0.921475757769878,-1.77052710032739,
17.8178799926168));
#24326=CARTESIAN_POINT('Ctrl Pts',(-0.859102242251811,-1.80160965149693,
17.822333268732));
#24327=CARTESIAN_POINT('Ctrl Pts',(-0.795391532281774,-1.82931131108799,
17.8267865448473));
#24328=CARTESIAN_POINT('Ctrl Pts',(-0.7612762792085,-1.84414475318812,17.829171146145));
#24329=CARTESIAN_POINT('Ctrl Pts',(-0.72677791776351,-1.85800963399779,
17.8315557474428));
#24330=CARTESIAN_POINT('Ctrl Pts',(-0.69195671403833,-1.87088841687506,
17.8339403487406));
#24331=CARTESIAN_POINT('Ctrl Pts',(-0.626916495472786,-1.89494384183414,
17.8383943874586));
#24332=CARTESIAN_POINT('Ctrl Pts',(-0.560491567793676,-1.91565124300101,
17.8428484261766));
#24333=CARTESIAN_POINT('Ctrl Pts',(-0.49305989658857,-1.9328526847321,17.8473024648945));
#24334=CARTESIAN_POINT('Ctrl Pts',(-0.425729585662315,-1.95002827002362,
17.8517498085003));
#24335=CARTESIAN_POINT('Ctrl Pts',(-0.357396005222441,-1.9637082355019,
17.8561971521061));
#24336=CARTESIAN_POINT('Ctrl Pts',(-0.288454977126301,-1.97378349589591,
17.8606444957118));
#24337=CARTESIAN_POINT('Ctrl Pts',(-0.219595223415858,-1.98384687859354,
17.8650865963566));
#24338=CARTESIAN_POINT('Ctrl Pts',(-0.150129926427493,-1.99031392594899,
17.8695286970014));
#24339=CARTESIAN_POINT('Ctrl Pts',(-0.0804661177590715,-1.993126379935,
17.8739707976462));
#24340=CARTESIAN_POINT('Ctrl Pts',(-0.0108462533297702,-1.99593705981257,
17.8784100961942));
#24341=CARTESIAN_POINT('Ctrl Pts',(0.0589713863406405,-1.99509769986978,
17.8828493947422));
#24342=CARTESIAN_POINT('Ctrl Pts',(0.128575135381385,-1.99060191828041,
17.8872886932902));
#24343=CARTESIAN_POINT('Ctrl Pts',(0.198158629588811,-1.98610744497268,
17.8917266999933));
#24344=CARTESIAN_POINT('Ctrl Pts',(0.26752786843497,-1.97795869381767,17.8961647066964));
#24345=CARTESIAN_POINT('Ctrl Pts',(0.336273464866386,-1.96620134251982,
17.9006027133994));
#24346=CARTESIAN_POINT('Ctrl Pts',(0.405022415424763,-1.9544434175758,17.9050409366347));
#24347=CARTESIAN_POINT('Ctrl Pts',(0.473147181007539,-1.9390766278222,17.90947915987));
#24348=CARTESIAN_POINT('Ctrl Pts',(0.540247527698153,-1.92019795107589,
17.9139173831053));
#24349=CARTESIAN_POINT('Ctrl Pts',(0.607418959801008,-1.90129927445498,
17.9183603081484));
#24350=CARTESIAN_POINT('Ctrl Pts',(0.673563334683393,-1.87888141784204,
17.9228032331914));
#24351=CARTESIAN_POINT('Ctrl Pts',(0.738295510370425,-1.85309128265903,
17.9272461582344));
#24352=CARTESIAN_POINT('Ctrl Pts',(0.803065472892864,-1.82728609271255,
17.9316916767957));
#24353=CARTESIAN_POINT('Ctrl Pts',(0.866421150631294,-1.79810491091656,
17.9361371953569));
#24354=CARTESIAN_POINT('Ctrl Pts',(0.927999890924212,-1.765741703915,17.9405827139182));
#24355=CARTESIAN_POINT('Ctrl Pts',(0.989686087837908,-1.73332202221381,
17.9450359900334));
#24356=CARTESIAN_POINT('Ctrl Pts',(1.0495887367749,-1.69770948122588,17.9494892661486));
#24357=CARTESIAN_POINT('Ctrl Pts',(1.10737284860007,-1.65914222919054,17.9539425422639));
#24358=CARTESIAN_POINT('Ctrl Pts',(1.13831457879753,-1.63849057479555,17.9563271435617));
#24359=CARTESIAN_POINT('Ctrl Pts',(1.16864940321442,-1.6169924285982,17.9587117448595));
#24360=CARTESIAN_POINT('Ctrl Pts',(1.1983299490112,-1.59468896522263,17.9610963461574));
#24361=CARTESIAN_POINT('Ctrl Pts',(1.25376827334243,-1.55302980420884,17.9655503848754));
#24362=CARTESIAN_POINT('Ctrl Pts',(1.30714141940108,-1.50839377884732,17.9700044235934));
#24363=CARTESIAN_POINT('Ctrl Pts',(1.35811196655997,-1.46101315832083,17.9744584623113));
#24364=CARTESIAN_POINT('Ctrl Pts',(1.40900589706705,-1.41370375822865,17.9789058059171));
#24365=CARTESIAN_POINT('Ctrl Pts',(1.45750404091836,-1.36365828176769,17.9833531495229));
#24366=CARTESIAN_POINT('Ctrl Pts',(1.50330038120899,-1.31115045908428,17.9878004931286));
#24367=CARTESIAN_POINT('Ctrl Pts',(1.54904273232183,-1.25870453772652,17.9922425937734));
#24368=CARTESIAN_POINT('Ctrl Pts',(1.59208928574462,-1.20380240274425,17.9966846944182));
#24369=CARTESIAN_POINT('Ctrl Pts',(1.63217068887368,-1.14675472742937,18.001126795063));
#24370=CARTESIAN_POINT('Ctrl Pts',(1.6722268084761,-1.08974303804079,18.005566093611));
#24371=CARTESIAN_POINT('Ctrl Pts',(1.70932120749868,-1.03058889283162,18.0100053921591));
#24372=CARTESIAN_POINT('Ctrl Pts',(1.74322563959379,-0.969634947783344,
18.0144446907071));
#24373=CARTESIAN_POINT('Ctrl Pts',(1.77712020542982,-0.908698740457763,
18.0188826974101));
#24374=CARTESIAN_POINT('Ctrl Pts',(1.80782640928376,-0.845964200622262,
18.0233207041132));
#24375=CARTESIAN_POINT('Ctrl Pts',(1.83516100802873,-0.781800253972191,
18.0277587108163));
#24376=CARTESIAN_POINT('Ctrl Pts',(1.86249694044043,-0.717633176735796,
18.0321969340516));
#24377=CARTESIAN_POINT('Ctrl Pts',(1.88646075147374,-0.652037005553244,
18.0366351572869));
#24378=CARTESIAN_POINT('Ctrl Pts',(1.90691728457396,-0.585400745039742,
18.0410733805222));
#24379=CARTESIAN_POINT('Ctrl Pts',(1.92739548911345,-0.51869389076208,18.0455163055652));
#24380=CARTESIAN_POINT('Ctrl Pts',(1.94435885565362,-0.450945216831616,
18.0499592306083));
#24381=CARTESIAN_POINT('Ctrl Pts',(1.95772237224233,-0.382558068431269,
18.0544021556513));
#24382=CARTESIAN_POINT('Ctrl Pts',(1.97109368966573,-0.314130999637519,
18.0588476742125));
#24383=CARTESIAN_POINT('Ctrl Pts',(1.98086090600766,-0.245065199434764,
18.0632931927738));
#24384=CARTESIAN_POINT('Ctrl Pts',(1.98699075573615,-0.175770586615263,
18.0677387113351));
#24385=CARTESIAN_POINT('Ctrl Pts',(1.99313130222353,-0.106355052762036,
18.0721919874503));
#24386=CARTESIAN_POINT('Ctrl Pts',(1.99562179424232,-0.0367103984459924,
18.0766452635655));
#24387=CARTESIAN_POINT('Ctrl Pts',(1.99448108963014,0.0327527954193907,
18.0810985396808));
#24388=CARTESIAN_POINT('Ctrl Pts',(1.99387027511332,0.069948338195728,18.0834831409786));
#24389=CARTESIAN_POINT('Ctrl Pts',(1.99221918026625,0.107091921061017,18.0858677422763));
#24390=CARTESIAN_POINT('Ctrl Pts',(1.98953677474741,0.144121422514747,18.0882523435741));
#24391=CARTESIAN_POINT('Ctrl Pts',(1.98452648726271,0.21328637404612,18.0927063822921));
#24392=CARTESIAN_POINT('Ctrl Pts',(1.97589526670082,0.282326721031587,18.0971604210101));
#24393=CARTESIAN_POINT('Ctrl Pts',(1.96365571159974,0.350833021253317,18.1016144597281));
#24394=CARTESIAN_POINT('Ctrl Pts',(1.95143455445166,0.419236345861818,18.1060618033338));
#24395=CARTESIAN_POINT('Ctrl Pts',(1.93561591323597,0.487106738974794,18.1105091469396));
#24396=CARTESIAN_POINT('Ctrl Pts',(1.91626424745491,0.554038713833296,18.1149564905453));
#24397=CARTESIAN_POINT('Ctrl Pts',(1.89693539529866,0.620891782773368,18.1193985911901));
#24398=CARTESIAN_POINT('Ctrl Pts',(1.87408192625443,0.686808162678716,18.1238406918349));
#24399=CARTESIAN_POINT('Ctrl Pts',(1.84781921053907,0.751393191120845,18.1282827924797));
#24400=CARTESIAN_POINT('Ctrl Pts',(1.82157306146113,0.815937479040921,18.1327220910277));
#24401=CARTESIAN_POINT('Ctrl Pts',(1.79192211592647,0.879151629064188,18.1371613895757));
#24402=CARTESIAN_POINT('Ctrl Pts',(1.75903088925285,0.940658223349132,18.1416006881237));
#24403=CARTESIAN_POINT('Ctrl Pts',(1.72614923399345,1.00214691908934,18.1460386948268));
#24404=CARTESIAN_POINT('Ctrl Pts',(1.69002940019957,1.06192861403172,18.1504767015299));
#24405=CARTESIAN_POINT('Ctrl Pts',(1.65088235492533,1.11964950439689,18.1549147082329));
#24406=CARTESIAN_POINT('Ctrl Pts',(1.61173339965005,1.17737321098893,18.1593529314682));
#24407=CARTESIAN_POINT('Ctrl Pts',(1.56955721642649,1.23303550955568,18.1637911547035));
#24408=CARTESIAN_POINT('Ctrl Pts',(1.52460768845155,1.2863121545,18.1682293779388));
#24409=CARTESIAN_POINT('Ctrl Pts',(1.47961054141226,1.33964524017013,18.1726723029819));
#24410=CARTESIAN_POINT('Ctrl Pts',(1.43183450173105,1.39058725285202,18.1771152280249));
#24411=CARTESIAN_POINT('Ctrl Pts',(1.38157265842686,1.43884834224714,18.1815581530679));
#24412=CARTESIAN_POINT('Ctrl Pts',(1.33128147521591,1.4871376036266,18.1860036716292));
#24413=CARTESIAN_POINT('Ctrl Pts',(1.27850197074633,1.53274250665963,18.1904491901904));
#24414=CARTESIAN_POINT('Ctrl Pts',(1.22356077697345,1.57541314820974,18.1948947087517));
#24415=CARTESIAN_POINT('Ctrl Pts',(1.16852370928375,1.61815825122051,18.1993479848669));
#24416=CARTESIAN_POINT('Ctrl Pts',(1.11131782411176,1.65795859201021,18.2038012609821));
#24417=CARTESIAN_POINT('Ctrl Pts',(1.05229853030599,1.6946077320772,18.2082545370974));
#24418=CARTESIAN_POINT('Ctrl Pts',(1.02069539567785,1.71423229267183,18.2106391383952));
#24419=CARTESIAN_POINT('Ctrl Pts',(0.988572726641358,1.73295409804132,18.213023739693));
#24420=CARTESIAN_POINT('Ctrl Pts',(0.955987608594783,1.75074705617723,18.2154083409909));
#24421=CARTESIAN_POINT('Ctrl Pts',(0.895124026266901,1.78398134340042,18.2198623797088));
#24422=CARTESIAN_POINT('Ctrl Pts',(0.832404790085185,1.81410384152131,18.2243164184268));
#24423=CARTESIAN_POINT('Ctrl Pts',(0.768180962672243,1.84090346598836,18.2287704571448));
#24424=CARTESIAN_POINT('Ctrl Pts',(0.704053673650548,1.86766280645589,18.2332178007506));
#24425=CARTESIAN_POINT('Ctrl Pts',(0.638426730301333,1.89110899970459,18.2376651443563));
#24426=CARTESIAN_POINT('Ctrl Pts',(0.571675947805817,1.91107670521105,18.2421124879621));
#24427=CARTESIAN_POINT('Ctrl Pts',(0.505003857621541,1.9310208708452,18.2465545886069));
#24428=CARTESIAN_POINT('Ctrl Pts',(0.437211026452579,1.94749455377516,18.2509966892517));
#24429=CARTESIAN_POINT('Ctrl Pts',(0.36869173250688,1.96038107746455,18.2554387898964));
#24430=CARTESIAN_POINT('Ctrl Pts',(0.300215660835344,1.97325947227772,18.2598780884445));
#24431=CARTESIAN_POINT('Ctrl Pts',(0.231014515470778,1.98255510644078,18.2643173869925));
#24432=CARTESIAN_POINT('Ctrl Pts',(0.16149468384471,1.98820195895435,18.2687566855405));
#24433=CARTESIAN_POINT('Ctrl Pts',(0.0919950826318286,1.99384716822228,
18.2731946922436));
#24434=CARTESIAN_POINT('Ctrl Pts',(0.0221774669620181,1.9958456640726,18.2776326989466));
#24435=CARTESIAN_POINT('Ctrl Pts',(-0.04754647991321,1.9941832650857,18.2820707056497));
#24436=CARTESIAN_POINT('Ctrl Pts',(-0.117273828649554,1.99252078498964,
18.286508928885));
#24437=CARTESIAN_POINT('Ctrl Pts',(-0.186907010153732,1.98719706949691,
18.2909471521203));
#24438=CARTESIAN_POINT('Ctrl Pts',(-0.25603595713023,1.97825002240779,18.2953853753556));
#24439=CARTESIAN_POINT('Ctrl Pts',(-0.325238138597088,1.96929349690966,
18.2998283003986));
#24440=CARTESIAN_POINT('Ctrl Pts',(-0.393934532857344,1.95670604127559,
18.3042712254417));
#24441=CARTESIAN_POINT('Ctrl Pts',(-0.461722764225033,1.94057714391786,
18.3087141504847));
#24442=CARTESIAN_POINT('Ctrl Pts',(-0.529550566373594,1.92443883145886,
18.3131596690459));
#24443=CARTESIAN_POINT('Ctrl Pts',(-0.5964686806551,1.90475510077308,18.3176051876072));
#24444=CARTESIAN_POINT('Ctrl Pts',(-0.662090156717492,1.88166526961567,
18.3220507061684));
#24445=CARTESIAN_POINT('Ctrl Pts',(-0.727826144087432,1.85853514605834,
18.3265039822837));
#24446=CARTESIAN_POINT('Ctrl Pts',(-0.792260523944197,1.83198724373524,
18.3309572583989));
#24447=CARTESIAN_POINT('Ctrl Pts',(-0.855027309003584,1.80220860705915,
18.3354105345142));
#24448=CARTESIAN_POINT('Ctrl Pts',(-0.888637117431817,1.78626300345702,
18.337795135812));
#24449=CARTESIAN_POINT('Ctrl Pts',(-0.921769209696405,1.7693918350193,18.3401797371097));
#24450=CARTESIAN_POINT('Ctrl Pts',(-0.954370742034073,1.75162897020155,
18.3425643384075));
#24451=CARTESIAN_POINT('Ctrl Pts',(-1.01526498352919,1.71845089229238,18.3470183771255));
#24452=CARTESIAN_POINT('Ctrl Pts',(-1.07454763790588,1.68202789996184,18.3514724158435));
#24453=CARTESIAN_POINT('Ctrl Pts',(-1.1318511647767,1.6425408680741,18.3559264545615));
#24454=CARTESIAN_POINT('Ctrl Pts',(-1.18906855554323,1.6031131913305,18.3603737981672));
#24455=CARTESIAN_POINT('Ctrl Pts',(-1.24431232347915,1.56063089177578,18.364821141773));
#24456=CARTESIAN_POINT('Ctrl Pts',(-1.29723998650435,1.51532042153275,18.3692684853788));
#24457=CARTESIAN_POINT('Ctrl Pts',(-1.35010525325527,1.47006336767668,18.3737105860235));
#24458=CARTESIAN_POINT('Ctrl Pts',(-1.40065946801004,1.42198508195742,18.3781526866683));
#24459=CARTESIAN_POINT('Ctrl Pts',(-1.44859106720036,1.37135388668547,18.3825947873131));
#24460=CARTESIAN_POINT('Ctrl Pts',(-1.49649243092557,1.32075462979579,18.3870340858611));
#24461=CARTESIAN_POINT('Ctrl Pts',(-1.54177412516799,1.26760601268498,18.3914733844091));
#24462=CARTESIAN_POINT('Ctrl Pts',(-1.584160619306,1.21221396409217,18.3959126829572));
#24463=CARTESIAN_POINT('Ctrl Pts',(-1.62653477888753,1.15683803469877,18.4003506896602));
#24464=CARTESIAN_POINT('Ctrl Pts',(-1.66601511352324,1.09922035841337,18.4047886963633));
#24465=CARTESIAN_POINT('Ctrl Pts',(-1.70236680988852,1.03969938303819,18.4092267030663));
#24466=CARTESIAN_POINT('Ctrl Pts',(-1.73872027986857,0.980175503609246,
18.4136649263016));
#24467=CARTESIAN_POINT('Ctrl Pts',(-1.77194455539026,0.918748559772755,
18.4181031495369));
#24468=CARTESIAN_POINT('Ctrl Pts',(-1.80184948906721,0.855783840258872,
18.4225413727722));
#24469=CARTESIAN_POINT('Ctrl Pts',(-1.83178610372115,0.792752416573324,
18.4269842978153));
#24470=CARTESIAN_POINT('Ctrl Pts',(-1.8583961473623,0.728180408697531,18.4314272228583));
#24471=CARTESIAN_POINT('Ctrl Pts',(-1.88153700708338,0.662454567103078,
18.4358701479013));
#24472=CARTESIAN_POINT('Ctrl Pts',(-1.90469137507678,0.596690358629536,
18.4403156664626));
#24473=CARTESIAN_POINT('Ctrl Pts',(-1.92437239023596,0.529771445645212,
18.4447611850238));
#24474=CARTESIAN_POINT('Ctrl Pts',(-1.94048768550706,0.462098587852696,
18.4492067035851));
#24475=CARTESIAN_POINT('Ctrl Pts',(-1.95663110241826,0.394307639034258,
18.4536599797003));
#24476=CARTESIAN_POINT('Ctrl Pts',(-1.96919629039305,0.325760600612199,
18.4581132558155));
#24477=CARTESIAN_POINT('Ctrl Pts',(-1.9781423585773,0.256866447209936,18.4625665319308));
#24478=CARTESIAN_POINT('Ctrl Pts',(-1.9829327208299,0.219975609236646,18.4649511332286));
#24479=CARTESIAN_POINT('Ctrl Pts',(-1.98668626629364,0.182985302955157,
18.4673357345265));
#24480=CARTESIAN_POINT('Ctrl Pts',(-1.98940285988789,0.145958293940053,
18.4697203358243));
#24481=CARTESIAN_POINT('Ctrl Pts',(-1.99294386346392,0.0976946259368988,
18.4728285967512));
#24482=CARTESIAN_POINT('Ctrl Pts',(-1.99472877578325,0.0493005479635618,
18.475936857678));
#24483=CARTESIAN_POINT('Ctrl Pts',(-1.9947498118588,0.000866365563832799,
18.4790451186048));
#24484=CARTESIAN_POINT('',(-1.99474923905823,0.00174234801668578,16.07864965537));
#24485=CARTESIAN_POINT('Ctrl Pts',(-1.99474916465594,-0.00182554222757092,
17.6788731275167));
#24486=CARTESIAN_POINT('Ctrl Pts',(-1.99487395459297,0.134530998253091,
17.670963424711));
#24487=CARTESIAN_POINT('Ctrl Pts',(-1.98101782634591,0.27053147043171,17.6630747226269));
#24488=CARTESIAN_POINT('Ctrl Pts',(-1.94710945436344,0.434461068927948,
17.6528395731388));
#24489=CARTESIAN_POINT('Ctrl Pts',(-1.94011125517069,0.46471475362475,17.650921029371));
#24490=CARTESIAN_POINT('Ctrl Pts',(-1.93038367435289,0.502705853059274,
17.6484692026851));
#24491=CARTESIAN_POINT('Ctrl Pts',(-1.92830865321938,0.51060752018063,17.6479569106788));
#24492=CARTESIAN_POINT('Ctrl Pts',(-1.924748354045,0.523833839833939,17.6470953706912));
#24493=CARTESIAN_POINT('Ctrl Pts',(-1.9232893632645,0.529165515045873,17.6467469715466));
#24494=CARTESIAN_POINT('Ctrl Pts',(-1.920371999549,0.539655146275757,17.6460593176069));
#24495=CARTESIAN_POINT('Ctrl Pts',(-1.91891495969128,0.544813426882911,
17.6457201085009));
#24496=CARTESIAN_POINT('Ctrl Pts',(-1.91610356314825,0.554615267053036,
17.6450735025496));
#24497=CARTESIAN_POINT('Ctrl Pts',(-1.91475307020975,0.559259902552393,
17.6447662336324));
#24498=CARTESIAN_POINT('Ctrl Pts',(-1.91163787743441,0.569830163452721,
17.6440649396523));
#24499=CARTESIAN_POINT('Ctrl Pts',(-1.90986250055745,0.575752565920685,
17.6436705680794));
#24500=CARTESIAN_POINT('Ctrl Pts',(-1.90435976063781,0.59380338157505,17.6424640987922));
#24501=CARTESIAN_POINT('Ctrl Pts',(-1.90054424364274,0.60590438147918,17.6416491218866));
#24502=CARTESIAN_POINT('Ctrl Pts',(-1.84952423406113,0.762490573328746,
17.6310212559867));
#24503=CARTESIAN_POINT('Ctrl Pts',(-1.78608076665082,0.90112636964128,17.6206419784212));
#24504=CARTESIAN_POINT('Ctrl Pts',(-1.6759606198772,1.08347319351912,17.6058018110514));
#24505=CARTESIAN_POINT('Ctrl Pts',(-1.64200105005281,1.13427986927447,17.6015290705849));
#24506=CARTESIAN_POINT('Ctrl Pts',(-1.55831260082218,1.24783264721737,17.5917470438183));
#24507=CARTESIAN_POINT('Ctrl Pts',(-1.50702614473421,1.3093126943296,17.5862718391463));
#24508=CARTESIAN_POINT('Ctrl Pts',(-1.44522760426659,1.37493548182497,17.580360339955));
#24509=CARTESIAN_POINT('Ctrl Pts',(-1.43821863299528,1.38226538027678,17.579699067453));
#24510=CARTESIAN_POINT('Ctrl Pts',(-1.4289912435603,1.39176909963981,17.5788407833141));
#24511=CARTESIAN_POINT('Ctrl Pts',(-1.42682338372019,1.39399147517855,17.5786400149043));
#24512=CARTESIAN_POINT('Ctrl Pts',(-1.42255686880042,1.3983449013131,17.5782466172185));
#24513=CARTESIAN_POINT('Ctrl Pts',(-1.42045859245903,1.40047631018831,17.5780539596466));
#24514=CARTESIAN_POINT('Ctrl Pts',(-1.41644414634149,1.40453584217814,17.577686933256));
#24515=CARTESIAN_POINT('Ctrl Pts',(-1.41452885263436,1.40646474424731,17.5775125037478));
#24516=CARTESIAN_POINT('Ctrl Pts',(-1.4100983845802,1.41090848691685,17.5771105636285));
#24517=CARTESIAN_POINT('Ctrl Pts',(-1.40758042355766,1.41342051928855,17.5768832766234));
#24518=CARTESIAN_POINT('Ctrl Pts',(-1.39948007435782,1.42145868192833,17.5761557040853));
#24519=CARTESIAN_POINT('Ctrl Pts',(-1.39387167195694,1.42695866442534,17.5756574400135));
#24520=CARTESIAN_POINT('Ctrl Pts',(-1.31909689409082,1.49942641378923,17.5690840964259));
#24521=CARTESIAN_POINT('Ctrl Pts',(-1.24519239302094,1.56134477679806,17.5633713287119));
#24522=CARTESIAN_POINT('Ctrl Pts',(-1.09137028803074,1.67232089231421,17.552289429932));
#24523=CARTESIAN_POINT('Ctrl Pts',(-1.01190424536467,1.72156796591944,17.546926926072));
#24524=CARTESIAN_POINT('Ctrl Pts',(-0.864738636181897,1.79904835912485,
17.5371847851522));
#24525=CARTESIAN_POINT('Ctrl Pts',(-0.798386657545375,1.82946036537168,
17.5328555983323));
#24526=CARTESIAN_POINT('Ctrl Pts',(-0.706536243996306,1.86560943166117,
17.5268390736166));
#24527=CARTESIAN_POINT('Ctrl Pts',(-0.682370196143658,1.87458337773705,
17.5252542883188));
#24528=CARTESIAN_POINT('Ctrl Pts',(-0.640982683262154,1.88904609805361,
17.5225329154798));
#24529=CARTESIAN_POINT('Ctrl Pts',(-0.623847806683709,1.89477382321997,
17.5214041780342));
#24530=CARTESIAN_POINT('Ctrl Pts',(-0.601396601373318,1.90194110359519,
17.5199216863733));
#24531=CARTESIAN_POINT('Ctrl Pts',(-0.59614841915814,1.90359262843793,17.519574889705));
#24532=CARTESIAN_POINT('Ctrl Pts',(-0.58579112517895,1.90680488219416,17.5188899614425));
#24533=CARTESIAN_POINT('Ctrl Pts',(-0.580682441201451,1.90836684174517,
17.5185518733498));
#24534=CARTESIAN_POINT('Ctrl Pts',(-0.570932421228476,1.91130509569048,
17.5179061223116));
#24535=CARTESIAN_POINT('Ctrl Pts',(-0.56629222205078,1.9126850543119,17.5175985818367));
#24536=CARTESIAN_POINT('Ctrl Pts',(-0.555682341862649,1.91579835549853,
17.5168948701816));
#24537=CARTESIAN_POINT('Ctrl Pts',(-0.549709512588068,1.91752070505459,
17.5164983436752));
#24538=CARTESIAN_POINT('Ctrl Pts',(-0.531357805844762,1.92271988844064,
17.5152788064337));
#24539=CARTESIAN_POINT('Ctrl Pts',(-0.51895347607888,1.9261049203074,17.5144528246592));
#24540=CARTESIAN_POINT('Ctrl Pts',(-0.404234574888088,1.95622207876314,
17.5067972944854));
#24541=CARTESIAN_POINT('Ctrl Pts',(-0.299995801873904,1.97489400501435,
17.4997058203022));
#24542=CARTESIAN_POINT('Ctrl Pts',(-0.0624775108408705,1.99819855041709,
17.483290746562));
#24543=CARTESIAN_POINT('Ctrl Pts',(0.0707869734158899,1.997920917267,17.4738939159684));
#24544=CARTESIAN_POINT('Ctrl Pts',(0.243123709943663,1.98028855865138,17.4620133766614));
#24545=CARTESIAN_POINT('Ctrl Pts',(0.283086946734378,1.97497193298334,17.4592801937768));
#24546=CARTESIAN_POINT('Ctrl Pts',(0.343984641105148,1.96498351243578,17.4551743703625));
#24547=CARTESIAN_POINT('Ctrl Pts',(0.365049075388629,1.96117946707962,17.4537651450919));
#24548=CARTESIAN_POINT('Ctrl Pts',(0.391199455421058,1.95602098801509,17.4520327417419));
#24549=CARTESIAN_POINT('Ctrl Pts',(0.396345722642714,1.95498470304402,17.4516926410067));
#24550=CARTESIAN_POINT('Ctrl Pts',(0.404507720269038,1.95330759764672,17.4511546199647));
#24551=CARTESIAN_POINT('Ctrl Pts',(0.407526113864646,1.95268008993195,17.4509559541228));
#24552=CARTESIAN_POINT('Ctrl Pts',(0.413183155429322,1.95149033329523,17.4505841952418));
#24553=CARTESIAN_POINT('Ctrl Pts',(0.415822087194919,1.95092973548234,17.4504110131692));
#24554=CARTESIAN_POINT('Ctrl Pts',(0.421836151923533,1.9496393889866,17.4500168701501));
#24555=CARTESIAN_POINT('Ctrl Pts',(0.425210525409237,1.9489062306018,17.4497961071131));
#24556=CARTESIAN_POINT('Ctrl Pts',(0.4355326280605,1.94663543763054,17.4491219248841));
#24557=CARTESIAN_POINT('Ctrl Pts',(0.442474142468444,1.94506936484769,17.4486701055179));
#24558=CARTESIAN_POINT('Ctrl Pts',(0.497199082655915,1.93241476572177,17.4451193580921));
#24559=CARTESIAN_POINT('Ctrl Pts',(0.544571677684162,1.91960317864502,17.4421134787008));
#24560=CARTESIAN_POINT('Ctrl Pts',(0.762228981851611,1.85203111125313,17.4284160925313));
#24561=CARTESIAN_POINT('Ctrl Pts',(0.925130804134118,1.7762757317428,17.4184207779021));
#24562=CARTESIAN_POINT('Ctrl Pts',(1.116064141616,1.65400087529898,17.4049080011937));
#24563=CARTESIAN_POINT('Ctrl Pts',(1.15542269983746,1.6267501171322,17.4020181171983));
#24564=CARTESIAN_POINT('Ctrl Pts',(1.21701323180001,1.58074307968851,17.3972935852474));
#24565=CARTESIAN_POINT('Ctrl Pts',(1.23988233875269,1.56286964916456,17.395491904199));
#24566=CARTESIAN_POINT('Ctrl Pts',(1.26876742393338,1.53926132518276,17.3931503896267));
#24567=CARTESIAN_POINT('Ctrl Pts',(1.27514954346977,1.53397843586224,17.3926287898682));
#24568=CARTESIAN_POINT('Ctrl Pts',(1.28562526378452,1.52519646023876,17.3917654928271));
#24569=CARTESIAN_POINT('Ctrl Pts',(1.28973797752693,1.52172024682695,17.3914247306714));
#24570=CARTESIAN_POINT('Ctrl Pts',(1.29751415308781,1.51509337414078,17.3907769069641));
#24571=CARTESIAN_POINT('Ctrl Pts',(1.30118034743469,1.51194596881081,17.3904699808064));
#24572=CARTESIAN_POINT('Ctrl Pts',(1.30947807645864,1.50476988641005,17.3897718745778));
#24573=CARTESIAN_POINT('Ctrl Pts',(1.31410250587305,1.50073310299943,17.3893803596675));
#24574=CARTESIAN_POINT('Ctrl Pts',(1.32599016035539,1.49025898771593,17.3883675248174));
#24575=CARTESIAN_POINT('Ctrl Pts',(1.33322510246685,1.48378993676585,17.38774488081));
#24576=CARTESIAN_POINT('Ctrl Pts',(1.35184711078189,1.46689309459556,17.3861258747288));
#24577=CARTESIAN_POINT('Ctrl Pts',(1.36316065166095,1.45638558677678,17.3851261552643));
#24578=CARTESIAN_POINT('Ctrl Pts',(1.49057017060994,1.33526809529004,17.373680142492));
#24579=CARTESIAN_POINT('Ctrl Pts',(1.59302136640857,1.21119898262068,17.3626082962276));
#24580=CARTESIAN_POINT('Ctrl Pts',(1.72227981449997,1.00948786995335,17.3458928314113));
#24581=CARTESIAN_POINT('Ctrl Pts',(1.76104082694941,0.940239339496951,17.3403617362564));
#24582=CARTESIAN_POINT('Ctrl Pts',(1.8092549393652,0.840600968220298,17.3328304511581));
#24583=CARTESIAN_POINT('Ctrl Pts',(1.82226292602302,0.81201692345694,17.3307168918657));
#24584=CARTESIAN_POINT('Ctrl Pts',(1.8416583609076,0.76658076250785,17.3274431509721));
#24585=CARTESIAN_POINT('Ctrl Pts',(1.84850126083855,0.749929815619094,17.3262611961893));
#24586=CARTESIAN_POINT('Ctrl Pts',(1.85693939906319,0.728579565859989,17.3247702641461));
#24587=CARTESIAN_POINT('Ctrl Pts',(1.85874353850996,0.723964484563416,17.3244494372982));
#24588=CARTESIAN_POINT('Ctrl Pts',(1.86160994577561,0.716550718727087,17.3239364380792));
#24589=CARTESIAN_POINT('Ctrl Pts',(1.86268312895095,0.713756319853589,17.3237436197941));
#24590=CARTESIAN_POINT('Ctrl Pts',(1.8647186077025,0.708420399012569,17.3233764790212));
#24591=CARTESIAN_POINT('Ctrl Pts',(1.86568198801607,0.705879357482266,17.323202095062));
#24592=CARTESIAN_POINT('Ctrl Pts',(1.86789251884577,0.700012653868794,17.3228005141895));
#24593=CARTESIAN_POINT('Ctrl Pts',(1.86913598160927,0.696685625133023,17.3225735395823));
#24594=CARTESIAN_POINT('Ctrl Pts',(1.87245107034768,0.687742959324083,17.3219654606523));
#24595=CARTESIAN_POINT('Ctrl Pts',(1.8745063380064,0.682121235493444,17.3215853130878));
#24596=CARTESIAN_POINT('Ctrl Pts',(1.88937630048065,0.640873007640733,17.3188109393327));
#24597=CARTESIAN_POINT('Ctrl Pts',(1.90120068030406,0.604894570267783,17.3164721232632));
#24598=CARTESIAN_POINT('Ctrl Pts',(1.93611125092309,0.487502755861741,17.3090349507673));
#24599=CARTESIAN_POINT('Ctrl Pts',(1.95504617159904,0.404947620795662,17.3040992794347));
#24600=CARTESIAN_POINT('Ctrl Pts',(1.98491677013169,0.2219993225217,17.2933351849493));
#24601=CARTESIAN_POINT('Ctrl Pts',(1.99359467703481,0.121480170666097,17.2875272621031));
#24602=CARTESIAN_POINT('Ctrl Pts',(1.9951754586604,-0.030546742864486,17.2784921451381));
#24603=CARTESIAN_POINT('Ctrl Pts',(1.99373045716577,-0.0818319821665538,
17.2754028734052));
#24604=CARTESIAN_POINT('Ctrl Pts',(1.9882691649609,-0.163557695667005,17.2703755639381));
#24605=CARTESIAN_POINT('Ctrl Pts',(1.98552399341436,-0.194061084227873,
17.2684759686639));
#24606=CARTESIAN_POINT('Ctrl Pts',(1.9810981674322,-0.233138154838589,17.2660079670331));
#24607=CARTESIAN_POINT('Ctrl Pts',(1.98006185204967,-0.241781733039885,
17.2654598937993));
#24608=CARTESIAN_POINT('Ctrl Pts',(1.97829918292811,-0.255711504780833,
17.2645730265905));
#24609=CARTESIAN_POINT('Ctrl Pts',(1.97760813234482,-0.261002116528721,
17.2642353485687));
#24610=CARTESIAN_POINT('Ctrl Pts',(1.97624940029182,-0.271089139291165,
17.263589904937));
#24611=CARTESIAN_POINT('Ctrl Pts',(1.97558546139651,-0.275886022905429,
17.2632822597861));
#24612=CARTESIAN_POINT('Ctrl Pts',(1.97402761864393,-0.286847208341354,
17.2625776378948));
#24613=CARTESIAN_POINT('Ctrl Pts',(1.97312229944541,-0.293009812256648,
17.2621803025157));
#24614=CARTESIAN_POINT('Ctrl Pts',(1.97025015004233,-0.311943717804821,
17.2609558396116));
#24615=CARTESIAN_POINT('Ctrl Pts',(1.96818810476172,-0.324700027764395,
17.2601257060466));
#24616=CARTESIAN_POINT('Ctrl Pts',(1.94732285168643,-0.446267489545338,
17.2521637323949));
#24617=CARTESIAN_POINT('Ctrl Pts',(1.91964228926552,-0.553341642130039,
17.2447451458188));
#24618=CARTESIAN_POINT('Ctrl Pts',(1.8265155066649,-0.820056361734216,17.2252779390862));
#24619=CARTESIAN_POINT('Ctrl Pts',(1.74898854175703,-0.974521106123854,
17.212998329644));
#24620=CARTESIAN_POINT('Ctrl Pts',(1.64226299508886,-1.13240467184797,17.2003629896625));
#24621=CARTESIAN_POINT('Ctrl Pts',(1.63171652882727,-1.14754926495797,17.1991508671861));
#24622=CARTESIAN_POINT('Ctrl Pts',(1.61804796396616,-1.16660761668881,17.1976275742049));
#24623=CARTESIAN_POINT('Ctrl Pts',(1.61511967513087,-1.17065835380331,17.1973039287264));
#24624=CARTESIAN_POINT('Ctrl Pts',(1.61040769947528,-1.17712515137752,17.1967874961048));
#24625=CARTESIAN_POINT('Ctrl Pts',(1.60863375268652,-1.17954823154703,17.1965940478792));
#24626=CARTESIAN_POINT('Ctrl Pts',(1.60524571220301,-1.18415418590358,17.1962264513651));
#24627=CARTESIAN_POINT('Ctrl Pts',(1.6036326541947,-1.1863377440762,17.1960522385548));
#24628=CARTESIAN_POINT('Ctrl Pts',(1.59991018454899,-1.19135529740016,17.1956520324233));
#24629=CARTESIAN_POINT('Ctrl Pts',(1.59779769967947,-1.1941869847874,17.1954262564242));
#24630=CARTESIAN_POINT('Ctrl Pts',(1.59212477184885,-1.20174927842679,17.1948234774285));
#24631=CARTESIAN_POINT('Ctrl Pts',(1.58855073766808,-1.20646971504061,17.1944474052699));
#24632=CARTESIAN_POINT('Ctrl Pts',(1.562781877784,-1.24019112326695,17.191761637912));
#24633=CARTESIAN_POINT('Ctrl Pts',(1.53981368369376,-1.26859585657837,17.189503459316));
#24634=CARTESIAN_POINT('Ctrl Pts',(1.46672571093517,-1.35407158985838,17.1826648983127));
#24635=CARTESIAN_POINT('Ctrl Pts',(1.41411493503509,-1.40892689903081,17.1782126288713));
#24636=CARTESIAN_POINT('Ctrl Pts',(1.28219160979058,-1.53162405966886,17.1677309272256));
#24637=CARTESIAN_POINT('Ctrl Pts',(1.20044138780058,-1.59650472294606,17.1617414827155));
#24638=CARTESIAN_POINT('Ctrl Pts',(1.0677793481733,-1.68581706743439,17.152270370152));
#24639=CARTESIAN_POINT('Ctrl Pts',(1.02028056041973,-1.71498068526348,17.1489250403128));
#24640=CARTESIAN_POINT('Ctrl Pts',(0.94323528179161,-1.75795094732029,17.1435189131193));
#24641=CARTESIAN_POINT('Ctrl Pts',(0.914462973075244,-1.77308815665554,
17.1415044638148));
#24642=CARTESIAN_POINT('Ctrl Pts',(0.877370034870741,-1.79145984757148,
17.1389074667355));
#24643=CARTESIAN_POINT('Ctrl Pts',(0.86937901241561,-1.79535141189792,17.1383479982075));
#24644=CARTESIAN_POINT('Ctrl Pts',(0.856513166103216,-1.80151093890031,
17.1374471338763));
#24645=CARTESIAN_POINT('Ctrl Pts',(0.851654654282618,-1.8038128549274,17.1371069193846));
#24646=CARTESIAN_POINT('Ctrl Pts',(0.842410439321841,-1.80814700129685,
17.1364595293659));
#24647=CARTESIAN_POINT('Ctrl Pts',(0.838026532360741,-1.8101829899104,17.1361524866121));
#24648=CARTESIAN_POINT('Ctrl Pts',(0.828044589280915,-1.81477480444193,
17.1354532768966));
#24649=CARTESIAN_POINT('Ctrl Pts',(0.822442059805473,-1.81732068978892,
17.1350607710491));
#24650=CARTESIAN_POINT('Ctrl Pts',(0.805385313501111,-1.82497653954453,
17.1338655526949));
#24651=CARTESIAN_POINT('Ctrl Pts',(0.793894774412921,-1.8300043574555,17.1330600389029));
#24652=CARTESIAN_POINT('Ctrl Pts',(0.637986768271091,-1.89647898274159,
17.1221242777255));
#24653=CARTESIAN_POINT('Ctrl Pts',(0.486887043540393,-1.94076798098162,
17.1113867182223));
#24654=CARTESIAN_POINT('Ctrl Pts',(0.242529791646867,-1.98203842136501,
17.0941118802415));
#24655=CARTESIAN_POINT('Ctrl Pts',(0.151929380314377,-1.99103383645298,
17.0877416606701));
#24656=CARTESIAN_POINT('Ctrl Pts',(0.0267245857756098,-1.99486621604645,
17.079194783896));
#24657=CARTESIAN_POINT('Ctrl Pts',(-0.00760291807186951,-1.99503080479141,
17.0768786512938));
#24658=CARTESIAN_POINT('Ctrl Pts',(-0.0610969171456245,-1.99390638240001,
17.0733280452297));
#24659=CARTESIAN_POINT('Ctrl Pts',(-0.0802683271625168,-1.99322666997899,
17.0720673510286));
#24660=CARTESIAN_POINT('Ctrl Pts',(-0.10448702612464,-1.99201799273349,
17.0704921300935));
#24661=CARTESIAN_POINT('Ctrl Pts',(-0.109545337950104,-1.99174622939305,
17.0701640894029));
#24662=CARTESIAN_POINT('Ctrl Pts',(-0.117615670421557,-1.99128180453433,
17.0696423040222));
#24663=CARTESIAN_POINT('Ctrl Pts',(-0.1206283415547,-1.99110157312717,17.0694478743199));
#24664=CARTESIAN_POINT('Ctrl Pts',(-0.126346204418445,-1.99074647998349,
17.0690795453665));
#24665=CARTESIAN_POINT('Ctrl Pts',(-0.129051415203062,-1.99057294346532,
17.0689055768848));
#24666=CARTESIAN_POINT('Ctrl Pts',(-0.135253177172652,-1.99016241101559,
17.0685074119068));
#24667=CARTESIAN_POINT('Ctrl Pts',(-0.138749459774596,-1.98992171504951,
17.0682834252993));
#24668=CARTESIAN_POINT('Ctrl Pts',(-0.149801121824968,-1.98913161237082,
17.0675768802434));
#24669=CARTESIAN_POINT('Ctrl Pts',(-0.157354128014693,-1.98854837261846,
17.0670961824657));
#24670=CARTESIAN_POINT('Ctrl Pts',(-0.286482863122264,-1.97783677806641,
17.0589124133052));
#24671=CARTESIAN_POINT('Ctrl Pts',(-0.406901684643899,-1.95661738195584,
17.0517943432779));
#24672=CARTESIAN_POINT('Ctrl Pts',(-0.621531346165174,-1.89810735803976,
17.0388781698789));
#24673=CARTESIAN_POINT('Ctrl Pts',(-0.716285588654842,-1.8644158780333,
17.033087291115));
#24674=CARTESIAN_POINT('Ctrl Pts',(-0.854615041238981,-1.80312218717505,
17.0240928161145));
#24675=CARTESIAN_POINT('Ctrl Pts',(-0.900325623519345,-1.78073851799526,
17.0210272342319));
#24676=CARTESIAN_POINT('Ctrl Pts',(-0.971940425098654,-1.7422073283255,
17.0160351231518));
#24677=CARTESIAN_POINT('Ctrl Pts',(-0.998417648215627,-1.72717011550998,
17.014146346494));
#24678=CARTESIAN_POINT('Ctrl Pts',(-1.03199354265398,-1.70707128356579,
17.0116905206944));
#24679=CARTESIAN_POINT('Ctrl Pts',(-1.03941845771678,-1.70256051439148,
17.0111435552908));
#24680=CARTESIAN_POINT('Ctrl Pts',(-1.05135203865993,-1.6952034920557,17.0102580486427));
#24681=CARTESIAN_POINT('Ctrl Pts',(-1.05587922910271,-1.69238737921352,
17.009920617077));
#24682=CARTESIAN_POINT('Ctrl Pts',(-1.06449756588004,-1.68697835053265,
17.0092753567829));
#24683=CARTESIAN_POINT('Ctrl Pts',(-1.06859067038259,-1.68438861353955,
17.0089676473002));
#24684=CARTESIAN_POINT('Ctrl Pts',(-1.07793221066091,-1.67843039902162,
17.0082624714675));
#24685=CARTESIAN_POINT('Ctrl Pts',(-1.08317434253265,-1.67505217750344,
17.0078646444645));
#24686=CARTESIAN_POINT('Ctrl Pts',(-1.09926199179173,-1.66457760979476,
17.0066371822756));
#24687=CARTESIAN_POINT('Ctrl Pts',(-1.11005408478666,-1.65740021156439,
17.0058045196354));
#24688=CARTESIAN_POINT('Ctrl Pts',(-1.21483242039514,-1.5862338189017,16.997628101887));
#24689=CARTESIAN_POINT('Ctrl Pts',(-1.30323839566535,-1.51443623268288,
16.9899794504521));
#24690=CARTESIAN_POINT('Ctrl Pts',(-1.50117195367957,-1.32346250925512,
16.9710030059021));
#24691=CARTESIAN_POINT('Ctrl Pts',(-1.60327818044759,-1.19773546977313,
16.9595208354585));
#24692=CARTESIAN_POINT('Ctrl Pts',(-1.70234762257109,-1.04002801779976,
16.9470843822573));
#24693=CARTESIAN_POINT('Ctrl Pts',(-1.71517890682172,-1.01872820959655,
16.9454432824012));
#24694=CARTESIAN_POINT('Ctrl Pts',(-1.73036593826448,-0.9924170944778,16.9434678090384));
#24695=CARTESIAN_POINT('Ctrl Pts',(-1.73310279663216,-0.987629823252238,
16.943110434944));
#24696=CARTESIAN_POINT('Ctrl Pts',(-1.73735586504191,-0.980118298975971,
16.9425529850741));
#24697=CARTESIAN_POINT('Ctrl Pts',(-1.738885573803,-0.977401781935186,16.9423520558596));
#24698=CARTESIAN_POINT('Ctrl Pts',(-1.74172491401848,-0.97233180554543,
16.9419783156686));
#24699=CARTESIAN_POINT('Ctrl Pts',(-1.74303613400936,-0.969979304860729,
16.9418054053613));
#24700=CARTESIAN_POINT('Ctrl Pts',(-1.74599288891186,-0.964649142550532,
16.9414147751311));
#24701=CARTESIAN_POINT('Ctrl Pts',(-1.7476355689051,-0.96166993041941,16.9411972394111));
#24702=CARTESIAN_POINT('Ctrl Pts',(-1.75246201799881,-0.95286333343815,
16.9405565178862));
#24703=CARTESIAN_POINT('Ctrl Pts',(-1.75562435909795,-0.947024165203018,
16.9401346774769));
#24704=CARTESIAN_POINT('Ctrl Pts',(-1.77737473607163,-0.906379360006077,
16.9372182765079));
#24705=CARTESIAN_POINT('Ctrl Pts',(-1.79495710862953,-0.871041893896169,
16.934783657536));
#24706=CARTESIAN_POINT('Ctrl Pts',(-1.8399626010414,-0.773429025800144,
16.9282666564147));
#24707=CARTESIAN_POINT('Ctrl Pts',(-1.86526793285316,-0.710233566745033,
16.9242705175052));
#24708=CARTESIAN_POINT('Ctrl Pts',(-1.91109806899398,-0.576312227966323,
16.9160255300904));
#24709=CARTESIAN_POINT('Ctrl Pts',(-1.93103697188816,-0.505497630126043,
16.9117879118472));
#24710=CARTESIAN_POINT('Ctrl Pts',(-1.97224754543779,-0.320508651458527,
16.9007249439881));
#24711=CARTESIAN_POINT('Ctrl Pts',(-1.98754375892155,-0.205305254166047,
16.8938296732041));
#24712=CARTESIAN_POINT('Ctrl Pts',(-1.99334611033523,-0.0760207855470938,
16.8857561467659));
#24713=CARTESIAN_POINT('Ctrl Pts',(-1.99381268095662,-0.0626007560284189,
16.8849143368068));
#24714=CARTESIAN_POINT('Ctrl Pts',(-1.99429969228872,-0.0428524027725935,
16.8836696537673));
#24715=CARTESIAN_POINT('Ctrl Pts',(-1.99442557588602,-0.0365268646384565,
16.8832700817958));
#24716=CARTESIAN_POINT('Ctrl Pts',(-1.99459487867349,-0.0253458037629439,
16.8825621787351));
#24717=CARTESIAN_POINT('Ctrl Pts',(-1.99465066581256,-0.0204904975402112,
16.88225423738));
#24718=CARTESIAN_POINT('Ctrl Pts',(-1.99473016565131,-0.010348079090638,
16.8816098216231));
#24719=CARTESIAN_POINT('Ctrl Pts',(-1.99475058642307,-0.00506098584367161,
16.8812732465272));
#24720=CARTESIAN_POINT('Ctrl Pts',(-1.99474902518492,0.00871386445208958,
16.8803946168026));
#24721=CARTESIAN_POINT('Ctrl Pts',(-1.99469388920883,0.0172014409270973,
16.8798515284149));
#24722=CARTESIAN_POINT('Ctrl Pts',(-1.99421732835034,0.0542043160928534,
16.8774762172676));
#24723=CARTESIAN_POINT('Ctrl Pts',(-1.99323860307682,0.0827078689679757,
16.8756266602739));
#24724=CARTESIAN_POINT('Ctrl Pts',(-1.98905591326439,0.157635832937072,
16.870709647773));
#24725=CARTESIAN_POINT('Ctrl Pts',(-1.98483815122889,0.203983878561712,
16.8676120683846));
#24726=CARTESIAN_POINT('Ctrl Pts',(-1.95455254570461,0.44359184664207,16.8513090825775));
#24727=CARTESIAN_POINT('Ctrl Pts',(-1.90187537957457,0.632378623373003,
16.8373450918898));
#24728=CARTESIAN_POINT('Ctrl Pts',(-1.80804112401136,0.843391916970157,
16.8217536975807));
#24729=CARTESIAN_POINT('Ctrl Pts',(-1.79253047780147,0.875875286437578,
16.8193585417887));
#24730=CARTESIAN_POINT('Ctrl Pts',(-1.77346527155746,0.913172074935447,
16.8166290083371));
#24731=CARTESIAN_POINT('Ctrl Pts',(-1.77075905014548,0.918408784968108,
16.8162462461532));
#24732=CARTESIAN_POINT('Ctrl Pts',(-1.76639736463288,0.92675797233013,16.8156368505928));
#24733=CARTESIAN_POINT('Ctrl Pts',(-1.76475681977809,0.929878140712621,
16.8154093076938));
#24734=CARTESIAN_POINT('Ctrl Pts',(-1.76183875727002,0.935392495029688,
16.8150075307899));
#24735=CARTESIAN_POINT('Ctrl Pts',(-1.76056461578253,0.937788441167372,
16.814833084945));
#24736=CARTESIAN_POINT('Ctrl Pts',(-1.75786828019294,0.94283387406216,16.8144660005724));
#24737=CARTESIAN_POINT('Ctrl Pts',(-1.75644498695282,0.945482740556031,
16.8142734337706));
#24738=CARTESIAN_POINT('Ctrl Pts',(-1.75263145533975,0.952541708355605,
16.8137606450252));
#24739=CARTESIAN_POINT('Ctrl Pts',(-1.7502305430359,0.956946065326368,16.8134410964274));
#24740=CARTESIAN_POINT('Ctrl Pts',(-1.73882755632265,0.977677814769204,
16.811938613708));
#24741=CARTESIAN_POINT('Ctrl Pts',(-1.72961310970501,0.993888188676363,
16.8107686910807));
#24742=CARTESIAN_POINT('Ctrl Pts',(-1.63309981005563,1.15826919894595,16.7989304673217));
#24743=CARTESIAN_POINT('Ctrl Pts',(-1.52720201954448,1.29471042660096,16.789268721702));
#24744=CARTESIAN_POINT('Ctrl Pts',(-1.32679708232649,1.49358806558945,16.7727534125305));
#24745=CARTESIAN_POINT('Ctrl Pts',(-1.24219968321856,1.56465030482708,16.7661753680787));
#24746=CARTESIAN_POINT('Ctrl Pts',(-1.14162358880379,1.63581480788914,16.7584846795465));
#24747=CARTESIAN_POINT('Ctrl Pts',(-1.13100420926848,1.64317496643819,16.7576743612264));
#24748=CARTESIAN_POINT('Ctrl Pts',(-1.11516086709462,1.65392944152406,16.7564675959102));
#24749=CARTESIAN_POINT('Ctrl Pts',(-1.10999115429502,1.65740338873693,16.7560741647671));
#24750=CARTESIAN_POINT('Ctrl Pts',(-1.10077329405929,1.66353514191372,16.7553732166747));
#24751=CARTESIAN_POINT('Ctrl Pts',(-1.09673156066048,1.6662025376495,16.7550660633818));
#24752=CARTESIAN_POINT('Ctrl Pts',(-1.08821620834786,1.67177795059815,16.7544193126021));
#24753=CARTESIAN_POINT('Ctrl Pts',(-1.08374056044535,1.67468278457462,16.7540795993115));
#24754=CARTESIAN_POINT('Ctrl Pts',(-1.07193160259281,1.68227999977469,16.7531838071098));
#24755=CARTESIAN_POINT('Ctrl Pts',(-1.06457919674939,1.68694234879012,16.75262661843));
#24756=CARTESIAN_POINT('Ctrl Pts',(-1.03122235534646,1.7077898595469,16.7501009625148));
#24757=CARTESIAN_POINT('Ctrl Pts',(-1.00487893758587,1.72342214729797,16.748112334381));
#24758=CARTESIAN_POINT('Ctrl Pts',(-0.933475519307544,1.76359947295092,
16.7427346096397));
#24759=CARTESIAN_POINT('Ctrl Pts',(-0.887813403303553,1.78702161455461,
16.7393079382413));
#24760=CARTESIAN_POINT('Ctrl Pts',(-0.749899513418087,1.85117271657148,
16.7289986718655));
#24761=CARTESIAN_POINT('Ctrl Pts',(-0.655412418530284,1.88669577792285,
16.7219791492113));
#24762=CARTESIAN_POINT('Ctrl Pts',(-0.476956327253535,1.93875809696486,
16.7090092913177));
#24763=CARTESIAN_POINT('Ctrl Pts',(-0.393810818413432,1.95734136191275,
16.7030783286534));
#24764=CARTESIAN_POINT('Ctrl Pts',(-0.272842241311096,1.97635493653421,
16.6948015506274));
#24765=CARTESIAN_POINT('Ctrl Pts',(-0.235798083935167,1.98111620808697,
16.69231423842));
#24766=CARTESIAN_POINT('Ctrl Pts',(-0.192708432024769,1.98542855584353,
16.6894919171655));
#24767=CARTESIAN_POINT('Ctrl Pts',(-0.186774830721642,1.98599553245411,
16.6891048287576));
#24768=CARTESIAN_POINT('Ctrl Pts',(-0.177308823081423,1.98685724372613,
16.688489872511));
#24769=CARTESIAN_POINT('Ctrl Pts',(-0.173778075906166,1.98716916906953,
16.6882610692757));
#24770=CARTESIAN_POINT('Ctrl Pts',(-0.167539948455341,1.98770352599418,
16.6878578496154));
#24771=CARTESIAN_POINT('Ctrl Pts',(-0.164832923342684,1.98792984014027,
16.6876832161804));
#24772=CARTESIAN_POINT('Ctrl Pts',(-0.159138273187571,1.98839421512925,
16.6873165765256));
#24773=CARTESIAN_POINT('Ctrl Pts',(-0.156150578533138,1.98863107233771,
16.6871246388226));
#24774=CARTESIAN_POINT('Ctrl Pts',(-0.148205450236327,1.98924292721306,
16.6866153103506));
#24775=CARTESIAN_POINT('Ctrl Pts',(-0.143247089177238,1.98960612978326,
16.6862985770149));
#24776=CARTESIAN_POINT('Ctrl Pts',(-0.120159096986449,1.99121058022812,
16.6848287729036));
#24777=CARTESIAN_POINT('Ctrl Pts',(-0.102013691133315,1.99222263982331,
16.683688036299));
#24778=CARTESIAN_POINT('Ctrl Pts',(0.0721460156645393,1.99955052407448,
16.6728557317881));
#24779=CARTESIAN_POINT('Ctrl Pts',(0.228403099608374,1.98777619380485,16.6640019459702));
#24780=CARTESIAN_POINT('Ctrl Pts',(0.50590133044061,1.93367590241801,16.6475426380116));
#24781=CARTESIAN_POINT('Ctrl Pts',(0.627493249398118,1.89770493173866,16.6400579838682));
#24782=CARTESIAN_POINT('Ctrl Pts',(0.756922220350272,1.84560712280681,16.6313498888973));
#24783=CARTESIAN_POINT('Ctrl Pts',(0.768945850515908,1.84063010015916,16.6305338378908));
#24784=CARTESIAN_POINT('Ctrl Pts',(0.786667694623885,1.83309042886999,16.62932016135));
#24785=CARTESIAN_POINT('Ctrl Pts',(0.792404115428017,1.8306180100148,16.6289256026702));
#24786=CARTESIAN_POINT('Ctrl Pts',(0.802568954494305,1.82618019614825,16.6282233840759));
#24787=CARTESIAN_POINT('Ctrl Pts',(0.807002023284808,1.82422552587605,16.6279160925957));
#24788=CARTESIAN_POINT('Ctrl Pts',(0.816293690844209,1.82008805920375,16.6272698023845));
#24789=CARTESIAN_POINT('Ctrl Pts',(0.821150749369042,1.81790191673574,16.6269306907076));
#24790=CARTESIAN_POINT('Ctrl Pts',(0.833885483514078,1.8121086148904,16.6260381871712));
#24791=CARTESIAN_POINT('Ctrl Pts',(0.841748447561085,1.80846956813637,16.6254837002685));
#24792=CARTESIAN_POINT('Ctrl Pts',(0.876923885565738,1.79191097582611,16.6229875838446));
#24793=CARTESIAN_POINT('Ctrl Pts',(0.903963184978954,1.77842369529033,16.621026366889));
#24794=CARTESIAN_POINT('Ctrl Pts',(0.975216622861375,1.74083744706297,16.6157405050005));
#24795=CARTESIAN_POINT('Ctrl Pts',(1.01883988620459,1.71567101973835,16.6123798458872));
#24796=CARTESIAN_POINT('Ctrl Pts',(1.14616265451037,1.63564877102358,16.6021953620248));
#24797=CARTESIAN_POINT('Ctrl Pts',(1.22673195346038,1.57612218113352,16.5952343024069));
#24798=CARTESIAN_POINT('Ctrl Pts',(1.39582834956368,1.43034194230574,16.5796569751341));
#24799=CARTESIAN_POINT('Ctrl Pts',(1.48152095304375,1.34138658966505,16.571060734088));
#24800=CARTESIAN_POINT('Ctrl Pts',(1.56317761729671,1.23917730211983,16.5625196994939));
#24801=CARTESIAN_POINT('Ctrl Pts',(1.56786016493216,1.23324740297999,16.5620286009859));
#24802=CARTESIAN_POINT('Ctrl Pts',(1.57466290057864,1.22453116238265,16.5613133745241));
#24803=CARTESIAN_POINT('Ctrl Pts',(1.57680955639181,1.22176570644128,16.5610874183815));
#24804=CARTESIAN_POINT('Ctrl Pts',(1.58060518470355,1.21684927501266,16.56068744916));
#24805=CARTESIAN_POINT('Ctrl Pts',(1.58225706517009,1.2147005754837,16.5605132307513));
#24806=CARTESIAN_POINT('Ctrl Pts',(1.58574039489923,1.210150438276,16.5601455454016));
#24807=CARTESIAN_POINT('Ctrl Pts',(1.58757076632006,1.20774821279019,16.5599521543381));
#24808=CARTESIAN_POINT('Ctrl Pts',(1.59246207078364,1.20129840900599,16.5594348301449));
#24809=CARTESIAN_POINT('Ctrl Pts',(1.59551305137694,1.19724325791056,16.559111591451));
#24810=CARTESIAN_POINT('Ctrl Pts',(1.61008247427344,1.17772399069686,16.5575651093825));
#24811=CARTESIAN_POINT('Ctrl Pts',(1.62139224091025,1.16210440161631,16.5563558200972));
#24812=CARTESIAN_POINT('Ctrl Pts',(1.65234311573005,1.11802736188042,16.5530137822637));
#24813=CARTESIAN_POINT('Ctrl Pts',(1.67147423263653,1.08921859010369,16.5509096621664));
#24814=CARTESIAN_POINT('Ctrl Pts',(1.73855751124592,0.982267155972074,16.5433300297437));
#24815=CARTESIAN_POINT('Ctrl Pts',(1.78185931372507,0.901338251149441,16.5380297012983));
#24816=CARTESIAN_POINT('Ctrl Pts',(1.88329840287108,0.675632396680486,16.5236780642973));
#24817=CARTESIAN_POINT('Ctrl Pts',(1.93028262906167,0.526584949104312,16.5146027167588));
#24818=CARTESIAN_POINT('Ctrl Pts',(1.96180648783979,0.361249165216293,16.5040921799395));
#24819=CARTESIAN_POINT('Ctrl Pts',(1.96404452339453,0.348876416062155,16.5033034114031));
#24820=CARTESIAN_POINT('Ctrl Pts',(1.967204507576,0.330411764749167,16.5021226610736));
#24821=CARTESIAN_POINT('Ctrl Pts',(1.96821547469222,0.324335247407431,16.5017335070935));
#24822=CARTESIAN_POINT('Ctrl Pts',(1.96996957076929,0.313481775671792,16.5010373493372));
#24823=CARTESIAN_POINT('Ctrl Pts',(1.97072351406344,0.308706598372016,16.5007306911271));
#24824=CARTESIAN_POINT('Ctrl Pts',(1.97227870383174,0.298618726014456,16.5000820516492));
#24825=CARTESIAN_POINT('Ctrl Pts',(1.97307585824194,0.293305447965371,16.4997399433618));
#24826=CARTESIAN_POINT('Ctrl Pts',(1.97513249277483,0.279209456726481,16.4988310601912));
#24827=CARTESIAN_POINT('Ctrl Pts',(1.97635484610452,0.270421527989015,16.4982631161582));
#24828=CARTESIAN_POINT('Ctrl Pts',(1.98176037521902,0.229563433203964,16.4956162199731));
#24829=CARTESIAN_POINT('Ctrl Pts',(1.98522162593979,0.197404271554775,16.4935146600132));
#24830=CARTESIAN_POINT('Ctrl Pts',(1.99248029288389,0.110046301160344,16.4877528446617));
#24831=CARTESIAN_POINT('Ctrl Pts',(1.99476539556015,0.0547538797841763,
16.4840480770293));
#24832=CARTESIAN_POINT('Ctrl Pts',(1.99472084027156,-0.10451324661133,16.4732187062672));
#24833=CARTESIAN_POINT('Ctrl Pts',(1.98656541957888,-0.208299905003579,
16.4659593160153));
#24834=CARTESIAN_POINT('Ctrl Pts',(1.95915199036361,-0.381997002730529,
16.4536967920309));
#24835=CARTESIAN_POINT('Ctrl Pts',(1.94410890929081,-0.45237156257599,16.4486997142241));
#24836=CARTESIAN_POINT('Ctrl Pts',(1.92459299505438,-0.524382125772988,
16.4436417649834));
#24837=CARTESIAN_POINT('Ctrl Pts',(1.92388351040222,-0.526979173191117,
16.4434594296823));
#24838=CARTESIAN_POINT('Ctrl Pts',(1.91293774660489,-0.566729084893602,
16.4406699224326));
#24839=CARTESIAN_POINT('Ctrl Pts',(1.90163131762015,-0.603582217110363,
16.4381007443645));
#24840=CARTESIAN_POINT('Ctrl Pts',(1.88714598452739,-0.646336701726393,
16.4351583548678));
#24841=CARTESIAN_POINT('Ctrl Pts',(1.88499767986217,-0.652575550262991,
16.4347299615342));
#24842=CARTESIAN_POINT('Ctrl Pts',(1.88169783505153,-0.662006293164019,
16.4340839862395));
#24843=CARTESIAN_POINT('Ctrl Pts',(1.88056906917945,-0.665206021538717,
16.4338650935147));
#24844=CARTESIAN_POINT('Ctrl Pts',(1.87852991603475,-0.670939763930992,
16.4334733689175));
#24845=CARTESIAN_POINT('Ctrl Pts',(1.87762256133708,-0.673474817428733,
16.4333003598805));
#24846=CARTESIAN_POINT('Ctrl Pts',(1.87565131169209,-0.678947331998111,
16.4329272787143));
#24847=CARTESIAN_POINT('Ctrl Pts',(1.87458565187466,-0.681884122702154,
16.4327273138992));
#24848=CARTESIAN_POINT('Ctrl Pts',(1.87160974587897,-0.690025549173345,
16.4321736212907));
#24849=CARTESIAN_POINT('Ctrl Pts',(1.86968467614099,-0.695224793106826,
16.4318207668955));
#24850=CARTESIAN_POINT('Ctrl Pts',(1.85885457118732,-0.724104483546334,
16.4298645832112));
#24851=CARTESIAN_POINT('Ctrl Pts',(1.84952084996295,-0.747623161211341,
16.428285695259));
#24852=CARTESIAN_POINT('Ctrl Pts',(1.77672383453969,-0.921338842276807,
16.416684432423));
#24853=CARTESIAN_POINT('Ctrl Pts',(1.69549817495256,-1.06344406120452,16.4074958847814));
#24854=CARTESIAN_POINT('Ctrl Pts',(1.53109063619255,-1.28344569354573,16.3914373817416));
#24855=CARTESIAN_POINT('Ctrl Pts',(1.45694606875831,-1.36703117385271,16.3847893560265));
#24856=CARTESIAN_POINT('Ctrl Pts',(1.36684771192279,-1.45290131940669,16.377020310384));
#24857=CARTESIAN_POINT('Ctrl Pts',(1.35739682432387,-1.4617348460928,16.3762090142992));
#24858=CARTESIAN_POINT('Ctrl Pts',(1.34326708546068,-1.47468638448044,16.3750010699312));
#24859=CARTESIAN_POINT('Ctrl Pts',(1.33865364862301,-1.47887551979562,16.3746074461707));
#24860=CARTESIAN_POINT('Ctrl Pts',(1.33042006700895,-1.48628175739307,16.3739062812565));
#24861=CARTESIAN_POINT('Ctrl Pts',(1.32680767682032,-1.48950743707856,16.3735991045751));
#24862=CARTESIAN_POINT('Ctrl Pts',(1.31919196574312,-1.4962581904967,16.3729524335373));
#24863=CARTESIAN_POINT('Ctrl Pts',(1.31518618598601,-1.49978042072497,16.3726128238682));
#24864=CARTESIAN_POINT('Ctrl Pts',(1.3046107003509,-1.50900435832209,16.3717175980776));
#24865=CARTESIAN_POINT('Ctrl Pts',(1.2980177976398,-1.51467918251336,16.3711608747291));
#24866=CARTESIAN_POINT('Ctrl Pts',(1.26852136370655,-1.53973415632697,16.3686759776842));
#24867=CARTESIAN_POINT('Ctrl Pts',(1.24522045446381,-1.55863837338692,16.3667285285644));
#24868=CARTESIAN_POINT('Ctrl Pts',(1.18191512173939,-1.60767275111424,16.361474987186));
#24869=CARTESIAN_POINT('Ctrl Pts',(1.14118962099465,-1.63683248155291,16.3581331919109));
#24870=CARTESIAN_POINT('Ctrl Pts',(0.940859195913623,-1.76915779898231,
16.3418771199799));
#24871=CARTESIAN_POINT('Ctrl Pts',(0.768181440041581,-1.85068066275807,
16.3282787648916));
#24872=CARTESIAN_POINT('Ctrl Pts',(0.552643582820447,-1.91699625236617,
16.3130598137048));
#24873=CARTESIAN_POINT('Ctrl Pts',(0.518414043724896,-1.92653492724311,
16.3106961606288));
#24874=CARTESIAN_POINT('Ctrl Pts',(0.478249379526924,-1.936579347296,16.3079984024909));
#24875=CARTESIAN_POINT('Ctrl Pts',(0.47254691662802,-1.93797870242915,16.3076171472811));
#24876=CARTESIAN_POINT('Ctrl Pts',(0.463417600623498,-1.94017629841859,
16.3070096899712));
#24877=CARTESIAN_POINT('Ctrl Pts',(0.459994724238379,-1.94099067376742,
16.3067825872857));
#24878=CARTESIAN_POINT('Ctrl Pts',(0.453929000806524,-1.94241689228135,
16.3063813128865));
#24879=CARTESIAN_POINT('Ctrl Pts',(0.451287040924777,-1.94303240535023,
16.3062069311387));
#24880=CARTESIAN_POINT('Ctrl Pts',(0.445710351368644,-1.9443196518877,16.3058396847283));
#24881=CARTESIAN_POINT('Ctrl Pts',(0.442775361837196,-1.94499012986654,
16.3056468929308));
#24882=CARTESIAN_POINT('Ctrl Pts',(0.435029168150651,-1.9467412515557,16.3051393265999));
#24883=CARTESIAN_POINT('Ctrl Pts',(0.430215417522592,-1.94781071293563,
16.3048251890987));
#24884=CARTESIAN_POINT('Ctrl Pts',(0.408050631234795,-1.95264884271615,
16.3033844350071));
#24885=CARTESIAN_POINT('Ctrl Pts',(0.390653063184677,-1.9562037362078,16.3022695623201));
#24886=CARTESIAN_POINT('Ctrl Pts',(0.204956648586496,-1.99157131492097,
16.2905171868948));
#24887=CARTESIAN_POINT('Ctrl Pts',(0.0332514037991786,-2.00181830485268,
16.2808883729642));
#24888=CARTESIAN_POINT('Ctrl Pts',(-0.249338889014082,-1.98226811197165,
16.264328044652));
#24889=CARTESIAN_POINT('Ctrl Pts',(-0.360141236352017,-1.96515894840319,
16.2576585183495));
#24890=CARTESIAN_POINT('Ctrl Pts',(-0.481493555491101,-1.93580964672997,
16.2498653864549));
#24891=CARTESIAN_POINT('Ctrl Pts',(-0.494041783208733,-1.93264526911354,
16.2490538005373));
#24892=CARTESIAN_POINT('Ctrl Pts',(-0.5125863130384,-1.92777635594111,16.247845506692));
#24893=CARTESIAN_POINT('Ctrl Pts',(-0.518607017057288,-1.9261654049605,
16.2474518258592));
#24894=CARTESIAN_POINT('Ctrl Pts',(-0.529292625670624,-1.92325254051255,
16.2467505966836));
#24895=CARTESIAN_POINT('Ctrl Pts',(-0.53396054535643,-1.92196179813806,
16.2464434130549));
#24896=CARTESIAN_POINT('Ctrl Pts',(-0.543759189451278,-1.91921388957568,
16.2457967655598));
#24897=CARTESIAN_POINT('Ctrl Pts',(-0.548888855698729,-1.91775312103295,
16.2454571865261));
#24898=CARTESIAN_POINT('Ctrl Pts',(-0.562367154549118,-1.91385641555012,
16.2445621281949));
#24899=CARTESIAN_POINT('Ctrl Pts',(-0.570705750864116,-1.91138644387144,
16.2440055424214));
#24900=CARTESIAN_POINT('Ctrl Pts',(-0.604991665118755,-1.90098626950671,
16.2417051015714));
#24901=CARTESIAN_POINT('Ctrl Pts',(-0.630790990500136,-1.89258191824386,
16.2399458025394));
#24902=CARTESIAN_POINT('Ctrl Pts',(-0.69868726747648,-1.86892163983815,
16.235237989733));
#24903=CARTESIAN_POINT('Ctrl Pts',(-0.740453738240495,-1.85277082832396,
16.2322611246372));
#24904=CARTESIAN_POINT('Ctrl Pts',(-0.909452116101657,-1.78079306677736,
16.2198810089001));
#24905=CARTESIAN_POINT('Ctrl Pts',(-1.03121785739565,-1.71315745230085,
16.2101286245708));
#24906=CARTESIAN_POINT('Ctrl Pts',(-1.22072406736468,-1.5803235492986,16.1940397857979));
#24907=CARTESIAN_POINT('Ctrl Pts',(-1.29271860449864,-1.52199632896768,
16.1876793772745));
#24908=CARTESIAN_POINT('Ctrl Pts',(-1.36615419918655,-1.45351709666854,
16.1811204156262));
#24909=CARTESIAN_POINT('Ctrl Pts',(-1.37186663311428,-1.44812678732777,
16.1806097353838));
#24910=CARTESIAN_POINT('Ctrl Pts',(-1.38011943987973,-1.44024669516089,
16.1798714629457));
#24911=CARTESIAN_POINT('Ctrl Pts',(-1.38268513607195,-1.43778372025244,
16.1796418738949));
#24912=CARTESIAN_POINT('Ctrl Pts',(-1.38720015235866,-1.43342620619791,
16.1792377517232));
#24913=CARTESIAN_POINT('Ctrl Pts',(-1.38915220363405,-1.43153452868563,
16.1790629983688));
#24914=CARTESIAN_POINT('Ctrl Pts',(-1.393244066615,-1.42755296904277,16.1786966220437));
#24915=CARTESIAN_POINT('Ctrl Pts',(-1.39538304170685,-1.42546226740192,
16.1785050656263));
#24916=CARTESIAN_POINT('Ctrl Pts',(-1.39973271281647,-1.42119158962664,
16.1781154329696));
#24917=CARTESIAN_POINT('Ctrl Pts',(-1.40194303892925,-1.41901124649057,
16.1779173861771));
#24918=CARTESIAN_POINT('Ctrl Pts',(-1.41135220939285,-1.40968626725036,
16.1770740501836));
#24919=CARTESIAN_POINT('Ctrl Pts',(-1.41850176033607,-1.40249178154965,
16.1764325710668));
#24920=CARTESIAN_POINT('Ctrl Pts',(-1.47692330683751,-1.34279927855359,
16.171182004695));
#24921=CARTESIAN_POINT('Ctrl Pts',(-1.52532375702421,-1.28755674990014,
16.1667748554819));
#24922=CARTESIAN_POINT('Ctrl Pts',(-1.60653714581684,-1.18383647792672,
16.1590105881081));
#24923=CARTESIAN_POINT('Ctrl Pts',(-1.64046912714042,-1.13635023349188,
16.155627454503));
#24924=CARTESIAN_POINT('Ctrl Pts',(-1.75326817084982,-0.962887791352267,
16.1436270980803));
#24925=CARTESIAN_POINT('Ctrl Pts',(-1.82008480465106,-0.829690516503707,
16.1350066792169));
#24926=CARTESIAN_POINT('Ctrl Pts',(-1.87616581456879,-0.677651586910031,
16.1249820646661));
#24927=CARTESIAN_POINT('Ctrl Pts',(-1.88070923261675,-0.664938046384692,
16.1241428609167));
#24928=CARTESIAN_POINT('Ctrl Pts',(-1.88906350256649,-0.640790054421439,
16.1225465352056));
#24929=CARTESIAN_POINT('Ctrl Pts',(-1.89290047274669,-0.629365236313066,
16.1217903017965));
#24930=CARTESIAN_POINT('Ctrl Pts',(-1.89853488634873,-0.612070682169828,
16.1206437757707));
#24931=CARTESIAN_POINT('Ctrl Pts',(-1.90040919696285,-0.606226127270713,
16.1202560150732));
#24932=CARTESIAN_POINT('Ctrl Pts',(-1.90371075307071,-0.595765287401171,
16.1195614071961));
#24933=CARTESIAN_POINT('Ctrl Pts',(-1.90514826186818,-0.591152271971093,
16.1192548996995));
#24934=CARTESIAN_POINT('Ctrl Pts',(-1.90815252441948,-0.581386712413458,
16.1186055937766));
#24935=CARTESIAN_POINT('Ctrl Pts',(-1.90971519795699,-0.576232962935452,
16.1182626645406));
#24936=CARTESIAN_POINT('Ctrl Pts',(-1.91381341614365,-0.5625171188833,16.1173492931216));
#24937=CARTESIAN_POINT('Ctrl Pts',(-1.91631234757277,-0.553944296014019,
16.1167776611458));
#24938=CARTESIAN_POINT('Ctrl Pts',(-1.92164650677388,-0.535176822822759,
16.1155245166883));
#24939=CARTESIAN_POINT('Ctrl Pts',(-1.92445833166587,-0.524975857713881,
16.1148422612552));
#24940=CARTESIAN_POINT('Ctrl Pts',(-1.9325869588191,-0.494543020349167,
16.1128033552907));
#24941=CARTESIAN_POINT('Ctrl Pts',(-1.93766667681076,-0.474249878078136,
16.1114391585396));
#24942=CARTESIAN_POINT('Ctrl Pts',(-1.97733363940674,-0.304491487802693,
16.0999861661938));
#24943=CARTESIAN_POINT('Ctrl Pts',(-1.99488318252704,-0.151604532131688,
16.0893478098941));
#24944=CARTESIAN_POINT('Ctrl Pts',(-1.99474923905823,0.00174234801668578,
16.07864965537));
#24945=CARTESIAN_POINT('',(-1.99474965194692,-0.00117837076332067,14.4790451186048));
#24946=CARTESIAN_POINT('Ctrl Pts',(-1.9947492380933,0.00174345238502811,
16.0786495783244));
#24947=CARTESIAN_POINT('Ctrl Pts',(-1.9946527896329,0.11209375190194,16.0709510549627));
#24948=CARTESIAN_POINT('Ctrl Pts',(-1.98539954860549,0.222261577203071,
16.0632697882811));
#24949=CARTESIAN_POINT('Ctrl Pts',(-1.9655023144666,0.340467667316,16.0553715701984));
#24950=CARTESIAN_POINT('Ctrl Pts',(-1.96386065344918,0.349812696704146,
16.0547496030639));
#24951=CARTESIAN_POINT('Ctrl Pts',(-1.96129914989705,0.363807178115647,
16.05382221121));
#24952=CARTESIAN_POINT('Ctrl Pts',(-1.96042934144709,0.368465488915019,
16.0535141827204));
#24953=CARTESIAN_POINT('Ctrl Pts',(-1.95895289923287,0.376219418966858,
16.0530026250845));
#24954=CARTESIAN_POINT('Ctrl Pts',(-1.95835551364941,0.379316747734227,
16.0527985926566));
#24955=CARTESIAN_POINT('Ctrl Pts',(-1.95717074648686,0.385382129463518,
16.0523996700488));
#24956=CARTESIAN_POINT('Ctrl Pts',(-1.95658395450499,0.388350287610403,
16.0522047473525));
#24957=CARTESIAN_POINT('Ctrl Pts',(-1.9554589819207,0.393973439400101,16.05183604079));
#24958=CARTESIAN_POINT('Ctrl Pts',(-1.95492215286741,0.396628638958936,
16.051662185347));
#24959=CARTESIAN_POINT('Ctrl Pts',(-1.95368115633524,0.402702977214842,
16.0512650019972));
#24960=CARTESIAN_POINT('Ctrl Pts',(-1.9529734222032,0.406121362524119,16.0510418803883));
#24961=CARTESIAN_POINT('Ctrl Pts',(-1.95107042847056,0.41519288496285,16.0504507838302));
#24962=CARTESIAN_POINT('Ctrl Pts',(-1.94985956284539,0.420842768420181,
16.0500836838035));
#24963=CARTESIAN_POINT('Ctrl Pts',(-1.94141985332776,0.459403865390753,
16.0475848259531));
#24964=CARTESIAN_POINT('Ctrl Pts',(-1.93338214728715,0.492134896974623,
16.0454968477282));
#24965=CARTESIAN_POINT('Ctrl Pts',(-1.90440331593729,0.598435132671208,
16.0387775753409));
#24966=CARTESIAN_POINT('Ctrl Pts',(-1.88005956466325,0.671010158128769,
16.0342867013603));
#24967=CARTESIAN_POINT('Ctrl Pts',(-1.83717276310179,0.778029089459532,
16.0275748916603));
#24968=CARTESIAN_POINT('Ctrl Pts',(-1.82169186239954,0.813616508858517,
16.0253276451676));
#24969=CARTESIAN_POINT('Ctrl Pts',(-1.79087764297408,0.879155964903707,
16.021126216155));
#24970=CARTESIAN_POINT('Ctrl Pts',(-1.77580566660233,0.909215117337312,
16.019173682129));
#24971=CARTESIAN_POINT('Ctrl Pts',(-1.71656009196387,1.02027431471765,16.0118236242065));
#24972=CARTESIAN_POINT('Ctrl Pts',(-1.66754930610852,1.09855121425934,16.0063595150894));
#24973=CARTESIAN_POINT('Ctrl Pts',(-1.59534772278531,1.19784189395358,15.9988244739383));
#24974=CARTESIAN_POINT('Ctrl Pts',(-1.5768296120453,1.22211610589529,15.9969308793983));
#24975=CARTESIAN_POINT('Ctrl Pts',(-1.55228919322179,1.25279791189754,15.9944654766801));
#24976=CARTESIAN_POINT('Ctrl Pts',(-1.54677090018576,1.25960474984806,15.9939138364973));
#24977=CARTESIAN_POINT('Ctrl Pts',(-1.53781261269245,1.2705071960211,15.993022588298));
#24978=CARTESIAN_POINT('Ctrl Pts',(-1.534400640192,1.27462576522166,15.992684116532));
#24979=CARTESIAN_POINT('Ctrl Pts',(-1.52786973029459,1.28244495861365,15.9920380752596));
#24980=CARTESIAN_POINT('Ctrl Pts',(-1.5247538032281,1.28614805659659,15.9917306300986));
#24981=CARTESIAN_POINT('Ctrl Pts',(-1.51761242078122,1.29457274822584,15.9910277573812));
#24982=CARTESIAN_POINT('Ctrl Pts',(-1.51357836523474,1.29928695483865,15.9906319775548));
#24983=CARTESIAN_POINT('Ctrl Pts',(-1.50115565219921,1.31366779802462,15.98941697728));
#24984=CARTESIAN_POINT('Ctrl Pts',(-1.49269602799819,1.32327243264591,15.9885948178463));
#24985=CARTESIAN_POINT('Ctrl Pts',(-1.38641376929217,1.44162392391303,15.9783282797106));
#24986=CARTESIAN_POINT('Ctrl Pts',(-1.27703009480913,1.53935057847327,15.9683627390451));
#24987=CARTESIAN_POINT('Ctrl Pts',(-1.0719773452698,1.68554050706017,15.9508342938042));
#24988=CARTESIAN_POINT('Ctrl Pts',(-0.981243680039204,1.73992661279771,
15.9434139653585));
#24989=CARTESIAN_POINT('Ctrl Pts',(-0.858568647998133,1.80079665636824,
15.9340969595623));
#24990=CARTESIAN_POINT('Ctrl Pts',(-0.830183715831587,1.81405731706274,
15.9319885889391));
#24991=CARTESIAN_POINT('Ctrl Pts',(-0.785101274697649,1.83383862768064,
15.9287263239504));
#24992=CARTESIAN_POINT('Ctrl Pts',(-0.768609077783679,1.84081184928874,
15.9275506864571));
#24993=CARTESIAN_POINT('Ctrl Pts',(-0.747450918990749,1.84942398324726,
15.9260670172339));
#24994=CARTESIAN_POINT('Ctrl Pts',(-0.74287034719889,1.85126864464043,15.9257472721007));
#24995=CARTESIAN_POINT('Ctrl Pts',(-0.735484679104377,1.85421113206303,
15.92523411598));
#24996=CARTESIAN_POINT('Ctrl Pts',(-0.732683900219955,1.8553196323324,15.9250400712032));
#24997=CARTESIAN_POINT('Ctrl Pts',(-0.727356374601661,1.85741423044616,
15.9246720326447));
#24998=CARTESIAN_POINT('Ctrl Pts',(-0.72483015885912,1.85840150667947,15.924497971473));
#24999=CARTESIAN_POINT('Ctrl Pts',(-0.719025013418015,1.86065659134515,
15.9240990200988));
#25000=CARTESIAN_POINT('Ctrl Pts',(-0.715744743324225,1.86192088545769,
15.9238743426542));
#25001=CARTESIAN_POINT('Ctrl Pts',(-0.706986211038732,1.86527006555698,
15.9232764076172));
#25002=CARTESIAN_POINT('Ctrl Pts',(-0.701502021424044,1.86733950744365,
15.922904057475));
#25003=CARTESIAN_POINT('Ctrl Pts',(-0.662903884023204,1.88171035290446,
15.9202972708386));
#25004=CARTESIAN_POINT('Ctrl Pts',(-0.629474994211099,1.89315530668457,
15.9181110025674));
#25005=CARTESIAN_POINT('Ctrl Pts',(-0.553101616402828,1.91705604216219,
15.9132389124869));
#25006=CARTESIAN_POINT('Ctrl Pts',(-0.510006666211071,1.92896836226965,
15.9105756461925));
#25007=CARTESIAN_POINT('Ctrl Pts',(-0.318539430504791,1.97502750518257,
15.8989755521283));
#25008=CARTESIAN_POINT('Ctrl Pts',(-0.166947111196137,1.99357250333605,
15.8903578065403));
#25009=CARTESIAN_POINT('Ctrl Pts',(0.0308947069436403,1.99503224802059,
15.8785432503216));
#25010=CARTESIAN_POINT('Ctrl Pts',(0.076502358957742,1.99380417752586,15.8757843444004));
#25011=CARTESIAN_POINT('Ctrl Pts',(0.149566215485059,1.9893262291711,15.8712818122131));
#25012=CARTESIAN_POINT('Ctrl Pts',(0.177067746360322,1.98706713395893,15.8695682414089));
#25013=CARTESIAN_POINT('Ctrl Pts',(0.213168027956534,1.98334633067129,15.8672907144756));
#25014=CARTESIAN_POINT('Ctrl Pts',(0.221817456240314,1.98239761091768,15.8667429017418));
#25015=CARTESIAN_POINT('Ctrl Pts',(0.235759212858958,1.98077601320342,15.8658563544656));
#25016=CARTESIAN_POINT('Ctrl Pts',(0.241055597976108,1.98013843422936,15.8655187343998));
#25017=CARTESIAN_POINT('Ctrl Pts',(0.251155104954563,1.97888153486538,15.8648733339777));
#25018=CARTESIAN_POINT('Ctrl Pts',(0.255958660534206,1.97826595259428,15.8645656737954));
#25019=CARTESIAN_POINT('Ctrl Pts',(0.266936986544989,1.97681841037125,15.8638609221095));
#25020=CARTESIAN_POINT('Ctrl Pts',(0.273110172181634,1.97597500357755,15.863463471495));
#25021=CARTESIAN_POINT('Ctrl Pts',(0.292082868441552,1.97329226695444,15.8622383059418));
#25022=CARTESIAN_POINT('Ctrl Pts',(0.30486832411298,1.97135741678673,15.8614075799533));
#25023=CARTESIAN_POINT('Ctrl Pts',(0.427356031565815,1.95160102150611,15.8533986795703));
#25024=CARTESIAN_POINT('Ctrl Pts',(0.535387807585934,1.92476804107169,15.8459298438467));
#25025=CARTESIAN_POINT('Ctrl Pts',(0.803614244301825,1.83380972905258,15.8264073746937));
#25026=CARTESIAN_POINT('Ctrl Pts',(0.958776542691533,1.75766969616028,15.8141277909881));
#25027=CARTESIAN_POINT('Ctrl Pts',(1.11705388713816,1.65273535286599,15.8015462129111));
#25028=CARTESIAN_POINT('Ctrl Pts',(1.1317379193471,1.64271509069432,15.8003791619288));
#25029=CARTESIAN_POINT('Ctrl Pts',(1.15031234244297,1.62967275051754,15.7989051495937));
#25030=CARTESIAN_POINT('Ctrl Pts',(1.15432761621008,1.62683112665772,15.7985866448457));
#25031=CARTESIAN_POINT('Ctrl Pts',(1.16078112047955,1.62222803568393,15.7980750051395));
#25032=CARTESIAN_POINT('Ctrl Pts',(1.16322591832389,1.62047587845511,15.7978812429672));
#25033=CARTESIAN_POINT('Ctrl Pts',(1.16786870923725,1.61713252498481,15.7975134150538));
#25034=CARTESIAN_POINT('Ctrl Pts',(1.17006739149406,1.61554239338464,15.7973392832791));
#25035=CARTESIAN_POINT('Ctrl Pts',(1.17511379968564,1.61187702262572,15.7969397430485));
#25036=CARTESIAN_POINT('Ctrl Pts',(1.1779592742476,1.60979872249933,15.7967145494943));
#25037=CARTESIAN_POINT('Ctrl Pts',(1.18698659570309,1.60316852465207,15.7960003584327));
#25038=CARTESIAN_POINT('Ctrl Pts',(1.19314777312266,1.59858840634351,15.7955132792673));
#25039=CARTESIAN_POINT('Ctrl Pts',(1.29240348122505,1.52390981996341,15.7876695668171));
#25040=CARTESIAN_POINT('Ctrl Pts',(1.37922156662505,1.44580929534614,15.7808460090613));
#25041=CARTESIAN_POINT('Ctrl Pts',(1.52592618006905,1.28851930502849,15.7683474311591));
#25042=CARTESIAN_POINT('Ctrl Pts',(1.58769000148148,1.21159908831075,15.7626743779119));
#25043=CARTESIAN_POINT('Ctrl Pts',(1.67506154760631,1.0845712865334,15.7535434302963));
#25044=CARTESIAN_POINT('Ctrl Pts',(1.70467098150482,1.03741127910021,15.7502011343208));
#25045=CARTESIAN_POINT('Ctrl Pts',(1.74837606466245,0.960866295521648,15.7447994784433));
#25046=CARTESIAN_POINT('Ctrl Pts',(1.76379158248398,0.932267110694594,15.7427863680743));
#25047=CARTESIAN_POINT('Ctrl Pts',(1.78252529368759,0.895382657920932,15.7401908720983));
#25048=CARTESIAN_POINT('Ctrl Pts',(1.78649628533786,0.887433121480815,15.7396315326831));
#25049=CARTESIAN_POINT('Ctrl Pts',(1.79278409236191,0.874632299828052,15.7387308269601));
#25050=CARTESIAN_POINT('Ctrl Pts',(1.79513467342641,0.869797657543339,15.7383906412148));
#25051=CARTESIAN_POINT('Ctrl Pts',(1.79956164346505,0.86059794262176,15.7377432738338));
#25052=CARTESIAN_POINT('Ctrl Pts',(1.80164176844044,0.856234702059272,15.7374362248336));
#25053=CARTESIAN_POINT('Ctrl Pts',(1.80633437719127,0.846298741859406,15.7367369565868));
#25054=CARTESIAN_POINT('Ctrl Pts',(1.80893695998885,0.840721425966304,15.73634439824));
#25055=CARTESIAN_POINT('Ctrl Pts',(1.8167664242427,0.823738268821107,15.7351488640905));
#25056=CARTESIAN_POINT('Ctrl Pts',(1.82191146607867,0.812295250257209,15.7343430848305));
#25057=CARTESIAN_POINT('Ctrl Pts',(1.88989435921471,0.657199727624472,15.7234167719473));
#25058=CARTESIAN_POINT('Ctrl Pts',(1.93567601962903,0.506705313167106,15.7126902034601));
#25059=CARTESIAN_POINT('Ctrl Pts',(1.97945196496466,0.262839467641361,15.6954194193815));
#25060=CARTESIAN_POINT('Ctrl Pts',(1.98938424300913,0.172238990371814,15.6890421884122));
#25061=CARTESIAN_POINT('Ctrl Pts',(1.99449324686085,0.0469503072085415,
15.6804862282634));
#25062=CARTESIAN_POINT('Ctrl Pts',(1.99500609791161,0.0125938935330608,
15.6781678503751));
#25063=CARTESIAN_POINT('Ctrl Pts',(1.99442191280116,-0.0409538870161705,
15.6746141948049));
#25064=CARTESIAN_POINT('Ctrl Pts',(1.99393549374277,-0.0601440042439693,
15.6733526450537));
#25065=CARTESIAN_POINT('Ctrl Pts',(1.99297063706869,-0.0843876386238216,
15.6717765113325));
#25066=CARTESIAN_POINT('Ctrl Pts',(1.99274986015056,-0.0894495947839769,
15.6714483947513));
#25067=CARTESIAN_POINT('Ctrl Pts',(1.99236679001827,-0.0975256202009443,
15.6709265169602));
#25068=CARTESIAN_POINT('Ctrl Pts',(1.99221694051022,-0.100540214864414,
15.6707320703219));
#25069=CARTESIAN_POINT('Ctrl Pts',(1.99191952422333,-0.106261562206286,
15.6703637285011));
#25070=CARTESIAN_POINT('Ctrl Pts',(1.99177328422832,-0.108968320642123,
15.6701897640073));
#25071=CARTESIAN_POINT('Ctrl Pts',(1.99142535289544,-0.115173367869909,
15.6697916332221));
#25072=CARTESIAN_POINT('Ctrl Pts',(1.99121996124137,-0.118671425514473,
15.6695676766948));
#25073=CARTESIAN_POINT('Ctrl Pts',(1.99054155550235,-0.129727503069359,
15.6688613215636));
#25074=CARTESIAN_POINT('Ctrl Pts',(1.99003471233042,-0.137283492685096,
15.6683807822093));
#25075=CARTESIAN_POINT('Ctrl Pts',(1.98056400084957,-0.267373832261972,
15.6601425066931));
#25076=CARTESIAN_POINT('Ctrl Pts',(1.96033950833219,-0.388846396194774,
15.6529781055579));
#25077=CARTESIAN_POINT('Ctrl Pts',(1.90357408724273,-0.604531993860171,
15.640030409639));
#25078=CARTESIAN_POINT('Ctrl Pts',(1.87083552266274,-0.699304305055512,
15.6342550555598));
#25079=CARTESIAN_POINT('Ctrl Pts',(1.80095385045338,-0.861032883307637,
15.6237783634448));
#25080=CARTESIAN_POINT('Ctrl Pts',(1.76682041958583,-0.929061847995357,
15.6191632092025));
#25081=CARTESIAN_POINT('Ctrl Pts',(1.72324031379163,-1.00478787356553,15.6136991452631));
#25082=CARTESIAN_POINT('Ctrl Pts',(1.7175073480908,-1.01455623340083,15.6129878679163));
#25083=CARTESIAN_POINT('Ctrl Pts',(1.70865903278578,-1.02934287345655,15.6119011188232));
#25084=CARTESIAN_POINT('Ctrl Pts',(1.70560400508463,-1.03439712783591,15.6115278465016));
#25085=CARTESIAN_POINT('Ctrl Pts',(1.70026028019183,-1.04314977729231,15.6108782548688));
#25086=CARTESIAN_POINT('Ctrl Pts',(1.69798183714066,-1.04685441132577,15.6106023133194));
#25087=CARTESIAN_POINT('Ctrl Pts',(1.69321261452415,-1.05455239570988,15.6100268316828));
#25088=CARTESIAN_POINT('Ctrl Pts',(1.69071978357449,-1.05854443746359,15.6097272170927));
#25089=CARTESIAN_POINT('Ctrl Pts',(1.683830829649,-1.06949005500667,15.6089024440314));
#25090=CARTESIAN_POINT('Ctrl Pts',(1.67940581963778,-1.07642525529635,15.6083762170346));
#25091=CARTESIAN_POINT('Ctrl Pts',(1.66382617558005,-1.10051290341008,15.606535597904));
#25092=CARTESIAN_POINT('Ctrl Pts',(1.6524509506281,-1.11752046827208,15.6052129933034));
#25093=CARTESIAN_POINT('Ctrl Pts',(1.55330359300697,-1.26093536098684,15.593858476359));
#25094=CARTESIAN_POINT('Ctrl Pts',(1.45145305901874,-1.37694444188002,15.5832591368896));
#25095=CARTESIAN_POINT('Ctrl Pts',(1.24285062431285,-1.56542559607305,15.5636462757614));
#25096=CARTESIAN_POINT('Ctrl Pts',(1.14042526210469,-1.64154573577819,15.5547373637761));
#25097=CARTESIAN_POINT('Ctrl Pts',(1.02307456070021,-1.71243725620804,15.545753233086));
#25098=CARTESIAN_POINT('Ctrl Pts',(1.01467932594733,-1.71742504584792,15.545116898694));
#25099=CARTESIAN_POINT('Ctrl Pts',(1.00285609771061,-1.72433251957279,15.5442300170998));
#25100=CARTESIAN_POINT('Ctrl Pts',(0.999458716866094,-1.72630393172737,
15.5439762401445));
#25101=CARTESIAN_POINT('Ctrl Pts',(0.993654372562984,-1.72964916408859,
15.5435445137915));
#25102=CARTESIAN_POINT('Ctrl Pts',(0.991250339306147,-1.73102802060276,
15.5433662399579));
#25103=CARTESIAN_POINT('Ctrl Pts',(0.986644401699797,-1.73365705899902,
15.543025720391));
#25104=CARTESIAN_POINT('Ctrl Pts',(0.984442988645295,-1.73490805978474,
15.5428634204495));
#25105=CARTESIAN_POINT('Ctrl Pts',(0.979224792440551,-1.73786028303442,
15.5424797612027));
#25106=CARTESIAN_POINT('Ctrl Pts',(0.976205936405182,-1.73955785406685,
15.5422586367755));
#25107=CARTESIAN_POINT('Ctrl Pts',(0.967182060644392,-1.74460129501744,
15.5416000910584));
#25108=CARTESIAN_POINT('Ctrl Pts',(0.961164074127508,-1.74792403808091,
15.5411641158733));
#25109=CARTESIAN_POINT('Ctrl Pts',(0.850582025185871,-1.80823649187624,
15.5332092985703));
#25110=CARTESIAN_POINT('Ctrl Pts',(0.741120812905381,-1.85579044322479,
15.5262479098748));
#25111=CARTESIAN_POINT('Ctrl Pts',(0.5318166317685,-1.92522196653055,15.5134390977038));
#25112=CARTESIAN_POINT('Ctrl Pts',(0.433286066257205,-1.94976169912284,
15.5075974330694));
#25113=CARTESIAN_POINT('Ctrl Pts',(0.281950476477381,-1.97541040930895,
15.4984816239273));
#25114=CARTESIAN_POINT('Ctrl Pts',(0.230261369932737,-1.98210025667364,
15.4953451779851));
#25115=CARTESIAN_POINT('Ctrl Pts',(0.147521013839934,-1.98952873710777,
15.4902478548551));
#25116=CARTESIAN_POINT('Ctrl Pts',(0.11661067700174,-1.99157948136775,15.4883268147675));
#25117=CARTESIAN_POINT('Ctrl Pts',(0.0769340281574682,-1.99328500543427,
15.4858346912803));
#25118=CARTESIAN_POINT('Ctrl Pts',(0.0681994057471645,-1.99360296817505,
15.4852844400508));
#25119=CARTESIAN_POINT('Ctrl Pts',(0.054122111901267,-1.99402279597857,
15.484394897841));
#25120=CARTESIAN_POINT('Ctrl Pts',(0.0487805619729641,-1.99416061784053,
15.4840567351901));
#25121=CARTESIAN_POINT('Ctrl Pts',(0.0385989265556293,-1.99438239026013,
15.4834109279476));
#25122=CARTESIAN_POINT('Ctrl Pts',(0.0337589560308472,-1.99447018727277,
15.4831034061917));
#25123=CARTESIAN_POINT('Ctrl Pts',(0.0227054358960415,-1.99463045175091,
15.4823998585181));
#25124=CARTESIAN_POINT('Ctrl Pts',(0.0164917950282941,-1.99469150374779,
15.4820034778714));
#25125=CARTESIAN_POINT('Ctrl Pts',(-0.00256814825675998,-1.99478971215964,
15.4807848276505));
#25126=CARTESIAN_POINT('Ctrl Pts',(-0.0154144068904503,-1.99473180511758,
15.4799595933177));
#25127=CARTESIAN_POINT('Ctrl Pts',(-0.172186242844886,-1.99251064736297,
15.4698397636446));
#25128=CARTESIAN_POINT('Ctrl Pts',(-0.315439739389119,-1.97489966395824,
15.4600417566724));
#25129=CARTESIAN_POINT('Ctrl Pts',(-0.552153552281778,-1.91937618556936,
15.443125276818));
#25130=CARTESIAN_POINT('Ctrl Pts',(-0.646958137923274,-1.88953026217246,
15.4361545250006));
#25131=CARTESIAN_POINT('Ctrl Pts',(-0.773694013565491,-1.83896939126179,
15.4268206040582));
#25132=CARTESIAN_POINT('Ctrl Pts',(-0.807849099097985,-1.82422340795237,
15.4243045975179));
#25133=CARTESIAN_POINT('Ctrl Pts',(-0.859980016618908,-1.79996502099589,
15.4204840902258));
#25134=CARTESIAN_POINT('Ctrl Pts',(-0.878255171450998,-1.79111910233697,
15.4191486291234));
#25135=CARTESIAN_POINT('Ctrl Pts',(-0.901006263085567,-1.77967467376247,
15.417493875022));
#25136=CARTESIAN_POINT('Ctrl Pts',(-0.905610618276656,-1.77733610779197,
15.4171593917827));
#25137=CARTESIAN_POINT('Ctrl Pts',(-0.912910986896972,-1.77359249384027,
15.4166297634478));
#25138=CARTESIAN_POINT('Ctrl Pts',(-0.915612919647041,-1.77219913832591,
15.4164338976519));
#25139=CARTESIAN_POINT('Ctrl Pts',(-0.920713598177809,-1.76955399843327,
15.4160644517662));
#25140=CARTESIAN_POINT('Ctrl Pts',(-0.923112952984117,-1.7683035258027,
15.4158907956441));
#25141=CARTESIAN_POINT('Ctrl Pts',(-0.928579806906484,-1.76544020435438,
15.4154954140523));
#25142=CARTESIAN_POINT('Ctrl Pts',(-0.931645647368408,-1.76382424326482,
15.4152738882577));
#25143=CARTESIAN_POINT('Ctrl Pts',(-0.939736486170129,-1.75953269589332,
15.414689779883));
#25144=CARTESIAN_POINT('Ctrl Pts',(-0.944754313838724,-1.75684355015778,
15.4143280395755));
#25145=CARTESIAN_POINT('Ctrl Pts',(-0.977997018819345,-1.73884456492324,
15.411934509218));
#25146=CARTESIAN_POINT('Ctrl Pts',(-1.00586211039976,-1.72287558727561,
15.4099424259101));
#25147=CARTESIAN_POINT('Ctrl Pts',(-1.04233473098311,-1.70078707165599,
15.407337654787));
#25148=CARTESIAN_POINT('Ctrl Pts',(-1.05129497982961,-1.69526317363566,
15.4066979594962));
#25149=CARTESIAN_POINT('Ctrl Pts',(-1.2148860731785,-1.59261515995388,15.3950149053074));
#25150=CARTESIAN_POINT('Ctrl Pts',(-1.35551254325261,-1.47477798037274,
15.3848314364103));
#25151=CARTESIAN_POINT('Ctrl Pts',(-1.51202120881655,-1.30206133511899,
15.3709704128747));
#25152=CARTESIAN_POINT('Ctrl Pts',(-1.54445932552945,-1.26341468593201,
15.3679303989625));
#25153=CARTESIAN_POINT('Ctrl Pts',(-1.59395470238153,-1.19968800996751,
15.3629763063732));
#25154=CARTESIAN_POINT('Ctrl Pts',(-1.61196617601303,-1.17537560299963,
15.3610992434239));
#25155=CARTESIAN_POINT('Ctrl Pts',(-1.63441739605989,-1.14358317535177,
15.3586566059735));
#25156=CARTESIAN_POINT('Ctrl Pts',(-1.63937145067098,-1.13646994962209,
15.3581108469893));
#25157=CARTESIAN_POINT('Ctrl Pts',(-1.64729497341312,-1.12493342618513,
15.3572268219234));
#25158=CARTESIAN_POINT('Ctrl Pts',(-1.65029339674597,-1.12053007391104,
15.3568896587039));
#25159=CARTESIAN_POINT('Ctrl Pts',(-1.65598483837359,-1.11209947772614,
15.3562445968015));
#25160=CARTESIAN_POINT('Ctrl Pts',(-1.65868089840397,-1.10807432506637,
15.3559368160397));
#25161=CARTESIAN_POINT('Ctrl Pts',(-1.66481855884391,-1.09883835289982,
15.3552310310868));
#25162=CARTESIAN_POINT('Ctrl Pts',(-1.66825039304214,-1.09362113381343,
15.354832664029));
#25163=CARTESIAN_POINT('Ctrl Pts',(-1.67875281166043,-1.07749044385639,
15.3536019022532));
#25164=CARTESIAN_POINT('Ctrl Pts',(-1.68574110892564,-1.06652405487339,
15.3527664564327));
#25165=CARTESIAN_POINT('Ctrl Pts',(-1.75653313051831,-0.952999470751862,
15.3441295571548));
#25166=CARTESIAN_POINT('Ctrl Pts',(-1.81099189664738,-0.844935107726615,
15.335981802361));
#25167=CARTESIAN_POINT('Ctrl Pts',(-1.89669597090157,-0.627894553412535,
15.3198424509148));
#25168=CARTESIAN_POINT('Ctrl Pts',(-1.92910947416793,-0.519849367004161,
15.3119103611211));
#25169=CARTESIAN_POINT('Ctrl Pts',(-1.96124541729301,-0.36670096513606,
15.3011502115146));
#25170=CARTESIAN_POINT('Ctrl Pts',(-1.96883818353093,-0.3234655111744,15.2981662913259));
#25171=CARTESIAN_POINT('Ctrl Pts',(-1.97819466860347,-0.257471726116805,
15.2937253378715));
#25172=CARTESIAN_POINT('Ctrl Pts',(-1.98100445068317,-0.234877229678068,
15.2922249591443));
#25173=CARTESIAN_POINT('Ctrl Pts',(-1.98399751581249,-0.206906205373042,
15.2903963344348));
#25174=CARTESIAN_POINT('Ctrl Pts',(-1.98454659748363,-0.201571636406673,
15.2900488737199));
#25175=CARTESIAN_POINT('Ctrl Pts',(-1.98537756917351,-0.193165685632635,
15.2895034625662));
#25176=CARTESIAN_POINT('Ctrl Pts',(-1.98567385550802,-0.190095802563266,
15.2893047173156));
#25177=CARTESIAN_POINT('Ctrl Pts',(-1.98621595254572,-0.184339441594563,
15.2889328904975));
#25178=CARTESIAN_POINT('Ctrl Pts',(-1.98646343059267,-0.181653183033562,
15.2887597195322));
#25179=CARTESIAN_POINT('Ctrl Pts',(-1.98701509900995,-0.175529112936757,
15.2883657069906));
#25180=CARTESIAN_POINT('Ctrl Pts',(-1.98731581682795,-0.172091016053264,
15.2881450628195));
#25181=CARTESIAN_POINT('Ctrl Pts',(-1.98820843730845,-0.161571259667954,
15.2874716013178));
#25182=CARTESIAN_POINT('Ctrl Pts',(-1.98877142973061,-0.15448710653519,
15.2870203788304));
#25183=CARTESIAN_POINT('Ctrl Pts',(-1.9929020221701,-0.0987410066511232,
15.2834866400716));
#25184=CARTESIAN_POINT('Ctrl Pts',(-1.99472128907784,-0.0499613959230888,
15.2804961767506));
#25185=CARTESIAN_POINT('Ctrl Pts',(-1.99480080939928,0.0868098812329685,
15.2722742076292));
#25186=CARTESIAN_POINT('Ctrl Pts',(-1.98903262433188,0.174692790294786,
15.2671769599265));
#25187=CARTESIAN_POINT('Ctrl Pts',(-1.9580319883537,0.408752153297152,15.2534837481734));
#25188=CARTESIAN_POINT('Ctrl Pts',(-1.9222926283037,0.552948031636237,15.2448875832467));
#25189=CARTESIAN_POINT('Ctrl Pts',(-1.86641799770841,0.704045754187782,
15.2349220473966));
#25190=CARTESIAN_POINT('Ctrl Pts',(-1.86179006631279,0.716194319169201,
15.2341141174458));
#25191=CARTESIAN_POINT('Ctrl Pts',(-1.85247175468876,0.739954575258685,
15.2325202680508));
#25192=CARTESIAN_POINT('Ctrl Pts',(-1.84779011653813,0.751569058163606,
15.2317346660948));
#25193=CARTESIAN_POINT('Ctrl Pts',(-1.84064671841057,0.768820552577513,
15.2305577431308));
#25194=CARTESIAN_POINT('Ctrl Pts',(-1.83826767770832,0.774491657655243,
15.230169222794));
#25195=CARTESIAN_POINT('Ctrl Pts',(-1.83397219844152,0.784599832766567,
15.2294737705707));
#25196=CARTESIAN_POINT('Ctrl Pts',(-1.83206577893743,0.789041128970013,
15.2291671815744));
#25197=CARTESIAN_POINT('Ctrl Pts',(-1.82800377910555,0.798410091612968,
15.2285182422574));
#25198=CARTESIAN_POINT('Ctrl Pts',(-1.82584437531591,0.803336048616278,
15.2281757632023));
#25199=CARTESIAN_POINT('Ctrl Pts',(-1.82005957604924,0.816388315963878,
15.2272648531099));
#25200=CARTESIAN_POINT('Ctrl Pts',(-1.81639971411059,0.824499131068781,
15.2266952436182));
#25201=CARTESIAN_POINT('Ctrl Pts',(-1.79907253452952,0.86222348185831,15.224029032601));
#25202=CARTESIAN_POINT('Ctrl Pts',(-1.78473517776987,0.891521986873294,
15.2219094195557));
#25203=CARTESIAN_POINT('Ctrl Pts',(-1.7438579943568,0.970113389341041,15.2160853490928));
#25204=CARTESIAN_POINT('Ctrl Pts',(-1.71595273161849,1.01865889723033,15.2123351915361));
#25205=CARTESIAN_POINT('Ctrl Pts',(-1.63022240228275,1.1542594522993,15.2014213903396));
#25206=CARTESIAN_POINT('Ctrl Pts',(-1.5675533622784,1.2380279510443,15.1941234151566));
#25207=CARTESIAN_POINT('Ctrl Pts',(-1.44751800232382,1.374668901293,15.1814421945112));
#25208=CARTESIAN_POINT('Ctrl Pts',(-1.39306822539288,1.42982011982667,15.1760658144811));
#25209=CARTESIAN_POINT('Ctrl Pts',(-1.30986335324619,1.50481929195788,15.1685122977678));
#25210=CARTESIAN_POINT('Ctrl Pts',(-1.28358081631915,1.52729949618003,15.1662131706301));
#25211=CARTESIAN_POINT('Ctrl Pts',(-1.25220267968629,1.55275559133462,15.1635805946313));
#25212=CARTESIAN_POINT('Ctrl Pts',(-1.24766402249621,1.55640482087588,15.163202477993));
#25213=CARTESIAN_POINT('Ctrl Pts',(-1.24036877857405,1.56221801798167,15.1625990595764));
#25214=CARTESIAN_POINT('Ctrl Pts',(-1.23762240050505,1.56439465506529,15.1623728756998));
#25215=CARTESIAN_POINT('Ctrl Pts',(-1.23274141573671,1.56824217279068,15.1619726476576));
#25216=CARTESIAN_POINT('Ctrl Pts',(-1.23060912428139,1.56991595131031,15.1617983972277));
#25217=CARTESIAN_POINT('Ctrl Pts',(-1.22609550621997,1.57344414625056,15.1614308010428));
#25218=CARTESIAN_POINT('Ctrl Pts',(-1.22371338743346,1.57529750125357,15.1612375305616));
#25219=CARTESIAN_POINT('Ctrl Pts',(-1.21732156993847,1.58024726640064,15.160720870029));
#25220=CARTESIAN_POINT('Ctrl Pts',(-1.21330423304413,1.58333384573065,15.160398171311));
#25221=CARTESIAN_POINT('Ctrl Pts',(-1.19401535039703,1.5980372563715,15.1588582124653));
#25222=CARTESIAN_POINT('Ctrl Pts',(-1.17858784541504,1.6094491251195,15.1576547644563));
#25223=CARTESIAN_POINT('Ctrl Pts',(-1.13510155823892,1.64065564156319,15.1543330275711));
#25224=CARTESIAN_POINT('Ctrl Pts',(-1.10669177363904,1.65995183301675,15.1522429472985));
#25225=CARTESIAN_POINT('Ctrl Pts',(-1.00124009921752,1.7276640850412,15.1447170002267));
#25226=CARTESIAN_POINT('Ctrl Pts',(-0.921405127454716,1.77153034581802,
15.1394544185937));
#25227=CARTESIAN_POINT('Ctrl Pts',(-0.696534339013358,1.87575914095947,
15.1250799494372));
#25228=CARTESIAN_POINT('Ctrl Pts',(-0.546959111374467,1.92469707869704,
15.1159464885486));
#25229=CARTESIAN_POINT('Ctrl Pts',(-0.380908247470206,1.95808422497812,
15.1053694082094));
#25230=CARTESIAN_POINT('Ctrl Pts',(-0.368587132168315,1.96044087889397,
15.1045824443923));
#25231=CARTESIAN_POINT('Ctrl Pts',(-0.350189480929749,1.96378022324521,
15.1034038752353));
#25232=CARTESIAN_POINT('Ctrl Pts',(-0.344129134898545,1.96485128569503,
15.103015082224));
#25233=CARTESIAN_POINT('Ctrl Pts',(-0.333300220069051,1.96671347438698,
15.1023193265262));
#25234=CARTESIAN_POINT('Ctrl Pts',(-0.328533528895954,1.96751534854255,
15.1020127078813));
#25235=CARTESIAN_POINT('Ctrl Pts',(-0.318459262704345,1.9691724561767,15.1013638982523));
#25236=CARTESIAN_POINT('Ctrl Pts',(-0.313151058556607,1.97002357289423,
15.1010215792733));
#25237=CARTESIAN_POINT('Ctrl Pts',(-0.299058785618285,1.97222473050573,
15.1001115443109));
#25238=CARTESIAN_POINT('Ctrl Pts',(-0.29026910264935,1.97353753161179,15.0995426538941));
#25239=CARTESIAN_POINT('Ctrl Pts',(-0.249299299617911,1.97937704102663,
15.0968848005136));
#25240=CARTESIAN_POINT('Ctrl Pts',(-0.217021984406268,1.98317544926241,
15.0947730011886));
#25241=CARTESIAN_POINT('Ctrl Pts',(-0.129216073968002,1.99133930929738,
15.0889759053021));
#25242=CARTESIAN_POINT('Ctrl Pts',(-0.0735774690030502,1.99417011351579,
15.0852454255007));
#25243=CARTESIAN_POINT('Ctrl Pts',(0.0863410709898142,1.99560499828671,
15.0743682201853));
#25244=CARTESIAN_POINT('Ctrl Pts',(0.190485317542087,1.9883677254945,15.067086962492));
#25245=CARTESIAN_POINT('Ctrl Pts',(0.368842389007298,1.96182901274293,15.0545134563551));
#25246=CARTESIAN_POINT('Ctrl Pts',(0.44341009782272,1.94633163668992,15.0492281869397));
#25247=CARTESIAN_POINT('Ctrl Pts',(0.552061654657239,1.91718015825094,15.0416306470847));
#25248=CARTESIAN_POINT('Ctrl Pts',(0.586947242990314,1.90678923212685,15.0392079963791));
#25249=CARTESIAN_POINT('Ctrl Pts',(0.627151514262558,1.89360595710644,15.0364507539518));
#25250=CARTESIAN_POINT('Ctrl Pts',(0.632763350600428,1.89173811266389,15.0360666884083));
#25251=CARTESIAN_POINT('Ctrl Pts',(0.641712149905379,1.88871531652209,15.0354556170125));
#25252=CARTESIAN_POINT('Ctrl Pts',(0.645054443832392,1.88757643425762,15.0352276938767));
#25253=CARTESIAN_POINT('Ctrl Pts',(0.650960803495403,1.88554633017055,15.0348254823307));
#25254=CARTESIAN_POINT('Ctrl Pts',(0.653526093965439,1.88465874252356,15.0346509805206));
#25255=CARTESIAN_POINT('Ctrl Pts',(0.658926436775886,1.8827778778209,15.0342840332829));
#25256=CARTESIAN_POINT('Ctrl Pts',(0.661761052539602,1.88178343491705,15.0340916586049));
#25257=CARTESIAN_POINT('Ctrl Pts',(0.66931016235145,1.87911588107262,15.0335799266968));
#25258=CARTESIAN_POINT('Ctrl Pts',(0.674020665720681,1.87743141856453,15.0332612379361));
#25259=CARTESIAN_POINT('Ctrl Pts',(0.696119985622988,1.86943487130393,15.0317688160012));
#25260=CARTESIAN_POINT('Ctrl Pts',(0.713427484007994,1.86289856322638,15.0306078837309));
#25261=CARTESIAN_POINT('Ctrl Pts',(0.890734578961677,1.79310355440872,15.0187717582043));
#25262=CARTESIAN_POINT('Ctrl Pts',(1.04202532815904,1.70962870249206,15.00910577681));
#25263=CARTESIAN_POINT('Ctrl Pts',(1.26972493122434,1.5424056940417,14.9925810546028));
#25264=CARTESIAN_POINT('Ctrl Pts',(1.35311867119392,1.46978957673048,14.9859976668641));
#25265=CARTESIAN_POINT('Ctrl Pts',(1.43908022240211,1.38139156267205,14.9783009980162));
#25266=CARTESIAN_POINT('Ctrl Pts',(1.44799836697333,1.3720405433729,14.9774906035349));
#25267=CARTESIAN_POINT('Ctrl Pts',(1.46107970562618,1.35805465789823,14.9762837463746));
#25268=CARTESIAN_POINT('Ctrl Pts',(1.46531317446124,1.35348574405218,14.9758903002234));
#25269=CARTESIAN_POINT('Ctrl Pts',(1.47279983858937,1.34532956893094,14.9751893352403));
#25270=CARTESIAN_POINT('Ctrl Pts',(1.47606151501364,1.34175013203158,14.9748821801282));
#25271=CARTESIAN_POINT('Ctrl Pts',(1.48288942211122,1.33420200594684,14.9742354355776));
#25272=CARTESIAN_POINT('Ctrl Pts',(1.48645282344283,1.33023081968834,14.9738957303736));
#25273=CARTESIAN_POINT('Ctrl Pts',(1.49578823918396,1.31974273705536,14.9729999823735));
#25274=CARTESIAN_POINT('Ctrl Pts',(1.50153354916492,1.31320232456329,14.9724428300073));
#25275=CARTESIAN_POINT('Ctrl Pts',(1.52729563045274,1.28348489009043,14.9699175734987));
#25276=CARTESIAN_POINT('Ctrl Pts',(1.5468189476705,1.25988744559841,14.967929316271));
#25277=CARTESIAN_POINT('Ctrl Pts',(1.59756783181815,1.19558995348401,14.9625528380557));
#25278=CARTESIAN_POINT('Ctrl Pts',(1.62777800869497,1.1541214463454,14.9591270637063));
#25279=CARTESIAN_POINT('Ctrl Pts',(1.71252213336685,1.02784024219568,14.9488194882605));
#25280=CARTESIAN_POINT('Ctrl Pts',(1.76226018648412,0.940012417867835,14.941800754716));
#25281=CARTESIAN_POINT('Ctrl Pts',(1.84139260246144,0.771723562317515,14.928826007052));
#25282=CARTESIAN_POINT('Ctrl Pts',(1.87266776147679,0.692388117021748,14.9228893921704));
#25283=CARTESIAN_POINT('Ctrl Pts',(1.9102041890702,0.575793566865182,14.9146106271431));
#25284=CARTESIAN_POINT('Ctrl Pts',(1.92063563320926,0.539979148710923,14.9121264681015));
#25285=CARTESIAN_POINT('Ctrl Pts',(1.93156257775568,0.49812555827962,14.909307317504));
#25286=CARTESIAN_POINT('Ctrl Pts',(1.93304187483262,0.492353710177109,14.9089203750672));
#25287=CARTESIAN_POINT('Ctrl Pts',(1.93535974414577,0.48313847064413,14.9083056063554));
#25288=CARTESIAN_POINT('Ctrl Pts',(1.93621502614915,0.479699378847779,14.9080768455621));
#25289=CARTESIAN_POINT('Ctrl Pts',(1.93770969084814,0.473620201269813,14.9076736745829));
#25290=CARTESIAN_POINT('Ctrl Pts',(1.93835285113517,0.470981067468106,14.9074990475611));
#25291=CARTESIAN_POINT('Ctrl Pts',(1.93969437176519,0.465426998435946,14.9071323933837));
#25292=CARTESIAN_POINT('Ctrl Pts',(1.94039155198076,0.462511807441816,14.9069404348515));
#25293=CARTESIAN_POINT('Ctrl Pts',(1.9422279643507,0.45475578954462,14.9064309918224));
#25294=CARTESIAN_POINT('Ctrl Pts',(1.94335567842903,0.449912215916506,14.9061141652831));
#25295=CARTESIAN_POINT('Ctrl Pts',(1.9485232235402,0.427335456758754,14.9046432912856));
#25296=CARTESIAN_POINT('Ctrl Pts',(1.95233868007559,0.40955107141852,14.9035015998676));
#25297=CARTESIAN_POINT('Ctrl Pts',(1.98663422462039,0.238307171274366,14.8926489748856));
#25298=CARTESIAN_POINT('Ctrl Pts',(1.99920750905528,0.0817929132677074,
14.8837790026025));
#25299=CARTESIAN_POINT('Ctrl Pts',(1.98863462462954,-0.200718385880195,
14.8673191846895));
#25300=CARTESIAN_POINT('Ctrl Pts',(1.9719578763923,-0.326084102407573,14.8598527150954));
#25301=CARTESIAN_POINT('Ctrl Pts',(1.94062593622361,-0.461700988290552,
14.8511652867954));
#25302=CARTESIAN_POINT('Ctrl Pts',(1.93757341671358,-0.474348046277771,
14.8503494086652));
#25303=CARTESIAN_POINT('Ctrl Pts',(1.93287265841588,-0.493021157499012,
14.849135940484));
#25304=CARTESIAN_POINT('Ctrl Pts',(1.9313194331916,-0.499070957808963,14.8487414157433));
#25305=CARTESIAN_POINT('Ctrl Pts',(1.92851102052709,-0.509800233966037,
14.8480392354362));
#25306=CARTESIAN_POINT('Ctrl Pts',(1.92726714461576,-0.514482640574314,
14.8477319481601));
#25307=CARTESIAN_POINT('Ctrl Pts',(1.92461989414998,-0.524303537053152,
14.8470856443031));
#25308=CARTESIAN_POINT('Ctrl Pts',(1.92321297258792,-0.529441023237143,
14.846746514691));
#25309=CARTESIAN_POINT('Ctrl Pts',(1.9194632355465,-0.542921302557391,14.8458539131069));
#25310=CARTESIAN_POINT('Ctrl Pts',(1.91708662422482,-0.551254500818922,
14.8452993456538));
#25311=CARTESIAN_POINT('Ctrl Pts',(1.90617667454421,-0.588584468351075,
14.8428023536974));
#25312=CARTESIAN_POINT('Ctrl Pts',(1.8970395997164,-0.61739920737807,14.8408403248901));
#25313=CARTESIAN_POINT('Ctrl Pts',(1.8709376268012,-0.69365532957347,14.8355517497883));
#25314=CARTESIAN_POINT('Ctrl Pts',(1.85282511125846,-0.740677871051671,
14.8321891437597));
#25315=CARTESIAN_POINT('Ctrl Pts',(1.79347697908041,-0.878908763841877,
14.822000968698));
#25316=CARTESIAN_POINT('Ctrl Pts',(1.74714085680376,-0.967747797229719,
14.8150381725344));
#25317=CARTESIAN_POINT('Ctrl Pts',(1.62933719241515,-1.15735008191424,14.7994637798773));
#25318=CARTESIAN_POINT('Ctrl Pts',(1.55477440098873,-1.25573998889278,14.7908723187804));
#25319=CARTESIAN_POINT('Ctrl Pts',(1.46650189535482,-1.35220443329619,14.7823355693203));
#25320=CARTESIAN_POINT('Ctrl Pts',(1.46136997719116,-1.35774903155914,14.7818445177215));
#25321=CARTESIAN_POINT('Ctrl Pts',(1.45381413645301,-1.36582000051582,14.7811293465781));
#25322=CARTESIAN_POINT('Ctrl Pts',(1.45141494420676,-1.36836927667659,14.7809033992405));
#25323=CARTESIAN_POINT('Ctrl Pts',(1.44714638968902,-1.37288099801883,14.7805034400217));
#25324=CARTESIAN_POINT('Ctrl Pts',(1.44527972616472,-1.37484596278961,14.7803292228468));
#25325=CARTESIAN_POINT('Ctrl Pts',(1.44132448642157,-1.37899253390432,14.7799615340296));
#25326=CARTESIAN_POINT('Ctrl Pts',(1.43923496454941,-1.38117319726308,14.7797681382884));
#25327=CARTESIAN_POINT('Ctrl Pts',(1.4336210208348,-1.38700543847324,14.779250788348));
#25328=CARTESIAN_POINT('Ctrl Pts',(1.43008757344184,-1.39064835648083,14.7789275287055));
#25329=CARTESIAN_POINT('Ctrl Pts',(1.41305977251629,-1.40807016641932,14.7773807929688));
#25330=CARTESIAN_POINT('Ctrl Pts',(1.39937940472645,-1.42166693105055,14.7761712765006));
#25331=CARTESIAN_POINT('Ctrl Pts',(1.36062312744969,-1.45908474841871,14.772828448244));
#25332=CARTESIAN_POINT('Ctrl Pts',(1.33512083489602,-1.48245615376489,14.7707237813228));
#25333=CARTESIAN_POINT('Ctrl Pts',(1.23980741855908,-1.56534958615536,14.7631401443741));
#25334=CARTESIAN_POINT('Ctrl Pts',(1.16651813537486,-1.62070338922514,14.7578365726643));
#25335=CARTESIAN_POINT('Ctrl Pts',(0.959271075542452,-1.75586578401537,
14.7434864113391));
#25336=CARTESIAN_POINT('Ctrl Pts',(0.819381425775328,-1.82534118989306,
14.7344156351421));
#25337=CARTESIAN_POINT('Ctrl Pts',(0.661003948046607,-1.88208916572404,
14.7239100001802));
#25338=CARTESIAN_POINT('Ctrl Pts',(0.649120498347943,-1.88622066952236,
14.7231207577561));
#25339=CARTESIAN_POINT('Ctrl Pts',(0.631360215353328,-1.89220765405401,
14.7219394347531));
#25340=CARTESIAN_POINT('Ctrl Pts',(0.62551242190712,-1.89414881576058,14.72155018606));
#25341=CARTESIAN_POINT('Ctrl Pts',(0.615060437903772,-1.89756464787097,
14.7208539227499));
#25342=CARTESIAN_POINT('Ctrl Pts',(0.610459683277312,-1.89904973856469,
14.7205472540992));
#25343=CARTESIAN_POINT('Ctrl Pts',(0.601170190040037,-1.90201107477083,
14.7199276547828));
#25344=CARTESIAN_POINT('Ctrl Pts',(0.59648130397468,-1.90348674259611,14.7196147076154));
#25345=CARTESIAN_POINT('Ctrl Pts',(0.583986723811788,-1.90736828798218,
14.7187802240287));
#25346=CARTESIAN_POINT('Ctrl Pts',(0.57617168964631,-1.90974355879213,14.7182576892593));
#25347=CARTESIAN_POINT('Ctrl Pts',(0.559099039307391,-1.91481821978313,
14.7171148022165));
#25348=CARTESIAN_POINT('Ctrl Pts',(0.549836032544862,-1.9174986003771,14.7164938431795));
#25349=CARTESIAN_POINT('Ctrl Pts',(0.522845912279533,-1.92509691877968,
14.7146818434446));
#25350=CARTESIAN_POINT('Ctrl Pts',(0.505070130984278,-1.92983681172478,
14.7134850998475));
#25351=CARTESIAN_POINT('Ctrl Pts',(0.443667653778369,-1.94530327288966,
14.7093388453182));
#25352=CARTESIAN_POINT('Ctrl Pts',(0.39974827929327,-1.9548009120681,14.7063514111754));
#25353=CARTESIAN_POINT('Ctrl Pts',(0.173425692977654,-1.99579761978097,
14.6908474355757));
#25354=CARTESIAN_POINT('Ctrl Pts',(-0.0123676467394637,-2.00327625017293,
14.6776477995529));
#25355=CARTESIAN_POINT('Ctrl Pts',(-0.205876688441953,-1.98411968517939,
14.6644020410063));
#25356=CARTESIAN_POINT('Ctrl Pts',(-0.215235721212382,-1.98312625056233,
14.6637629476002));
#25357=CARTESIAN_POINT('Ctrl Pts',(-0.263027584444043,-1.97771096549108,
14.660508349329));
#25358=CARTESIAN_POINT('Ctrl Pts',(-0.301336052990113,-1.97223762372811,
14.6579289971416));
#25359=CARTESIAN_POINT('Ctrl Pts',(-0.345973592532238,-1.96452881733855,
14.6549763543898));
#25360=CARTESIAN_POINT('Ctrl Pts',(-0.352477655690476,-1.96337227904,14.6545474549728));
#25361=CARTESIAN_POINT('Ctrl Pts',(-0.362315161909981,-1.96157253482772,
14.6539008685471));
#25362=CARTESIAN_POINT('Ctrl Pts',(-0.365652825840895,-1.9609531094126,
14.6536818671219));
#25363=CARTESIAN_POINT('Ctrl Pts',(-0.371635118917663,-1.95982707179363,
14.6532900253341));
#25364=CARTESIAN_POINT('Ctrl Pts',(-0.374280306503332,-1.95932362446945,
14.653117007348));
#25365=CARTESIAN_POINT('Ctrl Pts',(-0.379991175662831,-1.95822471170468,
14.652743994131));
#25366=CARTESIAN_POINT('Ctrl Pts',(-0.383056469736233,-1.95762740490456,
14.6525441058615));
#25367=CARTESIAN_POINT('Ctrl Pts',(-0.39155419293424,-1.95595080517453,
14.6519908397257));
#25368=CARTESIAN_POINT('Ctrl Pts',(-0.396983600992889,-1.95485607157423,
14.6516383330554));
#25369=CARTESIAN_POINT('Ctrl Pts',(-0.427107894392728,-1.94865141878452,
14.6496876405144));
#25370=CARTESIAN_POINT('Ctrl Pts',(-0.451710050428756,-1.94309590090232,
14.6481137347825));
#25371=CARTESIAN_POINT('Ctrl Pts',(-0.634194809744351,-1.89823468777809,
14.6365380993947));
#25372=CARTESIAN_POINT('Ctrl Pts',(-0.786863098619822,-1.84020620682486,
14.6273675226794));
#25373=CARTESIAN_POINT('Ctrl Pts',(-1.02985424164314,-1.7120077099945,14.6113061857728));
#25374=CARTESIAN_POINT('Ctrl Pts',(-1.12431648297316,-1.65150756914902,
14.6046332589389));
#25375=CARTESIAN_POINT('Ctrl Pts',(-1.22346629382407,-1.57553964285377,
14.596836584747));
#25376=CARTESIAN_POINT('Ctrl Pts',(-1.23365883797584,-1.56757162428156,
14.596025224356));
#25377=CARTESIAN_POINT('Ctrl Pts',(-1.24864502600964,-1.55561948978588,
14.5948172024474));
#25378=CARTESIAN_POINT('Ctrl Pts',(-1.25349880543022,-1.55171103667325,
14.5944235660231));
#25379=CARTESIAN_POINT('Ctrl Pts',(-1.26209197214017,-1.54472485289995,
14.5937223868507));
#25380=CARTESIAN_POINT('Ctrl Pts',(-1.26583863221877,-1.54165611399304,
14.5934152086284));
#25381=CARTESIAN_POINT('Ctrl Pts',(-1.26961833078248,-1.53853724684733,
14.5931038291399));
#25382=CARTESIAN_POINT('Ctrl Pts',(-1.26966260712151,-1.53850070844076,
14.5931001813545));
#25383=CARTESIAN_POINT('Ctrl Pts',(-1.26974953179697,-1.53842896880531,
14.5930930195013));
#25384=CARTESIAN_POINT('Ctrl Pts',(-1.26979218068056,-1.53839376735623,
14.5930895054035));
#25385=CARTESIAN_POINT('Ctrl Pts',(-1.26987592461901,-1.53832464109909,
14.5930826048583));
#25386=CARTESIAN_POINT('Ctrl Pts',(-1.26991701991006,-1.53829071630896,
14.5930792184052));
#25387=CARTESIAN_POINT('Ctrl Pts',(-1.26999772630241,-1.53822408651187,
14.5930725674516));
#25388=CARTESIAN_POINT('Ctrl Pts',(-1.27003733765258,-1.53819138149545,
14.5930693029432));
#25389=CARTESIAN_POINT('Ctrl Pts',(-1.27011514195353,-1.53812713750641,
14.5930628904947));
#25390=CARTESIAN_POINT('Ctrl Pts',(-1.27015333517176,-1.53809559849357,
14.5930597425441));
#25391=CARTESIAN_POINT('Ctrl Pts',(-1.2702283654229,-1.5380336356717,14.5930535581178));
#25392=CARTESIAN_POINT('Ctrl Pts',(-1.2702652027326,-1.53800321180065,14.5930505216301));
#25393=CARTESIAN_POINT('Ctrl Pts',(-1.27033758003062,-1.53794343114001,
14.5930445553093));
#25394=CARTESIAN_POINT('Ctrl Pts',(-1.27037312030605,-1.53791407426701,
14.5930416254625));
#25395=CARTESIAN_POINT('Ctrl Pts',(-1.27044295920464,-1.53785638207424,
14.5930358678639));
#25396=CARTESIAN_POINT('Ctrl Pts',(-1.27047725815306,-1.53782804662775,
14.5930330400944));
#25397=CARTESIAN_POINT('Ctrl Pts',(-1.2705446671855,-1.53777235409893,14.5930274823255));
#25398=CARTESIAN_POINT('Ctrl Pts',(-1.27057777759136,-1.53774499688193,
14.5930247523081));
#25399=CARTESIAN_POINT('Ctrl Pts',(-1.27064285953397,-1.53769121989276,
14.5930193859461));
#25400=CARTESIAN_POINT('Ctrl Pts',(-1.27067483141411,-1.53766479995823,
14.5930167495812));
#25401=CARTESIAN_POINT('Ctrl Pts',(-1.27073768369958,-1.53761285872956,
14.5930115666396));
#25402=CARTESIAN_POINT('Ctrl Pts',(-1.2707685644723,-1.53758733724417,14.5930090200398));
#25403=CARTESIAN_POINT('Ctrl Pts',(-1.27082927956527,-1.53753715603803,
14.5930040129373));
#25404=CARTESIAN_POINT('Ctrl Pts',(-1.27085911424879,-1.53751249612112,
14.5930015524113));
#25405=CARTESIAN_POINT('Ctrl Pts',(-1.2709177798195,-1.53746400310302,14.5929967139583));
#25406=CARTESIAN_POINT('Ctrl Pts',(-1.27094661112434,-1.53744016975308,
14.5929943360031));
#25407=CARTESIAN_POINT('Ctrl Pts',(-1.27100331047543,-1.53739329664454,
14.5929896593667));
#25408=CARTESIAN_POINT('Ctrl Pts',(-1.27103117896986,-1.53737025660492,
14.5929873606543));
#25409=CARTESIAN_POINT('Ctrl Pts',(-1.27108599125651,-1.53732493850628,
14.5929828393406));
#25410=CARTESIAN_POINT('Ctrl Pts',(-1.27111293550348,-1.53730266015431,
14.592980616707));
#25411=CARTESIAN_POINT('Ctrl Pts',(-1.27116593596108,-1.53725883536083,
14.5929762445421));
#25412=CARTESIAN_POINT('Ctrl Pts',(-1.27119199263413,-1.53723728861407,
14.5929740949777));
#25413=CARTESIAN_POINT('Ctrl Pts',(-1.27124325281111,-1.53719489842746,
14.5929698660895));
#25414=CARTESIAN_POINT('Ctrl Pts',(-1.27126845679979,-1.53717405465841,
14.5929677867305));
#25415=CARTESIAN_POINT('Ctrl Pts',(-1.27131804478319,-1.53713304320395,
14.5929636955298));
#25416=CARTESIAN_POINT('Ctrl Pts',(-1.27134242929451,-1.53711287515792,
14.5929616836499));
#25417=CARTESIAN_POINT('Ctrl Pts',(-1.27139040991838,-1.53707318921538,
14.5929577248135));
#25418=CARTESIAN_POINT('Ctrl Pts',(-1.27141400657607,-1.53705367092996,
14.5929557778161));
#25419=CARTESIAN_POINT('Ctrl Pts',(-1.2714604415981,-1.53701525979058,14.5929519462726));
#25420=CARTESIAN_POINT('Ctrl Pts',(-1.2714832805268,-1.53699636652747,14.5929500616837));
#25421=CARTESIAN_POINT('Ctrl Pts',(-1.27575141409662,-1.53346543777717,
14.5925978597812));
#25422=CARTESIAN_POINT('Ctrl Pts',(-1.27998210494452,-1.5299358579511,14.592246828577));
#25423=CARTESIAN_POINT('Ctrl Pts',(-1.29153930060784,-1.5202124321208,14.5912825839185));
#25424=CARTESIAN_POINT('Ctrl Pts',(-1.29883575475181,-1.51398324978483,
14.5906679235988));
#25425=CARTESIAN_POINT('Ctrl Pts',(-1.31496007599637,-1.50001512624289,
14.5892962620922));
#25426=CARTESIAN_POINT('Ctrl Pts',(-1.32376507517463,-1.49225044692981,
14.5885382042794));
#25427=CARTESIAN_POINT('Ctrl Pts',(-1.35046317354438,-1.46828451298885,
14.5862115641654));
#25428=CARTESIAN_POINT('Ctrl Pts',(-1.36813064579393,-1.45183630136658,
14.5846327087013));
#25429=CARTESIAN_POINT('Ctrl Pts',(-1.4331246173764,-1.38908767672252,14.5786737839427));
#25430=CARTESIAN_POINT('Ctrl Pts',(-1.47843105091569,-1.34076501709357,
14.5742097383838));
#25431=CARTESIAN_POINT('Ctrl Pts',(-1.64652228988481,-1.14258500881839,
14.5564034332814));
#25432=CARTESIAN_POINT('Ctrl Pts',(-1.74961210300578,-0.977440930746083,
14.542498689194));
#25433=CARTESIAN_POINT('Ctrl Pts',(-1.83204713369569,-0.789158946262437,
14.528982670265));
#25434=CARTESIAN_POINT('Ctrl Pts',(-1.83671218021921,-0.778239632900303,
14.5282069601541));
#25435=CARTESIAN_POINT('Ctrl Pts',(-1.84296713304245,-0.763229295130203,
14.5271523751145));
#25436=CARTESIAN_POINT('Ctrl Pts',(-1.84464133809237,-0.759173988697248,
14.5268686276136));
#25437=CARTESIAN_POINT('Ctrl Pts',(-1.84727939107534,-0.752723772621784,
14.526419199098));
#25438=CARTESIAN_POINT('Ctrl Pts',(-1.848251980349,-0.750332488890405,14.5262529940725));
#25439=CARTESIAN_POINT('Ctrl Pts',(-1.85024561867308,-0.745403378078806,
14.5259112550999));
#25440=CARTESIAN_POINT('Ctrl Pts',(-1.85126608798491,-0.742865342457778,
14.5257357594113));
#25441=CARTESIAN_POINT('Ctrl Pts',(-1.85366524738872,-0.736862685543493,
14.5253217883509));
#25442=CARTESIAN_POINT('Ctrl Pts',(-1.85503945815981,-0.733396261201187,
14.5250835834947));
#25443=CARTESIAN_POINT('Ctrl Pts',(-1.85954682786133,-0.721932771359423,
14.5242985978234));
#25444=CARTESIAN_POINT('Ctrl Pts',(-1.86263811161483,-0.713919185137957,
14.5237542781905));
#25445=CARTESIAN_POINT('Ctrl Pts',(-1.90307943843356,-0.607031516598376,
14.5165495530501));
#25446=CARTESIAN_POINT('Ctrl Pts',(-1.93257125688166,-0.505345141376698,
14.5103221302273));
#25447=CARTESIAN_POINT('Ctrl Pts',(-1.9809808172876,-0.269932199615473,
14.4963264032049));
#25448=CARTESIAN_POINT('Ctrl Pts',(-1.99467621243283,-0.135685087425805,
14.4886207563741));
#25449=CARTESIAN_POINT('Ctrl Pts',(-1.9947497026598,-0.00108914582907106,
14.4805293348879));
#25450=CARTESIAN_POINT('',(-1.99474935791997,0.0016004930108161,13.6790451185598));
#25451=CARTESIAN_POINT('Ctrl Pts',(-1.99474935792054,0.00160049230311827,
13.6790451186048));
#25452=CARTESIAN_POINT('Ctrl Pts',(-1.99480518364989,-0.0679770605314547,
13.6834740389305));
#25453=CARTESIAN_POINT('Ctrl Pts',(-1.99121636699624,-0.137603540603703,
13.6879029592563));
#25454=CARTESIAN_POINT('Ctrl Pts',(-1.98399420179308,-0.20686848419093,
13.692331879582));
#25455=CARTESIAN_POINT('Ctrl Pts',(-1.97677366562195,-0.276117804373161,
13.6967598009202));
#25456=CARTESIAN_POINT('Ctrl Pts',(-1.96592145888067,-0.345005261304889,
13.7011877222584));
#25457=CARTESIAN_POINT('Ctrl Pts',(-1.95150078725994,-0.413124968773165,
13.7056156435966));
#25458=CARTESIAN_POINT('Ctrl Pts',(-1.93707842336549,-0.481252670126485,
13.7100440845538));
#25459=CARTESIAN_POINT('Ctrl Pts',(-1.91908686764915,-0.548611962913746,
13.714472525511));
#25460=CARTESIAN_POINT('Ctrl Pts',(-1.8976401654057,-0.614808397095407,
13.7189009664682));
#25461=CARTESIAN_POINT('Ctrl Pts',(-1.87616885673531,-0.681080780376516,
13.7233344883049));
#25462=CARTESIAN_POINT('Ctrl Pts',(-1.85123464324678,-0.74618717445657,
13.7277680101415));
#25463=CARTESIAN_POINT('Ctrl Pts',(-1.82300076292189,-0.80975044358506,
13.7322015319782));
#25464=CARTESIAN_POINT('Ctrl Pts',(-1.79474856517079,-0.8733549509521,13.7366379301715));
#25465=CARTESIAN_POINT('Ctrl Pts',(-1.76319266460913,-0.9354139038495,13.7410743283648));
#25466=CARTESIAN_POINT('Ctrl Pts',(-1.72854227640487,-0.995574789345876,
13.7455107265581));
#25467=CARTESIAN_POINT('Ctrl Pts',(-1.6938298625014,-1.05584336543912,13.7499550660967));
#25468=CARTESIAN_POINT('Ctrl Pts',(-1.65601217440381,-1.11420668232168,
13.7543994056354));
#25469=CARTESIAN_POINT('Ctrl Pts',(-1.61534124467401,-1.17034192685515,
13.758843745174));
#25470=CARTESIAN_POINT('Ctrl Pts',(-1.5967195602771,-1.19604413760348,13.7608786405844));
#25471=CARTESIAN_POINT('Ctrl Pts',(-1.5775002754825,-1.22127973194823,13.7629135359947));
#25472=CARTESIAN_POINT('Ctrl Pts',(-1.55771020630618,-1.24602025491947,
13.7649484314051));
#25473=CARTESIAN_POINT('Ctrl Pts',(-1.51439312283603,-1.30017303675625,
13.7694024701231));
#25474=CARTESIAN_POINT('Ctrl Pts',(-1.46816300810093,-1.35217153646391,
13.773856508841));
#25475=CARTESIAN_POINT('Ctrl Pts',(-1.41926223182799,-1.40168551387486,
13.778310547559));
#25476=CARTESIAN_POINT('Ctrl Pts',(-1.37043496101952,-1.45112506408476,
13.7827578911648));
#25477=CARTESIAN_POINT('Ctrl Pts',(-1.31894533750337,-1.49808715881457,
13.7872052347706));
#25478=CARTESIAN_POINT('Ctrl Pts',(-1.2650762230469,-1.54227420142509,13.7916525783763));
#25479=CARTESIAN_POINT('Ctrl Pts',(-1.2112706147393,-1.58640915205424,13.7960946790211));
#25480=CARTESIAN_POINT('Ctrl Pts',(-1.15509146360779,-1.6277752391949,13.8005367796659));
#25481=CARTESIAN_POINT('Ctrl Pts',(-1.0968574485791,-1.66611263124572,13.8049788803107));
#25482=CARTESIAN_POINT('Ctrl Pts',(-1.03866016782506,-1.70442583989981,
13.8094181788587));
#25483=CARTESIAN_POINT('Ctrl Pts',(-0.978411002526847,-1.73971387491364,
13.8138574774067));
#25484=CARTESIAN_POINT('Ctrl Pts',(-0.916459356217322,-1.77175895959403,
13.8182967759548));
#25485=CARTESIAN_POINT('Ctrl Pts',(-0.854525737963603,-1.80379471908923,
13.8227347826578));
#25486=CARTESIAN_POINT('Ctrl Pts',(-0.790891056807318,-1.83258917684801,
13.8271727893609));
#25487=CARTESIAN_POINT('Ctrl Pts',(-0.725929612644464,-1.85797033345149,
13.831610796064));
#25488=CARTESIAN_POINT('Ctrl Pts',(-0.660964998985086,-1.88335272841242,
13.8360490192993));
#25489=CARTESIAN_POINT('Ctrl Pts',(-0.594673950661316,-1.90532131564903,
13.8404872425346));
#25490=CARTESIAN_POINT('Ctrl Pts',(-0.527449382701255,-1.92375276768821,
13.8449254657699));
#25491=CARTESIAN_POINT('Ctrl Pts',(-0.460153597730164,-1.94220374581679,
13.8493683908129));
#25492=CARTESIAN_POINT('Ctrl Pts',(-0.39192279228168,-1.95710997979983,
13.8538113158559));
#25493=CARTESIAN_POINT('Ctrl Pts',(-0.323162698535279,-1.96839869761575,
13.858254240899));
#25494=CARTESIAN_POINT('Ctrl Pts',(-0.254362466691924,-1.97969400512093,
13.8626997594602));
#25495=CARTESIAN_POINT('Ctrl Pts',(-0.185032818324061,-1.98736753950208,
13.8671452780215));
#25496=CARTESIAN_POINT('Ctrl Pts',(-0.115584490904185,-1.99139845032641,
13.8715907965827));
#25497=CARTESIAN_POINT('Ctrl Pts',(-0.0460149742143724,-1.99543639520265,
13.876044072698));
#25498=CARTESIAN_POINT('Ctrl Pts',(0.0236731454302083,-1.99581902516095,
13.8804973488132));
#25499=CARTESIAN_POINT('Ctrl Pts',(0.0930700454494838,-1.99257760931413,
13.8849506249284));
#25500=CARTESIAN_POINT('Ctrl Pts',(0.130230089777915,-1.99084192434087,
13.8873352262262));
#25501=CARTESIAN_POINT('Ctrl Pts',(0.167306729918206,-1.98806800686027,
13.889719827524));
#25502=CARTESIAN_POINT('Ctrl Pts',(0.204238144126611,-1.98426670157611,
13.8921044288218));
#25503=CARTESIAN_POINT('Ctrl Pts',(0.273219884993038,-1.97716649537802,
13.8965584675398));
#25504=CARTESIAN_POINT('Ctrl Pts',(0.341967546588619,-1.96645078236383,
13.9010125062578));
#25505=CARTESIAN_POINT('Ctrl Pts',(0.410072255166582,-1.95214454076602,
13.9054665449758));
#25506=CARTESIAN_POINT('Ctrl Pts',(0.478074591785962,-1.93785980367214,
13.9099138885815));
#25507=CARTESIAN_POINT('Ctrl Pts',(0.545435418367895,-1.91999534976437,
13.9143612321873));
#25508=CARTESIAN_POINT('Ctrl Pts',(0.611751383587362,-1.89862787485567,
13.918808575793));
#25509=CARTESIAN_POINT('Ctrl Pts',(0.677989169100425,-1.87728559000353,
13.9232506764378));
#25510=CARTESIAN_POINT('Ctrl Pts',(0.743184076008251,-1.85244863567209,
13.9276927770826));
#25511=CARTESIAN_POINT('Ctrl Pts',(0.806945112391134,-1.82424426765937,
13.9321348777274));
#25512=CARTESIAN_POINT('Ctrl Pts',(0.870665928029795,-1.79605769108694,
13.9365741762754));
#25513=CARTESIAN_POINT('Ctrl Pts',(0.932954220771736,-1.76450811230122,
13.9410134748235));
#25514=CARTESIAN_POINT('Ctrl Pts',(0.993437722011937,-1.72977138806946,
13.9454527733715));
#25515=CARTESIAN_POINT('Ctrl Pts',(1.05390362242961,-1.69504477229547,13.9498907800745));
#25516=CARTESIAN_POINT('Ctrl Pts',(1.11256534963501,-1.65713309593098,13.9543287867776));
#25517=CARTESIAN_POINT('Ctrl Pts',(1.16907564342495,-1.61625793190646,13.9587667934807));
#25518=CARTESIAN_POINT('Ctrl Pts',(1.22558869437612,-1.57538077356533,13.963205016716));
#25519=CARTESIAN_POINT('Ctrl Pts',(1.27994970824177,-1.53154012935786,13.9676432399513));
#25520=CARTESIAN_POINT('Ctrl Pts',(1.33184226767023,-1.48499957459489,13.9720814631866));
#25521=CARTESIAN_POINT('Ctrl Pts',(1.38378980153872,-1.43840971525021,13.9765243882296));
#25522=CARTESIAN_POINT('Ctrl Pts',(1.4332632962628,-1.38911456393194,13.9809673132726));
#25523=CARTESIAN_POINT('Ctrl Pts',(1.47998190000941,-1.33741584338774,13.9854102383157));
#25524=CARTESIAN_POINT('Ctrl Pts',(1.52672777532802,-1.28568694417237,13.9898557568769));
#25525=CARTESIAN_POINT('Ctrl Pts',(1.570715250024,-1.23155206315671,13.9943012754382));
#25526=CARTESIAN_POINT('Ctrl Pts',(1.61170441580573,-1.17534524228939,13.9987467939994));
#25527=CARTESIAN_POINT('Ctrl Pts',(1.65276510882595,-1.11904033895067,14.0032000701147));
#25528=CARTESIAN_POINT('Ctrl Pts',(1.69081678137464,-1.06065668848638,14.0076533462299));
#25529=CARTESIAN_POINT('Ctrl Pts',(1.72566384039382,-1.00055578178192,14.0121066223451));
#25530=CARTESIAN_POINT('Ctrl Pts',(1.7443234384093,-0.96837347455039,14.014491223643));
#25531=CARTESIAN_POINT('Ctrl Pts',(1.76206497861807,-0.935699178638638,
14.0168758249408));
#25532=CARTESIAN_POINT('Ctrl Pts',(1.77886410776198,-0.902590742593891,
14.0192604262386));
#25533=CARTESIAN_POINT('Ctrl Pts',(1.81024208767997,-0.840749689261355,
14.0237144649566));
#25534=CARTESIAN_POINT('Ctrl Pts',(1.83845356975254,-0.777147961615591,
14.0281685036746));
#25535=CARTESIAN_POINT('Ctrl Pts',(1.86329818552637,-0.712142846846149,
14.0326225423925));
#25536=CARTESIAN_POINT('Ctrl Pts',(1.88810545598251,-0.647235444864242,
14.0370698859983));
#25537=CARTESIAN_POINT('Ctrl Pts',(1.90955573146319,-0.580929296182433,
14.041517229604));
#25538=CARTESIAN_POINT('Ctrl Pts',(1.92749511536451,-0.513605045483351,
14.0459645732098));
#25539=CARTESIAN_POINT('Ctrl Pts',(1.94541335057622,-0.446360163155503,
14.0504066738546));
#25540=CARTESIAN_POINT('Ctrl Pts',(1.95982878930143,-0.378100033405074,
14.0548487744994));
#25541=CARTESIAN_POINT('Ctrl Pts',(1.97063673515249,-0.309222283426575,
14.0592908751442));
#25542=CARTESIAN_POINT('Ctrl Pts',(1.98143786330341,-0.240387981837958,
14.0637301736922));
#25543=CARTESIAN_POINT('Ctrl Pts',(1.98863593717698,-0.170937315413736,
14.0681694722402));
#25544=CARTESIAN_POINT('Ctrl Pts',(1.99217725904039,-0.101278482721227,
14.0726087707882));
#25545=CARTESIAN_POINT('Ctrl Pts',(1.9957175503719,-0.031639920891463,14.0770467774913));
#25546=CARTESIAN_POINT('Ctrl Pts',(1.99560317730049,0.0382061982726219,
14.0814847841943));
#25547=CARTESIAN_POINT('Ctrl Pts',(1.99183241814654,0.107847950933335,14.0859227908974));
#25548=CARTESIAN_POINT('Ctrl Pts',(1.98806147501563,0.177493101445062,14.0903610141327));
#25549=CARTESIAN_POINT('Ctrl Pts',(1.98063382047608,0.246933376942141,14.094799237368));
#25550=CARTESIAN_POINT('Ctrl Pts',(1.96959974535076,0.315760044360018,14.0992374606033));
#25551=CARTESIAN_POINT('Ctrl Pts',(1.95855398084057,0.384659626036245,14.1036803856464));
#25552=CARTESIAN_POINT('Ctrl Pts',(1.94389424765023,0.452943817812173,14.1081233106894));
#25553=CARTESIAN_POINT('Ctrl Pts',(1.9257221649402,0.520213135126373,14.1125662357324));
#25554=CARTESIAN_POINT('Ctrl Pts',(1.90753947443753,0.587521720309926,14.1170117542937));
#25555=CARTESIAN_POINT('Ctrl Pts',(1.88584050586163,0.653813786467538,14.1214572728549));
#25556=CARTESIAN_POINT('Ctrl Pts',(1.86077621830273,0.718706774629961,14.1259027914162));
#25557=CARTESIAN_POINT('Ctrl Pts',(1.83566819286234,0.783713002868256,14.1303560675314));
#25558=CARTESIAN_POINT('Ctrl Pts',(1.80718332580817,0.847314832827739,14.1348093436466));
#25559=CARTESIAN_POINT('Ctrl Pts',(1.77551964692295,0.909152102725731,14.1392626197619));
#25560=CARTESIAN_POINT('Ctrl Pts',(1.7585646574255,0.942264182515052,14.1416472210597));
#25561=CARTESIAN_POINT('Ctrl Pts',(1.74069897737165,0.974870766796611,14.1440318223575));
#25562=CARTESIAN_POINT('Ctrl Pts',(1.72195805822019,1.00692006049663,14.1464164236553));
#25563=CARTESIAN_POINT('Ctrl Pts',(1.68695313744456,1.06678281204141,14.1508704623733));
#25564=CARTESIAN_POINT('Ctrl Pts',(1.64875353704919,1.12493655663194,14.1553245010913));
#25565=CARTESIAN_POINT('Ctrl Pts',(1.60755116707231,1.1810193934667,14.1597785398093));
#25566=CARTESIAN_POINT('Ctrl Pts',(1.5664107306592,1.237017929084,14.164225883415));
#25567=CARTESIAN_POINT('Ctrl Pts',(1.52227677058713,1.29095134395445,14.1686732270208));
#25568=CARTESIAN_POINT('Ctrl Pts',(1.47538599529214,1.34248416281006,14.1731205706265));
#25569=CARTESIAN_POINT('Ctrl Pts',(1.42855049940136,1.39395622976926,14.1775626712713));
#25570=CARTESIAN_POINT('Ctrl Pts',(1.3789649710888,1.44303296121249,14.1820047719161));
#25571=CARTESIAN_POINT('Ctrl Pts',(1.32690703454506,1.48941105279061,14.1864468725609));
#25572=CARTESIAN_POINT('Ctrl Pts',(1.27488193637831,1.53575988886311,14.1908861711089));
#25573=CARTESIAN_POINT('Ctrl Pts',(1.22038788856991,1.57941313716979,14.1953254696569));
#25574=CARTESIAN_POINT('Ctrl Pts',(1.16373901454757,1.62010464739777,14.199764768205));
#25575=CARTESIAN_POINT('Ctrl Pts',(1.10710662546348,1.66078431631302,14.204202774908));
#25576=CARTESIAN_POINT('Ctrl Pts',(1.04832105238655,1.69850367263701,14.2086407816111));
#25577=CARTESIAN_POINT('Ctrl Pts',(0.987727691244489,1.73303824840909,14.2130787883141));
#25578=CARTESIAN_POINT('Ctrl Pts',(0.927131373726373,1.76757450913791,14.2175170115495));
#25579=CARTESIAN_POINT('Ctrl Pts',(0.864727519542407,1.79892544048044,14.2219552347848));
#25580=CARTESIAN_POINT('Ctrl Pts',(0.800887002138789,1.82691203190114,14.2263934580201));
#25581=CARTESIAN_POINT('Ctrl Pts',(0.736978852752398,1.85492827202685,14.2308363830631));
#25582=CARTESIAN_POINT('Ctrl Pts',(0.671631451598135,1.87957286141456,14.2352793081061));
#25583=CARTESIAN_POINT('Ctrl Pts',(0.605235686143643,1.90071495146385,14.2397222331492));
#25584=CARTESIAN_POINT('Ctrl Pts',(0.538801162747885,1.92186938302135,14.2441677517104));
#25585=CARTESIAN_POINT('Ctrl Pts',(0.471317530766223,1.93951712189295,14.2486132702717));
#25586=CARTESIAN_POINT('Ctrl Pts',(0.403188160569807,1.9535779661115,14.2530587888329));
#25587=CARTESIAN_POINT('Ctrl Pts',(0.334939902720654,1.96766334689569,14.2575120649482));
#25588=CARTESIAN_POINT('Ctrl Pts',(0.266044141236429,1.97814926482375,14.2619653410634));
#25589=CARTESIAN_POINT('Ctrl Pts',(0.196910900515753,1.98500721906951,14.2664186171786));
#25590=CARTESIAN_POINT('Ctrl Pts',(0.159892038159701,1.98867945635539,14.2688032184764));
#25591=CARTESIAN_POINT('Ctrl Pts',(0.122805116298964,1.99131234244859,14.2711878197742));
#25592=CARTESIAN_POINT('Ctrl Pts',(0.0857128758712415,1.99290764096329,
14.273572421072));
#25593=CARTESIAN_POINT('Ctrl Pts',(0.0164307383689842,1.99588739332601,
14.27802645979));
#25594=CARTESIAN_POINT('Ctrl Pts',(-0.0531441760713303,1.99525591815407,
14.282480498508));
#25595=CARTESIAN_POINT('Ctrl Pts',(-0.122603694260102,1.99097862787469,
14.286934537226));
#25596=CARTESIAN_POINT('Ctrl Pts',(-0.191958804001189,1.98670776702715,
14.2913818808318));
#25597=CARTESIAN_POINT('Ctrl Pts',(-0.261198377109999,1.97880199780628,
14.2958292244375));
#25598=CARTESIAN_POINT('Ctrl Pts',(-0.329912203479769,1.96727870432614,
14.3002765680433));
#25599=CARTESIAN_POINT('Ctrl Pts',(-0.398545023311044,1.95576899562458,
14.3047186686881));
#25600=CARTESIAN_POINT('Ctrl Pts',(-0.466652846918377,1.94065031345129,
14.3091607693329));
#25601=CARTESIAN_POINT('Ctrl Pts',(-0.533830359862819,1.92199185986537,
14.3136028699777));
#25602=CARTESIAN_POINT('Ctrl Pts',(-0.600965496934571,1.9033451761146,14.3180421685257));
#25603=CARTESIAN_POINT('Ctrl Pts',(-0.667171016897516,1.88116328122908,
14.3224814670737));
#25604=CARTESIAN_POINT('Ctrl Pts',(-0.732053081728854,1.85556617991148,
14.3269207656218));
#25605=CARTESIAN_POINT('Ctrl Pts',(-0.79691626574654,1.82997652740275,14.3313587723248));
#25606=CARTESIAN_POINT('Ctrl Pts',(-0.860456304003943,1.80097382094747,
14.3357967790279));
#25607=CARTESIAN_POINT('Ctrl Pts',(-0.922297471927478,1.76872692515724,
14.340234785731));
#25608=CARTESIAN_POINT('Ctrl Pts',(-0.984141657108056,1.73647845602717,
14.3446730089663));
#25609=CARTESIAN_POINT('Ctrl Pts',(-1.04428637440759,1.70098571178254,14.3491112322016));
#25610=CARTESIAN_POINT('Ctrl Pts',(-1.10238032409432,1.66246358863877,14.3535494554369));
#25611=CARTESIAN_POINT('Ctrl Pts',(-1.16053581790957,1.62390065555679,14.3579923804799));
#25612=CARTESIAN_POINT('Ctrl Pts',(-1.21663579895897,1.58230220907177,14.362435305523));
#25613=CARTESIAN_POINT('Ctrl Pts',(-1.27035862419177,1.53792604778045,14.366878230566));
#25614=CARTESIAN_POINT('Ctrl Pts',(-1.3241128096489,1.49352398229725,14.3713237491272));
#25615=CARTESIAN_POINT('Ctrl Pts',(-1.37548671666606,1.44634130591597,14.3757692676885));
#25616=CARTESIAN_POINT('Ctrl Pts',(-1.42419452533855,1.39667373301559,14.3802147862498));
#25617=CARTESIAN_POINT('Ctrl Pts',(-1.47298733049687,1.34691948881401,14.384668062365));
#25618=CARTESIAN_POINT('Ctrl Pts',(-1.51910442631869,1.29467205922888,14.3891213384802));
#25619=CARTESIAN_POINT('Ctrl Pts',(-1.56229985845326,1.24026074467304,14.3935746145955));
#25620=CARTESIAN_POINT('Ctrl Pts',(-1.58542977019919,1.21112505042334,14.3959592158932));
#25621=CARTESIAN_POINT('Ctrl Pts',(-1.60772268783294,1.18136941758474,14.398343817191));
#25622=CARTESIAN_POINT('Ctrl Pts',(-1.62914612543946,1.15104755091421,14.4007284184888));
#25623=CARTESIAN_POINT('Ctrl Pts',(-1.66957974506708,1.09381944187431,14.4052290062846));
#25624=CARTESIAN_POINT('Ctrl Pts',(-1.70707223248772,1.03434819745607,14.4097295940805));
#25625=CARTESIAN_POINT('Ctrl Pts',(-1.74136940073319,0.972964630749814,
14.4142301818764));
#25626=CARTESIAN_POINT('Ctrl Pts',(-1.77561242103956,0.911677975648865,
14.4187236642007));
#25627=CARTESIAN_POINT('Ctrl Pts',(-1.80666990660374,0.848485403704244,
14.423217146525));
#25628=CARTESIAN_POINT('Ctrl Pts',(-1.83433017896719,0.783747636060353,
14.4277106288492));
#25629=CARTESIAN_POINT('Ctrl Pts',(-1.8619505888703,0.719103164919873,14.4321976354144));
#25630=CARTESIAN_POINT('Ctrl Pts',(-1.88618333064802,0.652918359543348,
14.4366846419796));
#25631=CARTESIAN_POINT('Ctrl Pts',(-1.90686288451596,0.585577921506146,
14.4411716485448));
#25632=CARTESIAN_POINT('Ctrl Pts',(-1.92752471738716,0.51829518972756,14.445654810045));
#25633=CARTESIAN_POINT('Ctrl Pts',(-1.9446392685461,0.449859245091323,14.4501379715452));
#25634=CARTESIAN_POINT('Ctrl Pts',(-1.958089803987,0.380672933135736,14.4546211330453));
#25635=CARTESIAN_POINT('Ctrl Pts',(-1.97153482224691,0.311515000229131,
14.4591024556289));
#25636=CARTESIAN_POINT('Ctrl Pts',(-1.98131871235937,0.241607776836367,
14.4635837782125));
#25637=CARTESIAN_POINT('Ctrl Pts',(-1.98737547173003,0.171365973477396,
14.468065100796));
#25638=CARTESIAN_POINT('Ctrl Pts',(-1.99232217548495,0.113997771908761,
14.4717251067323));
#25639=CARTESIAN_POINT('Ctrl Pts',(-1.99478366955174,0.056406735287098,
14.4753851126685));
#25640=CARTESIAN_POINT('Ctrl Pts',(-1.99474965194692,-0.00117837076332067,
14.4790451186048));
#25641=CARTESIAN_POINT('',(-1.99502628289053,0.000403632376691979,12.8790451529297));
#25642=CARTESIAN_POINT('Ctrl Pts',(-1.99474995918462,0.000403525672960359,
12.879045156187));
#25643=CARTESIAN_POINT('Ctrl Pts',(-1.99476391393369,-0.0685790372895848,
12.8834750243028));
#25644=CARTESIAN_POINT('Ctrl Pts',(-1.99119525037218,-0.137704781892064,
12.8879048924186));
#25645=CARTESIAN_POINT('Ctrl Pts',(-1.98402549375135,-0.206568154962712,
12.8923347605343));
#25646=CARTESIAN_POINT('Ctrl Pts',(-1.97662908922472,-0.277608413542726,
12.8969046641331));
#25647=CARTESIAN_POINT('Ctrl Pts',(-1.96539997991584,-0.348368906523431,
12.9014745677318));
#25648=CARTESIAN_POINT('Ctrl Pts',(-1.95037610598785,-0.41840244704314,
12.9060444713306));
#25649=CARTESIAN_POINT('Ctrl Pts',(-1.93585123391419,-0.486109898649093,
12.9104625904841));
#25650=CARTESIAN_POINT('Ctrl Pts',(-1.91777983112837,-0.553137400773518,
12.9148807096376));
#25651=CARTESIAN_POINT('Ctrl Pts',(-1.89624871509232,-0.619086724951126,
12.9192988287911));
#25652=CARTESIAN_POINT('Ctrl Pts',(-1.87473021050309,-0.684997420550787,
12.9237143601143));
#25653=CARTESIAN_POINT('Ctrl Pts',(-1.84975616507364,-0.749830720662124,
12.9281298914375));
#25654=CARTESIAN_POINT('Ctrl Pts',(-1.82146361149838,-0.813202234679232,
12.9325454227606));
#25655=CARTESIAN_POINT('Ctrl Pts',(-1.79317774934347,-0.876558760814886,
12.9369599097746));
#25656=CARTESIAN_POINT('Ctrl Pts',(-1.76157513909554,-0.938453734973087,
12.9413743967885));
#25657=CARTESIAN_POINT('Ctrl Pts',(-1.7268407424001,-0.998523215998043,
12.9457888838024));
#25658=CARTESIAN_POINT('Ctrl Pts',(-1.69210243074373,-1.05859946753562,
12.9502038683791));
#25659=CARTESIAN_POINT('Ctrl Pts',(-1.65423188280755,-1.11684939032358,
12.9546188529558));
#25660=CARTESIAN_POINT('Ctrl Pts',(-1.61345881382973,-1.172935726532,12.9590338375325));
#25661=CARTESIAN_POINT('Ctrl Pts',(-1.57264128067329,-1.22908322646772,
12.9634536367741));
#25662=CARTESIAN_POINT('Ctrl Pts',(-1.52891520507429,-1.2830620325987,12.9678734360157));
#25663=CARTESIAN_POINT('Ctrl Pts',(-1.48255157511328,-1.33456674229097,
12.9722932352573));
#25664=CARTESIAN_POINT('Ctrl Pts',(-1.4361574262443,-1.38610535501234,12.9767159438364));
#25665=CARTESIAN_POINT('Ctrl Pts',(-1.38712262046823,-1.43516628284959,
12.9811386524155));
#25666=CARTESIAN_POINT('Ctrl Pts',(-1.33575408848825,-1.48148188567627,
12.9855613609945));
#25667=CARTESIAN_POINT('Ctrl Pts',(-1.2843006711123,-1.527874024042,12.9899913780045));
#25668=CARTESIAN_POINT('Ctrl Pts',(-1.23050622131947,-1.57151148022315,
12.9944213950146));
#25669=CARTESIAN_POINT('Ctrl Pts',(-1.17470881658145,-1.61216834069703,
12.9988514120246));
#25670=CARTESIAN_POINT('Ctrl Pts',(-1.16143741963982,-1.62183856346604,
12.9999050903179));
#25671=CARTESIAN_POINT('Ctrl Pts',(-1.14805282609176,-1.63134036776859,
13.0009587686113));
#25672=CARTESIAN_POINT('Ctrl Pts',(-1.13455979011492,-1.64067109597091,
13.0020124469047));
#25673=CARTESIAN_POINT('Ctrl Pts',(-1.07752292692536,-1.68011332890113,
13.0064664856227));
#25674=CARTESIAN_POINT('Ctrl Pts',(-1.01831387977906,-1.71665585503574,
13.0109205243406));
#25675=CARTESIAN_POINT('Ctrl Pts',(-0.957259602578503,-1.75005188945107,
13.0153745630586));
#25676=CARTESIAN_POINT('Ctrl Pts',(-0.896297099442749,-1.78339772443784,
13.0198219066644));
#25677=CARTESIAN_POINT('Ctrl Pts',(-0.833495297299515,-1.81360622189784,
13.0242692502701));
#25678=CARTESIAN_POINT('Ctrl Pts',(-0.769210569644161,-1.84047348854791,
13.0287165938759));
#25679=CARTESIAN_POINT('Ctrl Pts',(-0.705001627074957,-1.86730908145225,
13.0331586945207));
#25680=CARTESIAN_POINT('Ctrl Pts',(-0.639313680689665,-1.8908110789602,
13.0376007951655));
#25681=CARTESIAN_POINT('Ctrl Pts',(-0.572526575468782,-1.91082204375028,
13.0420428958103));
#25682=CARTESIAN_POINT('Ctrl Pts',(-0.505781599849651,-1.93082038553514,
13.0464821943583));
#25683=CARTESIAN_POINT('Ctrl Pts',(-0.437939308724834,-1.94733192299265,
13.0509214929063));
#25684=CARTESIAN_POINT('Ctrl Pts',(-0.369396909037524,-1.96024832255853,
13.0553607914543));
#25685=CARTESIAN_POINT('Ctrl Pts',(-0.300874455328736,-1.97316096342571,
13.0597987981574));
#25686=CARTESIAN_POINT('Ctrl Pts',(-0.231652778346969,-1.98248045264572,
13.0642368048605));
#25687=CARTESIAN_POINT('Ctrl Pts',(-0.162139795614553,-1.98814945343102,
13.0686748115635));
#25688=CARTESIAN_POINT('Ctrl Pts',(-0.0926234213143076,-1.99381873080927,
13.0731130347988));
#25689=CARTESIAN_POINT('Ctrl Pts',(-0.0228162011802754,-1.99583712873204,
13.0775512580341));
#25690=CARTESIAN_POINT('Ctrl Pts',(0.0468700844463606,-1.99419927732511,
13.0819894812694));
#25691=CARTESIAN_POINT('Ctrl Pts',(0.116630195002359,-1.99255969079536,
13.0864324063125));
#25692=CARTESIAN_POINT('Ctrl Pts',(0.186268624934378,-1.98725613535523,
13.0908753313555));
#25693=CARTESIAN_POINT('Ctrl Pts',(0.255375825712517,-1.97833534825157,
13.0953182563985));
#25694=CARTESIAN_POINT('Ctrl Pts',(0.324523367208244,-1.96940935371729,
13.0997637749598));
#25695=CARTESIAN_POINT('Ctrl Pts',(0.393138580608946,-1.95686201285637,
13.104209293521));
#25696=CARTESIAN_POINT('Ctrl Pts',(0.46082202448935,-1.94079123664693,13.1086548120823));
#25697=CARTESIAN_POINT('Ctrl Pts',(0.528623577868769,-1.92469241648439,
13.1131080881975));
#25698=CARTESIAN_POINT('Ctrl Pts',(0.595489646332659,-1.9050580253944,13.1175613643127));
#25699=CARTESIAN_POINT('Ctrl Pts',(0.661036623490899,-1.88203563858492,
13.122014640428));
#25700=CARTESIAN_POINT('Ctrl Pts',(0.696135144838806,-1.86970781249828,
13.1243992417258));
#25701=CARTESIAN_POINT('Ctrl Pts',(0.730855791739241,-1.85640937119444,
13.1267838430236));
#25702=CARTESIAN_POINT('Ctrl Pts',(0.765142455865676,-1.84216844635116,
13.1291684443214));
#25703=CARTESIAN_POINT('Ctrl Pts',(0.829184243341866,-1.81556876669395,
13.1336224830394));
#25704=CARTESIAN_POINT('Ctrl Pts',(0.891964126641946,-1.78557287142334,
13.1380765217574));
#25705=CARTESIAN_POINT('Ctrl Pts',(0.953097602768725,-1.75232203721134,
13.1425305604753));
#25706=CARTESIAN_POINT('Ctrl Pts',(1.01413918578238,-1.71912118416945,13.1469779040811));
#25707=CARTESIAN_POINT('Ctrl Pts',(1.07353884693997,-1.68267533494663,13.1514252476868));
#25708=CARTESIAN_POINT('Ctrl Pts',(1.13093221659763,-1.64317372300118,13.1558725912926));
#25709=CARTESIAN_POINT('Ctrl Pts',(1.188257925372,-1.6037186793958,13.1603146919374));
#25710=CARTESIAN_POINT('Ctrl Pts',(1.24358163892513,-1.56121530416657,13.1647567925822));
#25711=CARTESIAN_POINT('Ctrl Pts',(1.2965653380723,-1.5158977164075,13.1691988932269));
#25712=CARTESIAN_POINT('Ctrl Pts',(1.34951561486733,-1.47060871518354,13.173638191775));
#25713=CARTESIAN_POINT('Ctrl Pts',(1.40012843430692,-1.42250934052396,13.178077490323));
#25714=CARTESIAN_POINT('Ctrl Pts',(1.44809766158735,-1.37187489407936,13.182516788871));
#25715=CARTESIAN_POINT('Ctrl Pts',(1.49605292972452,-1.32125518236226,13.1869547955741));
#25716=CARTESIAN_POINT('Ctrl Pts',(1.54136579634628,-1.26810221855024,13.1913928022771));
#25717=CARTESIAN_POINT('Ctrl Pts',(1.58376720373819,-1.21272791955298,13.1958308089802));
#25718=CARTESIAN_POINT('Ctrl Pts',(1.62617067991297,-1.1573509188199,13.2002690322155));
#25719=CARTESIAN_POINT('Ctrl Pts',(1.66566211909979,-1.09975275787685,13.2047072554508));
#25720=CARTESIAN_POINT('Ctrl Pts',(1.70201406378162,-1.04027673682995,13.2091454786861));
#25721=CARTESIAN_POINT('Ctrl Pts',(1.73840451933701,-0.980737707502589,
13.2135884037292));
#25722=CARTESIAN_POINT('Ctrl Pts',(1.77164858613558,-0.919317265902124,
13.2180313287722));
#25723=CARTESIAN_POINT('Ctrl Pts',(1.80156382444342,-0.856385047135232,
13.2224742538152));
#25724=CARTESIAN_POINT('Ctrl Pts',(1.8314965255072,-0.793416092241892,13.2269197723765));
#25725=CARTESIAN_POINT('Ctrl Pts',(1.85809634366653,-0.728934056397803,
13.2313652909377));
#25726=CARTESIAN_POINT('Ctrl Pts',(1.88122933599327,-0.663327783149731,
13.235810809499));
#25727=CARTESIAN_POINT('Ctrl Pts',(1.90440269603738,-0.597607025123411,
13.2402640856142));
#25728=CARTESIAN_POINT('Ctrl Pts',(1.92409701561062,-0.5307585830934,13.2447173617295));
#25729=CARTESIAN_POINT('Ctrl Pts',(1.94022868063529,-0.463184875983908,
13.2491706378447));
#25730=CARTESIAN_POINT('Ctrl Pts',(1.94886672336118,-0.427001099029362,
13.2515552391425));
#25731=CARTESIAN_POINT('Ctrl Pts',(1.95648412833892,-0.390609520282348,
13.2539398404403));
#25732=CARTESIAN_POINT('Ctrl Pts',(1.96307416977555,-0.354072544064099,
13.2563244417381));
#25733=CARTESIAN_POINT('Ctrl Pts',(1.97538327140143,-0.285827547777349,
13.2607784804561));
#25734=CARTESIAN_POINT('Ctrl Pts',(1.98415376933049,-0.216804755553798,
13.2652325191741));
#25735=CARTESIAN_POINT('Ctrl Pts',(1.98929626850988,-0.147403930044804,
13.2696865578921));
#25736=CARTESIAN_POINT('Ctrl Pts',(1.99443103771401,-0.0781074247595321,
13.2741339014978));
#25737=CARTESIAN_POINT('Ctrl Pts',(1.995948596023,-0.00843449825290857,
13.2785812451036));
#25738=CARTESIAN_POINT('Ctrl Pts',(1.99381076884887,0.0612060497197463,
13.2830285887093));
#25739=CARTESIAN_POINT('Ctrl Pts',(1.99167546195322,0.130764498644711,13.2874706893541));
#25740=CARTESIAN_POINT('Ctrl Pts',(1.98589334338283,0.200290157879424,13.2919127899989));
#25741=CARTESIAN_POINT('Ctrl Pts',(1.97647824293634,0.269372080400441,13.2963548906437));
#25742=CARTESIAN_POINT('Ctrl Pts',(1.96706908157691,0.338410425738792,13.3007941891917));
#25743=CARTESIAN_POINT('Ctrl Pts',(1.95403155050615,0.407005105691801,13.3052334877398));
#25744=CARTESIAN_POINT('Ctrl Pts',(1.93743136664856,0.474749683545216,13.3096727862878));
#25745=CARTESIAN_POINT('Ctrl Pts',(1.92083601347846,0.542474547587803,13.3141107929909));
#25746=CARTESIAN_POINT('Ctrl Pts',(1.90068018206833,0.609349325371707,13.3185487996939));
#25747=CARTESIAN_POINT('Ctrl Pts',(1.87708044787254,0.674978929089375,13.322986806397));
#25748=CARTESIAN_POINT('Ctrl Pts',(1.85347956223567,0.740611734903338,13.3274250296323));
#25749=CARTESIAN_POINT('Ctrl Pts',(1.82643460811985,0.804998786162914,13.3318632528676));
#25750=CARTESIAN_POINT('Ctrl Pts',(1.79611106947771,0.867762979505146,13.3363014761029));
#25751=CARTESIAN_POINT('Ctrl Pts',(1.76575540639279,0.930593664583754,13.3407444011459));
#25752=CARTESIAN_POINT('Ctrl Pts',(1.73211443963886,0.991797618537426,13.3451873261889));
#25753=CARTESIAN_POINT('Ctrl Pts',(1.69540016767943,1.05102132896177,13.349630251232));
#25754=CARTESIAN_POINT('Ctrl Pts',(1.65866446408825,1.11027961070361,13.3540757697932));
#25755=CARTESIAN_POINT('Ctrl Pts',(1.61885216401748,1.16755494602156,13.3585212883545));
#25756=CARTESIAN_POINT('Ctrl Pts',(1.57621767231628,1.22252419688849,13.3629668069157));
#25757=CARTESIAN_POINT('Ctrl Pts',(1.53350878223693,1.27758937063264,13.367420083031));
#25758=CARTESIAN_POINT('Ctrl Pts',(1.48796818962266,1.33034005640665,13.3718733591462));
#25759=CARTESIAN_POINT('Ctrl Pts',(1.43988896155922,1.38048808067288,13.3763266352614));
#25760=CARTESIAN_POINT('Ctrl Pts',(1.4141439175352,1.40734090557158,13.3787112365593));
#25761=CARTESIAN_POINT('Ctrl Pts',(1.38767157722307,1.43344812795739,13.3810958378571));
#25762=CARTESIAN_POINT('Ctrl Pts',(1.3605207661014,1.45877030663051,13.3834804391549));
#25763=CARTESIAN_POINT('Ctrl Pts',(1.3098075655041,1.50606792587494,13.3879344778729));
#25764=CARTESIAN_POINT('Ctrl Pts',(1.2565245851602,1.55081154537459,13.3923885165908));
#25765=CARTESIAN_POINT('Ctrl Pts',(1.20095952898562,1.59270956933103,13.3968425553088));
#25766=CARTESIAN_POINT('Ctrl Pts',(1.14547799572374,1.63454461404768,13.4012898989146));
#25767=CARTESIAN_POINT('Ctrl Pts',(1.08772158265844,1.67354226040037,13.4057372425203));
#25768=CARTESIAN_POINT('Ctrl Pts',(1.02801332308524,1.70944908378672,13.4101845861261));
#25769=CARTESIAN_POINT('Ctrl Pts',(0.968375453412641,1.74531357671917,13.4146266867709));
#25770=CARTESIAN_POINT('Ctrl Pts',(0.906790724876314,1.77809423257428,13.4190687874157));
#25771=CARTESIAN_POINT('Ctrl Pts',(0.84361213189459,1.80758018727255,13.4235108880605));
#25772=CARTESIAN_POINT('Ctrl Pts',(0.780473392249227,1.83704754209996,13.4279501866085));
#25773=CARTESIAN_POINT('Ctrl Pts',(0.715743225269266,1.86322411210079,13.4323894851565));
#25774=CARTESIAN_POINT('Ctrl Pts',(0.649798925601301,1.88594509962178,13.4368287837045));
#25775=CARTESIAN_POINT('Ctrl Pts',(0.583873815859491,1.9086594752889,13.4412667904076));
#25776=CARTESIAN_POINT('Ctrl Pts',(0.51673573743669,1.9279201053192,13.4457047971106));
#25777=CARTESIAN_POINT('Ctrl Pts',(0.448779978711364,1.94361109618355,13.4501428038137));
#25778=CARTESIAN_POINT('Ctrl Pts',(0.38082090439542,1.95930285261808,13.454581027049));
#25779=CARTESIAN_POINT('Ctrl Pts',(0.312044548118415,1.97142451629559,13.4590192502843));
#25780=CARTESIAN_POINT('Ctrl Pts',(0.242857557342055,1.97991105086614,13.4634574735196));
#25781=CARTESIAN_POINT('Ctrl Pts',(0.173597270584371,1.9884065759835,13.4679003985627));
#25782=CARTESIAN_POINT('Ctrl Pts',(0.103925967932314,1.99325922582369,13.4723433236057));
#25783=CARTESIAN_POINT('Ctrl Pts',(0.0342556460789304,1.99445584388618,
13.4767862486487));
#25784=CARTESIAN_POINT('Ctrl Pts',(-0.0354553452089624,1.99565316046387,
13.48123176721));
#25785=CARTESIAN_POINT('Ctrl Pts',(-0.105164865154026,1.99319021472127,
13.4856772857712));
#25786=CARTESIAN_POINT('Ctrl Pts',(-0.174463495229841,1.98710594869327,
13.4901228043325));
#25787=CARTESIAN_POINT('Ctrl Pts',(-0.243883053349606,1.98101106545121,
13.4945760804477));
#25788=CARTESIAN_POINT('Ctrl Pts',(-0.312889805594576,1.97128231579446,
13.4990293565629));
#25789=CARTESIAN_POINT('Ctrl Pts',(-0.381082797903004,1.95801007751299,
13.5034826326782));
#25790=CARTESIAN_POINT('Ctrl Pts',(-0.417598184273228,1.95090317558011,
13.505867233976));
#25791=CARTESIAN_POINT('Ctrl Pts',(-0.453880466547818,1.94278111578831,
13.5082518352738));
#25792=CARTESIAN_POINT('Ctrl Pts',(-0.489870049548812,1.93366359459319,
13.5106364365716));
#25793=CARTESIAN_POINT('Ctrl Pts',(-0.557092606324624,1.91663358104241,
13.5150904752896));
#25794=CARTESIAN_POINT('Ctrl Pts',(-0.623559177798799,1.8960602401195,13.5195445140076));
#25795=CARTESIAN_POINT('Ctrl Pts',(-0.688868836301772,1.87202758763653,
13.5239985527256));
#25796=CARTESIAN_POINT('Ctrl Pts',(-0.754080324240724,1.84803105996424,
13.5284458963313));
#25797=CARTESIAN_POINT('Ctrl Pts',(-0.818137895034203,1.8205857088959,13.5328932399371));
#25798=CARTESIAN_POINT('Ctrl Pts',(-0.880653585988228,1.78982592002297,
13.5373405835429));
#25799=CARTESIAN_POINT('Ctrl Pts',(-0.943095577368579,1.75910239377934,
13.5417826841876));
#25800=CARTESIAN_POINT('Ctrl Pts',(-1.00399886197858,1.72507240537356,13.5462247848324));
#25801=CARTESIAN_POINT('Ctrl Pts',(-1.06299503889724,1.6879185732078,13.5506668854772));
#25802=CARTESIAN_POINT('Ctrl Pts',(-1.12195400076611,1.65078817784398,13.5551061840252));
#25803=CARTESIAN_POINT('Ctrl Pts',(-1.17900782814711,1.61053810808701,13.5595454825733));
#25804=CARTESIAN_POINT('Ctrl Pts',(-1.2338136943822,1.56739635384766,13.5639847811213));
#25805=CARTESIAN_POINT('Ctrl Pts',(-1.28860361199807,1.52426715394708,13.5684227878243));
#25806=CARTESIAN_POINT('Ctrl Pts',(-1.34114648260044,1.47824824270036,13.5728607945274));
#25807=CARTESIAN_POINT('Ctrl Pts',(-1.39113085402196,1.42960921565585,13.5772988012305));
#25808=CARTESIAN_POINT('Ctrl Pts',(-1.44111766420226,1.38096781549248,13.5817370244658));
#25809=CARTESIAN_POINT('Ctrl Pts',(-1.48854537817484,1.32970638886034,13.5861752477011));
#25810=CARTESIAN_POINT('Ctrl Pts',(-1.53313915238611,1.27613161622177,13.5906134709364));
#25811=CARTESIAN_POINT('Ctrl Pts',(-1.57778016877996,1.22250008702391,13.5950563959794));
#25812=CARTESIAN_POINT('Ctrl Pts',(-1.61958093925338,1.16655069729056,13.5994993210224));
#25813=CARTESIAN_POINT('Ctrl Pts',(-1.65830734248925,1.10862271325561,13.6039422460654));
#25814=CARTESIAN_POINT('Ctrl Pts',(-1.69705635192068,1.05066091427206,13.6083877646267));
#25815=CARTESIAN_POINT('Ctrl Pts',(-1.73272717166764,0.990718642949719,
13.6128332831879));
#25816=CARTESIAN_POINT('Ctrl Pts',(-1.76513087849859,0.929161204673771,
13.6172788017492));
#25817=CARTESIAN_POINT('Ctrl Pts',(-1.79759113070251,0.867496346949635,
13.6217320778644));
#25818=CARTESIAN_POINT('Ctrl Pts',(-1.82677268438971,0.804211140544934,
13.6261853539796));
#25819=CARTESIAN_POINT('Ctrl Pts',(-1.85253444408813,0.739691622209618,
13.6306386300949));
#25820=CARTESIAN_POINT('Ctrl Pts',(-1.86632912558135,0.70514327551471,13.6330232313927));
#25821=CARTESIAN_POINT('Ctrl Pts',(-1.87914410014879,0.670241294351013,
13.6354078326905));
#25822=CARTESIAN_POINT('Ctrl Pts',(-1.89096366219834,0.635046447707129,
13.6377924339883));
#25823=CARTESIAN_POINT('Ctrl Pts',(-1.91713820822316,0.557107085025591,
13.6430731589559));
#25824=CARTESIAN_POINT('Ctrl Pts',(-1.93851310398558,0.477479571807927,
13.6483538839235));
#25825=CARTESIAN_POINT('Ctrl Pts',(-1.95490359300059,0.396710857644933,
13.653634608891));
#25826=CARTESIAN_POINT('Ctrl Pts',(-1.97111438693516,0.316827641198072,
13.6588574392895));
#25827=CARTESIAN_POINT('Ctrl Pts',(-1.98244939795434,0.23582820185453,13.6640802696881));
#25828=CARTESIAN_POINT('Ctrl Pts',(-1.98877616824338,0.154262487751171,
13.6693031000866));
#25829=CARTESIAN_POINT('Ctrl Pts',(-1.99270989180756,0.103548307065135,
13.6725504395776));
#25830=CARTESIAN_POINT('Ctrl Pts',(-1.99470842578248,0.05261562048858,13.6757977790687));
#25831=CARTESIAN_POINT('Ctrl Pts',(-1.99474935791997,0.00160049301082166,
13.6790451185598));
#25832=CARTESIAN_POINT('',(-1.99423738866044,-0.00182902399065958,12.0790454206247));
#25833=CARTESIAN_POINT('Ctrl Pts',(-1.99423738866044,-0.00182902399065958,
12.0790454206247));
#25834=CARTESIAN_POINT('Ctrl Pts',(-1.99577709645304,-0.173571656520854,
12.0900037687456));
#25835=CARTESIAN_POINT('Ctrl Pts',(-1.89678413975083,-1.00784194773067,
12.1433474493388));
#25836=CARTESIAN_POINT('Ctrl Pts',(-0.728288010713249,-2.24331894452348,
12.2390764624042));
#25837=CARTESIAN_POINT('Ctrl Pts',(1.49178352251778,-1.82687307587338,12.366232459821));
#25838=CARTESIAN_POINT('Ctrl Pts',(2.34362655358403,0.265137494033562,12.4933884572377));
#25839=CARTESIAN_POINT('Ctrl Pts',(1.04595083702944,2.11397023629094,12.6205444546545));
#25840=CARTESIAN_POINT('Ctrl Pts',(-1.21104620563245,2.02391956392289,12.7477004520712));
#25841=CARTESIAN_POINT('Ctrl Pts',(-1.98780196605619,0.704986800798777,
12.8338673400546));
#25842=CARTESIAN_POINT('Ctrl Pts',(-1.99799837878425,0.0221817113925817,
12.8776488955658));
#25843=CARTESIAN_POINT('Ctrl Pts',(-1.99793808332185,0.000404756782470808,
12.8790451186048));
#25844=CARTESIAN_POINT('',(-1.99474936733483,0.00158871561359909,10.4790451186048));
#25845=CARTESIAN_POINT('Ctrl Pts',(-1.99474918095163,-0.00180764841896022,
12.0793396996528));
#25846=CARTESIAN_POINT('Ctrl Pts',(-1.99484885862249,0.108187165960091,
12.0729507633111));
#25847=CARTESIAN_POINT('Ctrl Pts',(-1.98585074754498,0.217993308813224,
12.0665054587627));
#25848=CARTESIAN_POINT('Ctrl Pts',(-1.96280285823564,0.3569073674302,12.0578927663831));
#25849=CARTESIAN_POINT('Ctrl Pts',(-1.95705291046282,0.387197204379771,
12.0559873421261));
#25850=CARTESIAN_POINT('Ctrl Pts',(-1.94891810280673,0.425218408213222,
12.0535559201257));
#25851=CARTESIAN_POINT('Ctrl Pts',(-1.94718488269249,0.433086014217266,
12.053050642673));
#25852=CARTESIAN_POINT('Ctrl Pts',(-1.94419256405425,0.44628788228874,12.0521990725554));
#25853=CARTESIAN_POINT('Ctrl Pts',(-1.94295904408368,0.451627891129366,
12.0518535979334));
#25854=CARTESIAN_POINT('Ctrl Pts',(-1.9404831389815,0.462148385791333,12.0511709161668));
#25855=CARTESIAN_POINT('Ctrl Pts',(-1.93924197591684,0.467329114334702,
12.0508337507229));
#25856=CARTESIAN_POINT('Ctrl Pts',(-1.9368325101669,0.477211547173679,12.0501886871813));
#25857=CARTESIAN_POINT('Ctrl Pts',(-1.93566780133287,0.481914095454843,
12.0498809070156));
#25858=CARTESIAN_POINT('Ctrl Pts',(-1.93296260807407,0.492668361670484,
12.0491751271378));
#25859=CARTESIAN_POINT('Ctrl Pts',(-1.93141081939197,0.498717158390616,
12.0487767645773));
#25860=CARTESIAN_POINT('Ctrl Pts',(-1.92654025131116,0.517338680208813,
12.0475460302998));
#25861=CARTESIAN_POINT('Ctrl Pts',(-1.92312696895886,0.529886117870888,
12.0467106076777));
#25862=CARTESIAN_POINT('Ctrl Pts',(-1.88441590732639,0.66688749837837,12.0375200092384));
#25863=CARTESIAN_POINT('Ctrl Pts',(-1.83722141552458,0.78763443173628,12.0287643231951));
#25864=CARTESIAN_POINT('Ctrl Pts',(-1.74787812498756,0.963629234417369,
12.015077962897));
#25865=CARTESIAN_POINT('Ctrl Pts',(-1.71398649726138,1.02269705494905,12.0103152752113));
#25866=CARTESIAN_POINT('Ctrl Pts',(-1.63085581147103,1.15180162108369,11.9996264039091));
#25867=CARTESIAN_POINT('Ctrl Pts',(-1.57998942645046,1.22064495557221,11.9937244327594));
#25868=CARTESIAN_POINT('Ctrl Pts',(-1.51342462071226,1.2995722040838,11.9868833827804));
#25869=CARTESIAN_POINT('Ctrl Pts',(-1.50181187290085,1.31297492286934,11.985719054412));
#25870=CARTESIAN_POINT('Ctrl Pts',(-1.48667898069485,1.32997685893993,11.9842406060038));
#25871=CARTESIAN_POINT('Ctrl Pts',(-1.48332227391515,1.33371956197636,11.983915057994));
#25872=CARTESIAN_POINT('Ctrl Pts',(-1.47793357859478,1.33968240897271,11.9833963081703));
#25873=CARTESIAN_POINT('Ctrl Pts',(-1.47591068107915,1.34191068310096,11.983202434957));
#25874=CARTESIAN_POINT('Ctrl Pts',(-1.4720546105342,1.34613897741245,11.982834524539));
#25875=CARTESIAN_POINT('Ctrl Pts',(-1.47022242289288,1.34813981107635,11.9826604207673));
#25876=CARTESIAN_POINT('Ctrl Pts',(-1.46600337344847,1.3527283779938,11.9822611130898));
#25877=CARTESIAN_POINT('Ctrl Pts',(-1.46361374126741,1.35531353288827,11.9820361232395));
#25878=CARTESIAN_POINT('Ctrl Pts',(-1.45618922870233,1.36330299221135,11.9813406641503));
#25879=CARTESIAN_POINT('Ctrl Pts',(-1.45113109457436,1.36868574509045,11.9808719337115));
#25880=CARTESIAN_POINT('Ctrl Pts',(-1.35911923888734,1.46551922219162,11.9724336906515));
#25881=CARTESIAN_POINT('Ctrl Pts',(-1.26369533533535,1.54855948118669,11.9650908535941));
#25882=CARTESIAN_POINT('Ctrl Pts',(-1.07027612907576,1.68700858150156,11.9512871450542));
#25883=CARTESIAN_POINT('Ctrl Pts',(-0.974215785000916,1.74424497553258,
11.9448441838547));
#25884=CARTESIAN_POINT('Ctrl Pts',(-0.818198653931384,1.82027873847391,
11.934436573094));
#25885=CARTESIAN_POINT('Ctrl Pts',(-0.761293234419289,1.84480219602976,
11.9306541643618));
#25886=CARTESIAN_POINT('Ctrl Pts',(-0.693291119944838,1.870425186837,11.9261076584501));
#25887=CARTESIAN_POINT('Ctrl Pts',(-0.683208600509569,1.87413152086904,
11.9254329366476));
#25888=CARTESIAN_POINT('Ctrl Pts',(-0.668587338317781,1.87937262979526,
11.9244533993587));
#25889=CARTESIAN_POINT('Ctrl Pts',(-0.664072108739256,1.88097281860383,
11.9241507576373));
#25890=CARTESIAN_POINT('Ctrl Pts',(-0.654941558998126,1.88417169431438,
11.9235384454758));
#25891=CARTESIAN_POINT('Ctrl Pts',(-0.650326045196499,1.88576972443685,
11.9232287557767));
#25892=CARTESIAN_POINT('Ctrl Pts',(-0.641373417822971,1.88883261768678,
11.9226277183401));
#25893=CARTESIAN_POINT('Ctrl Pts',(-0.637037035344169,1.89029953545775,
11.9223364408747));
#25894=CARTESIAN_POINT('Ctrl Pts',(-0.625517845486112,1.89415212473706,
11.9215622635058));
#25895=CARTESIAN_POINT('Ctrl Pts',(-0.618326498225142,1.89651184695599,
11.9210785111946));
#25896=CARTESIAN_POINT('Ctrl Pts',(-0.592670503133408,1.90476900416666,
11.9193509937921));
#25897=CARTESIAN_POINT('Ctrl Pts',(-0.574134017130108,1.91043800495356,
11.9180997712826));
#25898=CARTESIAN_POINT('Ctrl Pts',(-0.424621203735764,1.95379094618723,
11.9079796719291));
#25899=CARTESIAN_POINT('Ctrl Pts',(-0.290203918461033,1.97822417123613,
11.8986726693985));
#25900=CARTESIAN_POINT('Ctrl Pts',(-0.0168923781969079,1.99943906768614,
11.8795916941514));
#25901=CARTESIAN_POINT('Ctrl Pts',(0.121331746008538,1.99582718770227,11.8698700086057));
#25902=CARTESIAN_POINT('Ctrl Pts',(0.274380916292036,1.97585746830651,11.8596518898124));
#25903=CARTESIAN_POINT('Ctrl Pts',(0.29065003984629,1.97352988810661,11.8585731054541));
#25904=CARTESIAN_POINT('Ctrl Pts',(0.312062161289376,1.9701959746685,11.8571646959501));
#25905=CARTESIAN_POINT('Ctrl Pts',(0.317232035378616,1.969370155238,11.8568255201808));
#25906=CARTESIAN_POINT('Ctrl Pts',(0.325437880504499,1.96802622772115,11.8562886277261));
#25907=CARTESIAN_POINT('Ctrl Pts',(0.328475960789748,1.9675214333177,11.8560901707426));
#25908=CARTESIAN_POINT('Ctrl Pts',(0.334173703317038,1.966561155817,11.8557185899691));
#25909=CARTESIAN_POINT('Ctrl Pts',(0.336833579628456,1.9661073173413,11.8555453781047));
#25910=CARTESIAN_POINT('Ctrl Pts',(0.342900167127311,1.96505954004727,11.8551508892476));
#25911=CARTESIAN_POINT('Ctrl Pts',(0.346306253033582,1.9644621401539,11.8549298114993));
#25912=CARTESIAN_POINT('Ctrl Pts',(0.35674117106134,1.96260395719676,11.8542537189989));
#25913=CARTESIAN_POINT('Ctrl Pts',(0.363764897181355,1.9613142683493,11.8538003173172));
#25914=CARTESIAN_POINT('Ctrl Pts',(0.419662547128181,1.95073979738671,11.8502042266845));
#25915=CARTESIAN_POINT('Ctrl Pts',(0.468185222418544,1.93966645716922,11.8471572666069));
#25916=CARTESIAN_POINT('Ctrl Pts',(0.533914062706573,1.92205563153123,11.8430699621467));
#25917=CARTESIAN_POINT('Ctrl Pts',(0.551515154688451,1.91707932606761,11.8419794650533));
#25918=CARTESIAN_POINT('Ctrl Pts',(0.722686369746059,1.86613199322953,11.8313921624243));
#25919=CARTESIAN_POINT('Ctrl Pts',(0.870255180355367,1.80204996139328,11.8223554016313));
#25920=CARTESIAN_POINT('Ctrl Pts',(1.04955047029234,1.69697606776551,11.8099661025321));
#25921=CARTESIAN_POINT('Ctrl Pts',(1.08965952079484,1.67150399284907,11.807097049638));
#25922=CARTESIAN_POINT('Ctrl Pts',(1.15261526627158,1.62829316305592,11.8024037375847));
#25923=CARTESIAN_POINT('Ctrl Pts',(1.17605301515939,1.61144647708154,11.8006118901766));
#25924=CARTESIAN_POINT('Ctrl Pts',(1.20573611074448,1.58911818799078,11.7982804893771));
#25925=CARTESIAN_POINT('Ctrl Pts',(1.2123249315063,1.58409735851978,11.7977589498346));
#25926=CARTESIAN_POINT('Ctrl Pts',(1.223139054096,1.57574976912173,11.7968961788712));
#25927=CARTESIAN_POINT('Ctrl Pts',(1.22738256050131,1.57244666993689,11.7965558840395));
#25928=CARTESIAN_POINT('Ctrl Pts',(1.23541469885217,1.56614221766,11.7959084306857));
#25929=CARTESIAN_POINT('Ctrl Pts',(1.23920588588474,1.56314416986726,11.7956014053222));
#25930=CARTESIAN_POINT('Ctrl Pts',(1.24779739949618,1.55629915329115,11.7949023588638));
#25931=CARTESIAN_POINT('Ctrl Pts',(1.2525908840936,1.55244371247677,11.7945099994814));
#25932=CARTESIAN_POINT('Ctrl Pts',(1.26709444312639,1.54066747193688,11.7933156619083));
#25933=CARTESIAN_POINT('Ctrl Pts',(1.27674763709945,1.5326774109821,11.7925108884855));
#25934=CARTESIAN_POINT('Ctrl Pts',(1.40661048967167,1.42311023347928,11.7815480588068));
#25935=CARTESIAN_POINT('Ctrl Pts',(1.51443727901229,1.30776720970524,11.7707790256885));
#25936=CARTESIAN_POINT('Ctrl Pts',(1.66124710740046,1.10792779327813,11.7534928249695));
#25937=CARTESIAN_POINT('Ctrl Pts',(1.709878420532,1.03129191348939,11.7471429084596));
#25938=CARTESIAN_POINT('Ctrl Pts',(1.76945902784338,0.921528059331686,11.7386221069192));
#25939=CARTESIAN_POINT('Ctrl Pts',(1.7850124510975,0.891027528080388,11.7363122646895));
#25940=CARTESIAN_POINT('Ctrl Pts',(1.80802969927368,0.842865780320253,11.7327702042771));
#25941=CARTESIAN_POINT('Ctrl Pts',(1.81603658232634,0.825472783064892,11.7315119089266));
#25942=CARTESIAN_POINT('Ctrl Pts',(1.82584260359814,0.803338020924796,11.7299392476661));
#25943=CARTESIAN_POINT('Ctrl Pts',(1.8278754551799,0.798701765799615,11.7296114200392));
#25944=CARTESIAN_POINT('Ctrl Pts',(1.83109177052213,0.791289829664729,11.7290898941046));
#25945=CARTESIAN_POINT('Ctrl Pts',(1.83228660706276,0.788519154162068,11.7288955119525));
#25946=CARTESIAN_POINT('Ctrl Pts',(1.83454303716102,0.783253954178378,11.7285272190856));
#25947=CARTESIAN_POINT('Ctrl Pts',(1.83560581895316,0.780760007583391,11.7283532393672));
#25948=CARTESIAN_POINT('Ctrl Pts',(1.8380313631467,0.775035845378071,11.7279549782062));
#25949=CARTESIAN_POINT('Ctrl Pts',(1.8393906948618,0.771804201625543,11.7277309070036));
#25950=CARTESIAN_POINT('Ctrl Pts',(1.84366297158519,0.761571994084027,11.7270238276549));
#25951=CARTESIAN_POINT('Ctrl Pts',(1.84654456841583,0.754558292146722,11.7265426841799));
#25952=CARTESIAN_POINT('Ctrl Pts',(1.89503001638701,0.634605202873113,11.7183710696226));
#25953=CARTESIAN_POINT('Ctrl Pts',(1.93024327377328,0.517719228208718,11.7112636517435));
#25954=CARTESIAN_POINT('Ctrl Pts',(1.97464031991498,0.299868793151865,11.6983549000612));
#25955=CARTESIAN_POINT('Ctrl Pts',(1.98723742444042,0.20002991003316,11.6925606543961));
#25956=CARTESIAN_POINT('Ctrl Pts',(1.99480471555322,0.0487733192826281,
11.6835581582014));
#25957=CARTESIAN_POINT('Ctrl Pts',(1.99539952188995,-0.00220061530919844,
11.6804879050253));
#25958=CARTESIAN_POINT('Ctrl Pts',(1.99323007481769,-0.0836096056814195,
11.6754888512549));
#25959=CARTESIAN_POINT('Ctrl Pts',(1.99171977314159,-0.114056501075558,
11.6735979386913));
#25960=CARTESIAN_POINT('Ctrl Pts',(1.98888313599916,-0.153124040179684,
11.6711397086736));
#25961=CARTESIAN_POINT('Ctrl Pts',(1.98819709542604,-0.161788152317992,
11.6705925240673));
#25962=CARTESIAN_POINT('Ctrl Pts',(1.98699882125027,-0.175760295189872,
11.6697067482134));
#25963=CARTESIAN_POINT('Ctrl Pts',(1.98652187981424,-0.181071304003883,
11.6693692678851));
#25964=CARTESIAN_POINT('Ctrl Pts',(1.98557110693201,-0.191202511456369,
11.6687239714021));
#25965=CARTESIAN_POINT('Ctrl Pts',(1.98510100314457,-0.196023028506678,
11.6684162747333));
#25966=CARTESIAN_POINT('Ctrl Pts',(1.98398559089455,-0.207044950158387,
11.6677112089154));
#25967=CARTESIAN_POINT('Ctrl Pts',(1.98332875655866,-0.213245112984284,
11.6673134795132));
#25968=CARTESIAN_POINT('Ctrl Pts',(1.98121790476579,-0.232316505682064,
11.6660866130978));
#25969=CARTESIAN_POINT('Ctrl Pts',(1.97966759867766,-0.245176529389799,
11.6652544528902));
#25970=CARTESIAN_POINT('Ctrl Pts',(1.96337726564101,-0.370058765795065,
11.6571246703258));
#25971=CARTESIAN_POINT('Ctrl Pts',(1.93927252087176,-0.480632804230657,
11.6495261565314));
#25972=CARTESIAN_POINT('Ctrl Pts',(1.85816798075956,-0.743276750710874,
11.6305658696391));
#25973=CARTESIAN_POINT('Ctrl Pts',(1.79173053639902,-0.891600260354994,
11.6190425211045));
#25974=CARTESIAN_POINT('Ctrl Pts',(1.69517360110864,-1.05168433240267,11.6065568580152));
#25975=CARTESIAN_POINT('Ctrl Pts',(1.68184939079497,-1.07286357180088,11.6049052939087));
#25976=CARTESIAN_POINT('Ctrl Pts',(1.66509997765402,-1.09840800806227,11.6029189514031));
#25977=CARTESIAN_POINT('Ctrl Pts',(1.66205122821783,-1.10301577699605,11.6025608780701));
#25978=CARTESIAN_POINT('Ctrl Pts',(1.65725094942257,-1.1102056508084,11.6020025797066));
#25979=CARTESIAN_POINT('Ctrl Pts',(1.6555124691493,-1.11279637008216,11.6018014970358));
#25980=CARTESIAN_POINT('Ctrl Pts',(1.65226208322431,-1.11761568668576,11.6014276193161));
#25981=CARTESIAN_POINT('Ctrl Pts',(1.65075175860802,-1.11984527787244,11.6012547242442));
#25982=CARTESIAN_POINT('Ctrl Pts',(1.64732505077487,-1.12488190097569,11.6008643175221));
#25983=CARTESIAN_POINT('Ctrl Pts',(1.64540601097656,-1.12768709024932,11.6006469891924));
#25984=CARTESIAN_POINT('Ctrl Pts',(1.63972512704918,-1.13594584488514,11.6000074401708));
#25985=CARTESIAN_POINT('Ctrl Pts',(1.63594322667921,-1.14138565649322,11.5995865575342));
#25986=CARTESIAN_POINT('Ctrl Pts',(1.60968159344546,-1.17876119122882,11.5966965886775));
#25987=CARTESIAN_POINT('Ctrl Pts',(1.58629353090542,-1.21005210789473,11.5942862019571));
#25988=CARTESIAN_POINT('Ctrl Pts',(1.5565788281996,-1.2474637817082,11.5913883961672));
#25989=CARTESIAN_POINT('Ctrl Pts',(1.55111300363812,-1.2542535585753,11.5908618172267));
#25990=CARTESIAN_POINT('Ctrl Pts',(1.52933401218317,-1.28094782706485,11.5887879607823));
#25991=CARTESIAN_POINT('Ctrl Pts',(1.51268034270638,-1.30057222911857,11.587255377766));
#25992=CARTESIAN_POINT('Ctrl Pts',(1.46300240240858,-1.35686632934202,11.5828174953894));
#25993=CARTESIAN_POINT('Ctrl Pts',(1.42899115602662,-1.39264024437269,11.5799437707428));
#25994=CARTESIAN_POINT('Ctrl Pts',(1.32172972569539,-1.49738911145848,11.5712385953718));
#25995=CARTESIAN_POINT('Ctrl Pts',(1.24456184455973,-1.56211660966999,11.5654396830185));
#25996=CARTESIAN_POINT('Ctrl Pts',(1.121348002591,-1.65051953840637,11.5564260630053));
#25997=CARTESIAN_POINT('Ctrl Pts',(1.07872483074414,-1.6786864598584,11.5533493281785));
#25998=CARTESIAN_POINT('Ctrl Pts',(1.0089717614848,-1.72102749624539,11.5483406427772));
#25999=CARTESIAN_POINT('Ctrl Pts',(0.982514316992654,-1.73626758229258,
11.5464467686824));
#26000=CARTESIAN_POINT('Ctrl Pts',(0.948085605967691,-1.75506036042423,
11.5439852053992));
#26001=CARTESIAN_POINT('Ctrl Pts',(0.940425514347337,-1.75917680552066,
11.5434377172538));
#26002=CARTESIAN_POINT('Ctrl Pts',(0.928024356344151,-1.76573690073081,
11.5425515686164));
#26003=CARTESIAN_POINT('Ctrl Pts',(0.923299919687577,-1.76821188378936,
11.5422140207621));
#26004=CARTESIAN_POINT('Ctrl Pts',(0.914266569797192,-1.77289809573383,
11.5415686740953));
#26005=CARTESIAN_POINT('Ctrl Pts',(0.909959411952963,-1.77511264048898,
11.5412609951013));
#26006=CARTESIAN_POINT('Ctrl Pts',(0.900090879921511,-1.78014123542618,
11.5405560812922));
#26007=CARTESIAN_POINT('Ctrl Pts',(0.894524317425016,-1.78294493865071,
11.5401584867767));
#26008=CARTESIAN_POINT('Ctrl Pts',(0.877358585304075,-1.79149015648187,
11.538932443463));
#26009=CARTESIAN_POINT('Ctrl Pts',(0.865716787778558,-1.79714481837445,
11.5381009773507));
#26010=CARTESIAN_POINT('Ctrl Pts',(0.752071778063161,-1.85098405786124,
11.5299833723584));
#26011=CARTESIAN_POINT('Ctrl Pts',(0.646227564069054,-1.89053853113174,
11.5223973190649));
#26012=CARTESIAN_POINT('Ctrl Pts',(0.381544594245775,-1.96461714860328,
11.5034402644728));
#26013=CARTESIAN_POINT('Ctrl Pts',(0.220726094123614,-1.98911476078211,
11.4919058024667));
#26014=CARTESIAN_POINT('Ctrl Pts',(0.0336692489413088,-1.99462323167431,
11.4794070491161));
#26015=CARTESIAN_POINT('Ctrl Pts',(0.00860918121163235,-1.9948888393611,
11.4777528251775));
#26016=CARTESIAN_POINT('Ctrl Pts',(-0.0219781157949418,-1.99463657845007,
11.475763720997));
#26017=CARTESIAN_POINT('Ctrl Pts',(-0.0275054673085827,-1.99456801556112,
11.4754054707219));
#26018=CARTESIAN_POINT('Ctrl Pts',(-0.0361526363513712,-1.99442480105054,
11.4748469576618));
#26019=CARTESIAN_POINT('Ctrl Pts',(-0.0392726317413574,-1.99436580418058,
11.4746458361718));
#26020=CARTESIAN_POINT('Ctrl Pts',(-0.0450848360069074,-1.99424225509335,
11.4742719236012));
#26021=CARTESIAN_POINT('Ctrl Pts',(-0.047777024582177,-1.99417957328167,
11.4740990323226));
#26022=CARTESIAN_POINT('Ctrl Pts',(-0.0538659733519217,-1.99402546757891,
11.4737086818615));
#26023=CARTESIAN_POINT('Ctrl Pts',(-0.0572626227174797,-1.99393081647717,
11.4734914057772));
#26024=CARTESIAN_POINT('Ctrl Pts',(-0.0672772751470178,-1.9936261365331,
11.4728521519743));
#26025=CARTESIAN_POINT('Ctrl Pts',(-0.0738945744111544,-1.99339183274748,
11.4724315104659));
#26026=CARTESIAN_POINT('Ctrl Pts',(-0.119459882573349,-1.99155125804546,
11.4695463838337));
#26027=CARTESIAN_POINT('Ctrl Pts',(-0.158357764620448,-1.98883643987945,
11.46714037629));
#26028=CARTESIAN_POINT('Ctrl Pts',(-0.205693685456895,-1.98413490324016,
11.4642549602885));
#26029=CARTESIAN_POINT('Ctrl Pts',(-0.214227829298461,-1.98323161724602,
11.4637364464589));
#26030=CARTESIAN_POINT('Ctrl Pts',(-0.29674049139646,-1.97395933870372,
11.4587373372729));
#26031=CARTESIAN_POINT('Ctrl Pts',(-0.370206653177138,-1.9615093424676,
11.4543949416884));
#26032=CARTESIAN_POINT('Ctrl Pts',(-0.541163907989573,-1.92258791784375,
11.4442132612495));
#26033=CARTESIAN_POINT('Ctrl Pts',(-0.637676655607367,-1.89276782948434,
11.4383990057976));
#26034=CARTESIAN_POINT('Ctrl Pts',(-0.779373910791746,-1.83691321503152,
11.4293487666133));
#26035=CARTESIAN_POINT('Ctrl Pts',(-0.826481307962906,-1.81620535460337,
11.426250667406));
#26036=CARTESIAN_POINT('Ctrl Pts',(-0.900330014255933,-1.78027393962846,
11.4212102487798));
#26037=CARTESIAN_POINT('Ctrl Pts',(-0.927611932134093,-1.76621215535936,
11.4193066306862));
#26038=CARTESIAN_POINT('Ctrl Pts',(-0.962207310700516,-1.74735816423032,
11.4168341027166));
#26039=CARTESIAN_POINT('Ctrl Pts',(-0.969829621235627,-1.74313911228063,
11.4162856191016));
#26040=CARTESIAN_POINT('Ctrl Pts',(-0.982076374868853,-1.73625517721604,
11.4153982478786));
#26041=CARTESIAN_POINT('Ctrl Pts',(-0.986718245355617,-1.73362139749837,
11.4150604785516));
#26042=CARTESIAN_POINT('Ctrl Pts',(-0.995551402419267,-1.7285625286114,
11.4144149667268));
#26043=CARTESIAN_POINT('Ctrl Pts',(-0.999744543701183,-1.72614074073892,
11.4141073451367));
#26044=CARTESIAN_POINT('Ctrl Pts',(-1.00930877618424,-1.72057028901564,
11.4134029271462));
#26045=CARTESIAN_POINT('Ctrl Pts',(-1.01467400655014,-1.71741171071603,
11.4130057728487));
#26046=CARTESIAN_POINT('Ctrl Pts',(-1.03111664143485,-1.70762778092399,
11.4117824136283));
#26047=CARTESIAN_POINT('Ctrl Pts',(-1.04214442285568,-1.70092009080897,
11.4109532105261));
#26048=CARTESIAN_POINT('Ctrl Pts',(-1.17103287111351,-1.62079923931634,
11.4011570985037));
#26049=CARTESIAN_POINT('Ctrl Pts',(-1.28095890319296,-1.53539510147643,
11.3917242485488));
#26050=CARTESIAN_POINT('Ctrl Pts',(-1.45046430713703,-1.37274166259998,
11.3753962728556));
#26051=CARTESIAN_POINT('Ctrl Pts',(-1.51491738958601,-1.30126559770483,
11.3686448961182));
#26052=CARTESIAN_POINT('Ctrl Pts',(-1.61243467974873,-1.176011483173,11.357737462348));
#26053=CARTESIAN_POINT('Ctrl Pts',(-1.64855920119987,-1.12481240610626,
11.3535049234383));
#26054=CARTESIAN_POINT('Ctrl Pts',(-1.68593214343734,-1.06616514973489,
11.3489700326566));
#26055=CARTESIAN_POINT('Ctrl Pts',(-1.68961570199279,-1.06031792485678,
11.3485212377572));
#26056=CARTESIAN_POINT('Ctrl Pts',(-1.69507256614742,-1.05155513440061,
11.3478537763595));
#26057=CARTESIAN_POINT('Ctrl Pts',(-1.69686885012071,-1.04865404738951,
11.3476336324629));
#26058=CARTESIAN_POINT('Ctrl Pts',(-1.69993625787856,-1.0436715142072,11.3472569850947));
#26059=CARTESIAN_POINT('Ctrl Pts',(-1.70121101395357,-1.04159233708212,
11.3471002426869));
#26060=CARTESIAN_POINT('Ctrl Pts',(-1.70385671008482,-1.03725928926541,
11.3467744864204));
#26061=CARTESIAN_POINT('Ctrl Pts',(-1.70522698784058,-1.03500504433891,
11.3466055160234));
#26062=CARTESIAN_POINT('Ctrl Pts',(-1.70901135214203,-1.02875146803669,
11.3461381412386));
#26063=CARTESIAN_POINT('Ctrl Pts',(-1.71141588775784,-1.0247463319942,11.3458403589902));
#26064=CARTESIAN_POINT('Ctrl Pts',(-1.72089003532516,-1.00883927447145,
11.3446636473225));
#26065=CARTESIAN_POINT('Ctrl Pts',(-1.72784994749971,-0.996871997751052,
11.3437915981138));
#26066=CARTESIAN_POINT('Ctrl Pts',(-1.80206042138588,-0.866157640561091,
11.3343983272512));
#26067=CARTESIAN_POINT('Ctrl Pts',(-1.85709048237705,-0.740862511226564,
11.326551437279));
#26068=CARTESIAN_POINT('Ctrl Pts',(-1.94471219943039,-0.468508317244706,
11.3099556916309));
#26069=CARTESIAN_POINT('Ctrl Pts',(-1.97435629501184,-0.321425209948056,
11.3012230293888));
#26070=CARTESIAN_POINT('Ctrl Pts',(-1.98849628779947,-0.158450961733807,
11.291024449328));
#26071=CARTESIAN_POINT('Ctrl Pts',(-1.98956099172601,-0.14446881366375,
11.2901457708214));
#26072=CARTESIAN_POINT('Ctrl Pts',(-1.99089936334497,-0.124051407241659,
11.2888568439449));
#26073=CARTESIAN_POINT('Ctrl Pts',(-1.9912894367552,-0.11762399455444,11.2884502464913));
#26074=CARTESIAN_POINT('Ctrl Pts',(-1.99191996569431,-0.106330380202884,
11.2877342897963));
#26075=CARTESIAN_POINT('Ctrl Pts',(-1.99217372799311,-0.101464951042295,
11.2874253503271));
#26076=CARTESIAN_POINT('Ctrl Pts',(-1.99263245238927,-0.0920034661096103,
11.2868235911062));
#26077=CARTESIAN_POINT('Ctrl Pts',(-1.99283934400358,-0.0874075311297139,
11.286530833881));
#26078=CARTESIAN_POINT('Ctrl Pts',(-1.99334947391403,-0.0751301167560543,
11.2857475460491));
#26079=CARTESIAN_POINT('Ctrl Pts',(-1.9936242071673,-0.067447590412097,
11.2852561253582));
#26080=CARTESIAN_POINT('Ctrl Pts',(-1.99445806607978,-0.0396281648272461,
11.2834718654378));
#26081=CARTESIAN_POINT('Ctrl Pts',(-1.99475653780781,-0.0194852290356758,
11.2821709080192));
#26082=CARTESIAN_POINT('Ctrl Pts',(-1.99471414973372,0.10898149033513,11.2738132404301));
#26083=CARTESIAN_POINT('Ctrl Pts',(-1.98585511496646,0.217104032450646,
11.2664899925974));
#26084=CARTESIAN_POINT('Ctrl Pts',(-1.95017223943802,0.433901895587183,
11.2513024728591));
#26085=CARTESIAN_POINT('Ctrl Pts',(-1.92289727096811,0.542132887434468,
11.2434556380222));
#26086=CARTESIAN_POINT('Ctrl Pts',(-1.88156141372123,0.6625765128277,11.2346869576134));
#26087=CARTESIAN_POINT('Ctrl Pts',(-1.87621362607337,0.677571722353845,
11.233594879948));
#26088=CARTESIAN_POINT('Ctrl Pts',(-1.85310682343192,0.739991203550207,
11.2290514120307));
#26089=CARTESIAN_POINT('Ctrl Pts',(-1.83372302952571,0.786799050173972,
11.2256499073268));
#26090=CARTESIAN_POINT('Ctrl Pts',(-1.80958192734027,0.839340372631031,
11.2218775000677));
#26091=CARTESIAN_POINT('Ctrl Pts',(-1.80655200324658,0.845842110707983,
11.2214115069976));
#26092=CARTESIAN_POINT('Ctrl Pts',(-1.8020067567347,0.855459650030122,11.2207235776715));
#26093=CARTESIAN_POINT('Ctrl Pts',(-1.80051832436742,0.858587985130398,
11.2205000297473));
#26094=CARTESIAN_POINT('Ctrl Pts',(-1.79785581235016,0.864146587608158,
11.2201032257265));
#26095=CARTESIAN_POINT('Ctrl Pts',(-1.79668494584757,0.866578359158642,
11.2199297728655));
#26096=CARTESIAN_POINT('Ctrl Pts',(-1.79416920624207,0.871776279661413,
11.219559322282));
#26097=CARTESIAN_POINT('Ctrl Pts',(-1.79282287455694,0.874541687506327,
11.219362417559));
#26098=CARTESIAN_POINT('Ctrl Pts',(-1.78912833019076,0.882086011899745,
11.2188257114352));
#26099=CARTESIAN_POINT('Ctrl Pts',(-1.78676734926795,0.886858700943163,
11.2184866976372));
#26100=CARTESIAN_POINT('Ctrl Pts',(-1.7744326984453,0.911543819822088,11.2167356536189));
#26101=CARTESIAN_POINT('Ctrl Pts',(-1.76414470304014,0.931298612001251,
11.2153424252113));
#26102=CARTESIAN_POINT('Ctrl Pts',(-1.73327010004191,0.988234904828696,
11.2113385374838));
#26103=CARTESIAN_POINT('Ctrl Pts',(-1.71182265606783,1.02493763822833,11.2087720950914));
#26104=CARTESIAN_POINT('Ctrl Pts',(-1.66667147435011,1.09682758747717,11.2037183604904));
#26105=CARTESIAN_POINT('Ctrl Pts',(-1.64298589889468,1.13199918801789,11.2012321719789));
#26106=CARTESIAN_POINT('Ctrl Pts',(-1.51091864981972,1.31522324214131,11.1880656825469));
#26107=CARTESIAN_POINT('Ctrl Pts',(-1.38363604813714,1.44852782860564,11.1776153939314));
#26108=CARTESIAN_POINT('Ctrl Pts',(-1.22476888851582,1.5745931111486,11.1650457384017));
#26109=CARTESIAN_POINT('Ctrl Pts',(-1.20943111860765,1.58640430658461,11.1638376301024));
#26110=CARTESIAN_POINT('Ctrl Pts',(-1.18786436662905,1.60251771630324,11.1621451762499));
#26111=CARTESIAN_POINT('Ctrl Pts',(-1.18177880260236,1.60701077897569,11.1616682961255));
#26112=CARTESIAN_POINT('Ctrl Pts',(-1.17197033170511,1.61416667453005,11.1609007070685));
#26113=CARTESIAN_POINT('Ctrl Pts',(-1.16826351885159,1.61685152735509,11.1606108536295));
#26114=CARTESIAN_POINT('Ctrl Pts',(-1.16058158844212,1.62237535741303,11.1600106303612));
#26115=CARTESIAN_POINT('Ctrl Pts',(-1.15660522084007,1.62521253570094,11.1597001939598));
#26116=CARTESIAN_POINT('Ctrl Pts',(-1.14729659825684,1.63180286712385,11.1589740372681));
#26117=CARTESIAN_POINT('Ctrl Pts',(-1.14195630565864,1.63554451966978,11.1585578805209));
#26118=CARTESIAN_POINT('Ctrl Pts',(-1.12471266151726,1.64750057889092,11.1572154481452));
#26119=CARTESIAN_POINT('Ctrl Pts',(-1.11273850688099,1.65561158651543,11.1562852651877));
#26120=CARTESIAN_POINT('Ctrl Pts',(-1.08460455151432,1.6742257780697,11.1541039777264));
#26121=CARTESIAN_POINT('Ctrl Pts',(-1.06837884933993,1.68462624348337,11.1528491538563));
#26122=CARTESIAN_POINT('Ctrl Pts',(-1.01125892502959,1.72008224887004,11.1484418047274));
#26123=CARTESIAN_POINT('Ctrl Pts',(-0.969616550873315,1.7438952595526,11.1452458812956));
#26124=CARTESIAN_POINT('Ctrl Pts',(-0.746266333009698,1.86114313851902,
11.1281966848339));
#26125=CARTESIAN_POINT('Ctrl Pts',(-0.551892657704264,1.9277356069535,11.1135097981827));
#26126=CARTESIAN_POINT('Ctrl Pts',(-0.341177652899238,1.96538068168746,
11.0991978668756));
#26127=CARTESIAN_POINT('Ctrl Pts',(-0.331527084905448,1.96703157441143,
11.0985461644639));
#26128=CARTESIAN_POINT('Ctrl Pts',(-0.315736022130048,1.96961338586238,
11.0974863651123));
#26129=CARTESIAN_POINT('Ctrl Pts',(-0.309602755153813,1.9705867810459,11.0970763532846));
#26130=CARTESIAN_POINT('Ctrl Pts',(-0.291290409597636,1.97340548064566,
11.0958571767614));
#26131=CARTESIAN_POINT('Ctrl Pts',(-0.279098391181395,1.9751666765927,11.0950520762503));
#26132=CARTESIAN_POINT('Ctrl Pts',(-0.262474955543196,1.9774110125116,11.093964039578));
#26133=CARTESIAN_POINT('Ctrl Pts',(-0.258057399642526,1.97799236452394,
11.0936758319242));
#26134=CARTESIAN_POINT('Ctrl Pts',(-0.251063972197548,1.97888887465765,
11.0932210815517));
#26135=CARTESIAN_POINT('Ctrl Pts',(-0.248489403668808,1.97921381180342,
11.0930539929213));
#26136=CARTESIAN_POINT('Ctrl Pts',(-0.243206726917152,1.9798700699711,11.0927118230577));
#26137=CARTESIAN_POINT('Ctrl Pts',(-0.240498578913211,1.98020085839826,
11.0925367756152));
#26138=CARTESIAN_POINT('Ctrl Pts',(-0.234131735779365,1.98096528660171,
11.0921260828978));
#26139=CARTESIAN_POINT('Ctrl Pts',(-0.230472481476498,1.9813943505102,11.0918906960174));
#26140=CARTESIAN_POINT('Ctrl Pts',(-0.2185267537348,1.98276149983412,11.0911243385719));
#26141=CARTESIAN_POINT('Ctrl Pts',(-0.210235444758749,1.98365777566052,
11.0905956709455));
#26142=CARTESIAN_POINT('Ctrl Pts',(-0.109096762730718,1.99394942660463,
11.0841837881886));
#26143=CARTESIAN_POINT('Ctrl Pts',(-0.0156924274389661,1.99687133690277,
11.0786385887509));
#26144=CARTESIAN_POINT('Ctrl Pts',(0.20197861287314,1.98839871846358,11.0659008717482));
#26145=CARTESIAN_POINT('Ctrl Pts',(0.325642823904791,1.9719232850224,11.058791286622));
#26146=CARTESIAN_POINT('Ctrl Pts',(0.470385409641683,1.93864453764539,11.0499784270535));
#26147=CARTESIAN_POINT('Ctrl Pts',(0.493706062181091,1.93283712319577,11.0485436095578));
#26148=CARTESIAN_POINT('Ctrl Pts',(0.571294044103228,1.91202002185902,11.0437107036334));
#26149=CARTESIAN_POINT('Ctrl Pts',(0.625025987981041,1.89513562903186,11.0402651180139));
#26150=CARTESIAN_POINT('Ctrl Pts',(0.687427807448072,1.8725842402793,11.0361147830802));
#26151=CARTESIAN_POINT('Ctrl Pts',(0.696860994846514,1.86909429278878,11.0354833266871));
#26152=CARTESIAN_POINT('Ctrl Pts',(0.71210843460038,1.86332180516486,11.0344558982169));
#26153=CARTESIAN_POINT('Ctrl Pts',(0.717939146868416,1.86108300518392,11.0340613892884));
#26154=CARTESIAN_POINT('Ctrl Pts',(0.728273838849401,1.85705903249711,11.0333592268182));
#26155=CARTESIAN_POINT('Ctrl Pts',(0.732782030381808,1.85528475706629,11.0330519414998));
#26156=CARTESIAN_POINT('Ctrl Pts',(0.742233270264344,1.85152523877342,11.0324056312807));
#26157=CARTESIAN_POINT('Ctrl Pts',(0.747174913065369,1.84953658673747,11.0320664933089));
#26158=CARTESIAN_POINT('Ctrl Pts',(0.760134975801118,1.84426068711078,11.0311738460251));
#26159=CARTESIAN_POINT('Ctrl Pts',(0.76813997414649,1.84094096582307,11.0306192410278));
#26160=CARTESIAN_POINT('Ctrl Pts',(0.803972814082364,1.82580646631468,11.0281218408807));
#26161=CARTESIAN_POINT('Ctrl Pts',(0.83155027754727,1.81341266876545,11.0261594335594));
#26162=CARTESIAN_POINT('Ctrl Pts',(0.904314029014205,1.7787025557704,11.020869593305));
#26163=CARTESIAN_POINT('Ctrl Pts',(0.948951889413259,1.75529377540411,11.017506079385));
#26164=CARTESIAN_POINT('Ctrl Pts',(1.07945595432892,1.68042174971877,11.0073161832775));
#26165=CARTESIAN_POINT('Ctrl Pts',(1.16238131418147,1.6241640242548,11.0003525775965));
#26166=CARTESIAN_POINT('Ctrl Pts',(1.33715080289835,1.48533470045382,10.9847795593506));
#26167=CARTESIAN_POINT('Ctrl Pts',(1.42628573532158,1.3999671067408,10.976190332675));
#26168=CARTESIAN_POINT('Ctrl Pts',(1.511934732569,1.3012063628643,10.9676555821612));
#26169=CARTESIAN_POINT('Ctrl Pts',(1.51685195699323,1.29547087165352,10.9671645487956));
#26170=CARTESIAN_POINT('Ctrl Pts',(1.52399989745012,1.28703695726432,10.9664493991542));
#26171=CARTESIAN_POINT('Ctrl Pts',(1.52625620968471,1.28436046328533,10.9662234552391));
#26172=CARTESIAN_POINT('Ctrl Pts',(1.53024688085735,1.27960126269821,10.9658234999083));
#26173=CARTESIAN_POINT('Ctrl Pts',(1.53198405293116,1.27752094690757,10.9656492832129));
#26174=CARTESIAN_POINT('Ctrl Pts',(1.53564809435162,1.27311492576691,10.9652815930475));
#26175=CARTESIAN_POINT('Ctrl Pts',(1.53757391806136,1.27078838942245,10.9650881954876));
#26176=CARTESIAN_POINT('Ctrl Pts',(1.54272170582291,1.26454065076075,10.9645708355375));
#26177=CARTESIAN_POINT('Ctrl Pts',(1.54593402856096,1.26061147850669,10.9642475677505));
#26178=CARTESIAN_POINT('Ctrl Pts',(1.5612822600414,1.2416912957655,10.9627007333817));
#26179=CARTESIAN_POINT('Ctrl Pts',(1.57321581985781,1.22653643264868,10.9614911285787));
#26180=CARTESIAN_POINT('Ctrl Pts',(1.60592962879547,1.18372880164766,10.9581479929672));
#26181=CARTESIAN_POINT('Ctrl Pts',(1.62621404579863,1.15570412278028,10.9560431134106));
#26182=CARTESIAN_POINT('Ctrl Pts',(1.69760624878023,1.05146514246465,10.9484579299611));
#26183=CARTESIAN_POINT('Ctrl Pts',(1.74417085959855,0.972273731676528,10.9431531070067));
#26184=CARTESIAN_POINT('Ctrl Pts',(1.85458578864389,0.750846761892662,10.9288028019407));
#26185=CARTESIAN_POINT('Ctrl Pts',(1.90749604478679,0.603911316919937,10.9197330629681));
#26186=CARTESIAN_POINT('Ctrl Pts',(1.945639820445,0.440081144942404,10.9092289437504));
#26187=CARTESIAN_POINT('Ctrl Pts',(1.94837566380584,0.42780601465771,10.9084400025407));
#26188=CARTESIAN_POINT('Ctrl Pts',(1.95227845828373,0.409480569795257,10.9072590435396));
#26189=CARTESIAN_POINT('Ctrl Pts',(1.95353378138997,0.403449227664561,10.906869855045));
#26190=CARTESIAN_POINT('Ctrl Pts',(1.95572428910217,0.392674724251599,10.9061736588264));
#26191=CARTESIAN_POINT('Ctrl Pts',(1.95667021213585,0.387933775683647,10.9058669968145));
#26192=CARTESIAN_POINT('Ctrl Pts',(1.9586309279056,0.377917072951118,10.9052183735151));
#26193=CARTESIAN_POINT('Ctrl Pts',(1.95964165833786,0.372640571800645,10.9048762853009));
#26194=CARTESIAN_POINT('Ctrl Pts',(1.96226479608967,0.358640669761366,10.9039675118626));
#26195=CARTESIAN_POINT('Ctrl Pts',(1.96384033301381,0.34991056313041,10.9033996579913));
#26196=CARTESIAN_POINT('Ctrl Pts',(1.97088659520713,0.309319624980195,10.9007538031932));
#26197=CARTESIAN_POINT('Ctrl Pts',(1.97564026137116,0.277340864941067,10.8986532161165));
#26198=CARTESIAN_POINT('Ctrl Pts',(1.98641214249404,0.190396476743029,10.8928947489147));
#26199=CARTESIAN_POINT('Ctrl Pts',(1.99092525056377,0.135276499381504,10.8891924199297));
#26200=CARTESIAN_POINT('Ctrl Pts',(1.99731373093364,-0.0237999900573737,
10.8783675871078));
#26201=CARTESIAN_POINT('Ctrl Pts',(1.9933618471923,-0.127804115035621,10.8711102724036));
#26202=CARTESIAN_POINT('Ctrl Pts',(1.96840327881251,-0.341862118209449,
10.8560819114379));
#26203=CARTESIAN_POINT('Ctrl Pts',(1.94619830397782,-0.45144183950228,10.8483393833563));
#26204=CARTESIAN_POINT('Ctrl Pts',(1.91298558663952,-0.565298499776993,
10.8405935926979));
#26205=CARTESIAN_POINT('Ctrl Pts',(1.91099646315087,-0.571986686768454,
10.8401397531064));
#26206=CARTESIAN_POINT('Ctrl Pts',(1.9079600016913,-0.582003754515409,10.839461919585));
#26207=CARTESIAN_POINT('Ctrl Pts',(1.90693898253526,-0.58534046132441,10.8392364479633));
#26208=CARTESIAN_POINT('Ctrl Pts',(1.90515998825462,-0.591100183475566,
10.83884781316));
#26209=CARTESIAN_POINT('Ctrl Pts',(1.9044061375858,-0.593524448573728,10.8386844109206));
#26210=CARTESIAN_POINT('Ctrl Pts',(1.90282145889481,-0.59858642293466,10.8383435932321));
#26211=CARTESIAN_POINT('Ctrl Pts',(1.90198977273272,-0.601223847402193,
10.8381662315056));
#26212=CARTESIAN_POINT('Ctrl Pts',(1.8999729660485,-0.607573431998805,10.8377397304922));
#26213=CARTESIAN_POINT('Ctrl Pts',(1.89878243922579,-0.611283891576089,
10.8374909083308));
#26214=CARTESIAN_POINT('Ctrl Pts',(1.89462939570906,-0.624098287545705,
10.8366329175562));
#26215=CARTESIAN_POINT('Ctrl Pts',(1.89161215794336,-0.633184548359881,
10.8360268838645));
#26216=CARTESIAN_POINT('Ctrl Pts',(1.86591014906682,-0.708761165815411,
10.83100287727));
#26217=CARTESIAN_POINT('Ctrl Pts',(1.83978999220034,-0.774040176661591,
10.826771464365));
#26218=CARTESIAN_POINT('Ctrl Pts',(1.71995802878394,-1.0329635103083,10.8099169845858));
#26219=CARTESIAN_POINT('Ctrl Pts',(1.59868925052306,-1.21221524453463,10.7979075049042));
#26220=CARTESIAN_POINT('Ctrl Pts',(1.43841788903086,-1.38214516490472,10.7834184070685));
#26221=CARTESIAN_POINT('Ctrl Pts',(1.42551023265425,-1.39545398367508,10.7822607504544));
#26222=CARTESIAN_POINT('Ctrl Pts',(1.4071744588801,-1.4138397261316,10.7806279904034));
#26223=CARTESIAN_POINT('Ctrl Pts',(1.40190036466913,-1.41906944651749,10.7801596713481));
#26224=CARTESIAN_POINT('Ctrl Pts',(1.39334775204551,-1.4274558894862,10.7794022968901));
#26225=CARTESIAN_POINT('Ctrl Pts',(1.39008738814232,-1.43063109407207,10.779114054218));
#26226=CARTESIAN_POINT('Ctrl Pts',(1.38329341326811,-1.43720246157727,10.7785143835791));
#26227=CARTESIAN_POINT('Ctrl Pts',(1.3797580982615,-1.44059681116248,10.778202879712));
#26228=CARTESIAN_POINT('Ctrl Pts',(1.37141879070365,-1.44854474435454,10.7774693301549));
#26229=CARTESIAN_POINT('Ctrl Pts',(1.36660459362305,-1.4530874918027,10.7770468213284));
#26230=CARTESIAN_POINT('Ctrl Pts',(1.35080235057007,-1.46785073063549,10.7756630236307));
#26231=CARTESIAN_POINT('Ctrl Pts',(1.3397217800798,-1.47797100419504,10.7746974823524));
#26232=CARTESIAN_POINT('Ctrl Pts',(1.3134688300473,-1.50141092793196,10.7724204592106));
#26233=CARTESIAN_POINT('Ctrl Pts',(1.29820655542032,-1.51462696130548,10.7711048003558));
#26234=CARTESIAN_POINT('Ctrl Pts',(1.24352974053001,-1.56053957536424,10.7664186534991));
#26235=CARTESIAN_POINT('Ctrl Pts',(1.20306225242803,-1.59194549102781,10.7629984954555));
#26236=CARTESIAN_POINT('Ctrl Pts',(1.07961189172609,-1.68035540833415,10.7527077093552));
#26237=CARTESIAN_POINT('Ctrl Pts',(0.993478856661449,-1.73267209620089,
10.745700469698));
#26238=CARTESIAN_POINT('Ctrl Pts',(0.795663834775676,-1.83320858555724,
10.7302186708135));
#26239=CARTESIAN_POINT('Ctrl Pts',(0.68275319723829,-1.87818796353214,10.7217669820146));
#26240=CARTESIAN_POINT('Ctrl Pts',(0.559888341819996,-1.9145755016175,10.7134005982871));
#26241=CARTESIAN_POINT('Ctrl Pts',(0.55332276636768,-1.91648329661188,10.7129559924206));
#26242=CARTESIAN_POINT('Ctrl Pts',(0.543425704378367,-1.91930403954843,
10.7122896361611));
#26243=CARTESIAN_POINT('Ctrl Pts',(0.540101527074303,-1.92024212882044,
10.7120664755009));
#26244=CARTESIAN_POINT('Ctrl Pts',(0.534338602189818,-1.92185228870698,
10.7116807440751));
#26245=CARTESIAN_POINT('Ctrl Pts',(0.531900995442505,-1.92252835938038,
10.7115179424627));
#26246=CARTESIAN_POINT('Ctrl Pts',(0.526787963007332,-1.92393599100447,
10.7111772102434));
#26247=CARTESIAN_POINT('Ctrl Pts',(0.524112291688488,-1.92466661042395,
10.7109993370033));
#26248=CARTESIAN_POINT('Ctrl Pts',(0.517708900616808,-1.92640077854165,
10.7105746698735));
#26249=CARTESIAN_POINT('Ctrl Pts',(0.513979749351479,-1.92739909806181,
10.7103281792805));
#26250=CARTESIAN_POINT('Ctrl Pts',(0.501271270038886,-1.93076173922968,
10.7094908980206));
#26251=CARTESIAN_POINT('Ctrl Pts',(0.492278171765269,-1.93307423278164,
10.7089030301733));
#26252=CARTESIAN_POINT('Ctrl Pts',(0.470452452215516,-1.93852432549036,
10.7074867761515));
#26253=CARTESIAN_POINT('Ctrl Pts',(0.45760400021766,-1.94159745314368,10.7066617780542));
#26254=CARTESIAN_POINT('Ctrl Pts',(0.409409218789583,-1.95261981403455,
10.7035965335695));
#26255=CARTESIAN_POINT('Ctrl Pts',(0.373877085727865,-1.95973373268864,
10.7013954269203));
#26256=CARTESIAN_POINT('Ctrl Pts',(0.217022144433218,-1.986715817347,10.6918580652488));
#26257=CARTESIAN_POINT('Ctrl Pts',(0.094201094630038,-1.99631375931502,
10.6848434951022));
#26258=CARTESIAN_POINT('Ctrl Pts',(-0.150098987651191,-1.99279492673645,
10.6706009047127));
#26259=CARTESIAN_POINT('Ctrl Pts',(-0.271037755010063,-1.97997311258582,
10.6634023191527));
#26260=CARTESIAN_POINT('Ctrl Pts',(-0.40280551753441,-1.95370018279441,
10.6550161586736));
#26261=CARTESIAN_POINT('Ctrl Pts',(-0.415533921375953,-1.95103260778462,
10.6542006091297));
#26262=CARTESIAN_POINT('Ctrl Pts',(-0.43433448633204,-1.94690013007262,
10.6529875369877));
#26263=CARTESIAN_POINT('Ctrl Pts',(-0.440427490029545,-1.94553082398599,
10.6525930767661));
#26264=CARTESIAN_POINT('Ctrl Pts',(-0.451235666931748,-1.94304848278454,
10.6518909692361));
#26265=CARTESIAN_POINT('Ctrl Pts',(-0.455953425466466,-1.94194683415626,
10.6515836899444));
#26266=CARTESIAN_POINT('Ctrl Pts',(-0.465850284518916,-1.93959775571201,
10.6509373601097));
#26267=CARTESIAN_POINT('Ctrl Pts',(-0.471028487880685,-1.93834674510174,
10.6505981963727));
#26268=CARTESIAN_POINT('Ctrl Pts',(-0.484618831478258,-1.93500575779146,
10.6497054082381));
#26269=CARTESIAN_POINT('Ctrl Pts',(-0.493022396916671,-1.93288168461351,
10.6491506875261));
#26270=CARTESIAN_POINT('Ctrl Pts',(-0.530690230874716,-1.9230991883353,
10.6466520288688));
#26271=CARTESIAN_POINT('Ctrl Pts',(-0.559790539553972,-1.91483080034854,
10.6446884544847));
#26272=CARTESIAN_POINT('Ctrl Pts',(-0.636874061173812,-1.89102146065539,
10.6393947127876));
#26273=CARTESIAN_POINT('Ctrl Pts',(-0.684472333285816,-1.87431791305439,
10.636028398905));
#26274=CARTESIAN_POINT('Ctrl Pts',(-0.877401596119748,-1.79828440702858,
10.6219833888218));
#26275=CARTESIAN_POINT('Ctrl Pts',(-1.0161119061499,-1.723707522456,10.6108727852393));
#26276=CARTESIAN_POINT('Ctrl Pts',(-1.1581947589843,-1.62415731277163,10.59892463305));
#26277=CARTESIAN_POINT('Ctrl Pts',(-1.17164534681666,-1.61448111816995,
10.5977880160493));
#26278=CARTESIAN_POINT('Ctrl Pts',(-1.22544568058563,-1.5747512906306,10.5932236350435));
#26279=CARTESIAN_POINT('Ctrl Pts',(-1.26477623830486,-1.54334079418733,
10.5898448501145));
#26280=CARTESIAN_POINT('Ctrl Pts',(-1.30830296841903,-1.50579619735658,
10.5860947100608));
#26281=CARTESIAN_POINT('Ctrl Pts',(-1.3137004703893,-1.5010895786146,10.5856294844136));
#26282=CARTESIAN_POINT('Ctrl Pts',(-1.32166963728357,-1.494064562879,10.584942466842));
#26283=CARTESIAN_POINT('Ctrl Pts',(-1.32426072709766,-1.4917684388939,10.5847190693551));
#26284=CARTESIAN_POINT('Ctrl Pts',(-1.32886096642559,-1.48767045326297,
10.5843224312973));
#26285=CARTESIAN_POINT('Ctrl Pts',(-1.33087244476128,-1.48587125340549,
10.5841489945939));
#26286=CARTESIAN_POINT('Ctrl Pts',(-1.33476482285541,-1.48237540665768,
10.5838133751035));
#26287=CARTESIAN_POINT('Ctrl Pts',(-1.33664613006854,-1.48067927038371,
10.5836511557962));
#26288=CARTESIAN_POINT('Ctrl Pts',(-1.34196213486135,-1.47586811449661,
10.5831927444763));
#26289=CARTESIAN_POINT('Ctrl Pts',(-1.34538923787452,-1.47274466980684,
10.5828971835219));
#26290=CARTESIAN_POINT('Ctrl Pts',(-1.35975228755055,-1.45956228161801,
10.5816581807811));
#26291=CARTESIAN_POINT('Ctrl Pts',(-1.37058690733418,-1.44939294131666,
10.5807228128043));
#26292=CARTESIAN_POINT('Ctrl Pts',(-1.39888315082848,-1.42223310402637,
10.578274721014));
#26293=CARTESIAN_POINT('Ctrl Pts',(-1.41614936628058,-1.4050416929023,10.576775512938));
#26294=CARTESIAN_POINT('Ctrl Pts',(-1.48722382436947,-1.33163351269884,
10.5705584605321));
#26295=CARTESIAN_POINT('Ctrl Pts',(-1.53803771669201,-1.27260540314262,
10.5659986970419));
#26296=CARTESIAN_POINT('Ctrl Pts',(-1.69062725996627,-1.07281551577602,
10.551376716922));
#26297=CARTESIAN_POINT('Ctrl Pts',(-1.77751254700866,-0.921735378559279,
10.5414384016456));
#26298=CARTESIAN_POINT('Ctrl Pts',(-1.85148416868359,-0.742593142861553,
10.529436796406));
#26299=CARTESIAN_POINT('Ctrl Pts',(-1.85893220067566,-0.72374666056684,
10.5281728602616));
#26300=CARTESIAN_POINT('Ctrl Pts',(-1.8688144019601,-0.697581306868724,
10.5264149377355));
#26301=CARTESIAN_POINT('Ctrl Pts',(-1.87149536157609,-0.690356471377057,
10.5259292106535));
#26302=CARTESIAN_POINT('Ctrl Pts',(-1.87571111221322,-0.678790531014614,
10.5251510395536));
#26303=CARTESIAN_POINT('Ctrl Pts',(-1.87727287234161,-0.674459282436686,
10.5248594960355));
#26304=CARTESIAN_POINT('Ctrl Pts',(-1.88045574173863,-0.665535487599173,
10.5242585320391));
#26305=CARTESIAN_POINT('Ctrl Pts',(-1.88207505375224,-0.660942337306063,
10.5239490542189));
#26306=CARTESIAN_POINT('Ctrl Pts',(-1.88579234504433,-0.650273869073988,
10.523229847435));
#26307=CARTESIAN_POINT('Ctrl Pts',(-1.88787780509945,-0.644194275698024,
10.5228197070701));
#26308=CARTESIAN_POINT('Ctrl Pts',(-1.89439916021462,-0.624879375940557,
10.5215157094706));
#26309=CARTESIAN_POINT('Ctrl Pts',(-1.89872545071886,-0.611607765661261,
10.5206182519358));
#26310=CARTESIAN_POINT('Ctrl Pts',(-1.94370860280674,-0.468535547863655,
10.5109259451319));
#26311=CARTESIAN_POINT('Ctrl Pts',(-1.97111857903476,-0.334972842261761,
10.5016865325503));
#26312=CARTESIAN_POINT('Ctrl Pts',(-1.99145701881209,-0.132824304519319,
10.4875693700212));
#26313=CARTESIAN_POINT('Ctrl Pts',(-1.99480094163841,-0.0656668475864861,
10.4828651127876));
#26314=CARTESIAN_POINT('Ctrl Pts',(-1.99474941351911,0.00152962909411654,
10.478194963257));
#26315=CARTESIAN_POINT('',(-1.99474949650966,-0.00141727712825375,9.67904511860478));
#26316=CARTESIAN_POINT('Ctrl Pts',(-1.99474949650966,-0.00141727712825375,
9.67904511860478));
#26317=CARTESIAN_POINT('Ctrl Pts',(-1.99468698571738,-0.0893982153304589,
9.68468225042636));
#26318=CARTESIAN_POINT('Ctrl Pts',(-1.98880353854553,-0.177174871919355,
9.69031938224794));
#26319=CARTESIAN_POINT('Ctrl Pts',(-1.97718053383553,-0.264167937346383,
9.69595651406953));
#26320=CARTESIAN_POINT('Ctrl Pts',(-1.967996907368,-0.332903332201714,9.70041055278751));
#26321=CARTESIAN_POINT('Ctrl Pts',(-1.95520650942798,-0.401295387301663,
9.70486459150549));
#26322=CARTESIAN_POINT('Ctrl Pts',(-1.93884667508122,-0.468936171591067,
9.70931863022347));
#26323=CARTESIAN_POINT('Ctrl Pts',(-1.92251143210734,-0.536475281272242,
9.71376597382923));
#26324=CARTESIAN_POINT('Ctrl Pts',(-1.90261751589915,-0.603264889514319,
9.71821331743499));
#26325=CARTESIAN_POINT('Ctrl Pts',(-1.87925378838465,-0.668904149592394,
9.72266066104075));
#26326=CARTESIAN_POINT('Ctrl Pts',(-1.85591760430336,-0.734466027729838,
9.72710276168554));
#26327=CARTESIAN_POINT('Ctrl Pts',(-1.82911989663795,-0.798879792183266,
9.73154486233033));
#26328=CARTESIAN_POINT('Ctrl Pts',(-1.79899969029709,-0.861758479396032,
9.73598696297511));
#26329=CARTESIAN_POINT('Ctrl Pts',(-1.76889848391584,-0.924597502454316,
9.74042626152313));
#26330=CARTESIAN_POINT('Ctrl Pts',(-1.73547914754314,-0.985902928728562,
9.74486556007115));
#26331=CARTESIAN_POINT('Ctrl Pts',(-1.6989287184433,-1.04530797956804,9.74930485861917));
#26332=CARTESIAN_POINT('Ctrl Pts',(-1.66238892559304,-1.10469574341628,
9.75374286532223));
#26333=CARTESIAN_POINT('Ctrl Pts',(-1.62272010521412,-1.16218381290231,
9.7581808720253));
#26334=CARTESIAN_POINT('Ctrl Pts',(-1.58015423331931,-1.21743178922807,
9.76261887872837));
#26335=CARTESIAN_POINT('Ctrl Pts',(-1.53758628461752,-1.27268246112608,
9.76705710196367));
#26336=CARTESIAN_POINT('Ctrl Pts',(-1.4921213044535,-1.32569243652428,9.77149532519897));
#26337=CARTESIAN_POINT('Ctrl Pts',(-1.44403231901547,-1.37615341591655,
9.77593354843427));
#26338=CARTESIAN_POINT('Ctrl Pts',(-1.39589238860436,-1.42666785314775,
9.78037647347729));
#26339=CARTESIAN_POINT('Ctrl Pts',(-1.34512324289893,-1.47462754943579,
9.78481939852032));
#26340=CARTESIAN_POINT('Ctrl Pts',(-1.29203496222465,-1.51976090846197,
9.78926232356335));
#26341=CARTESIAN_POINT('Ctrl Pts',(-1.23891569173576,-1.56492061368756,
9.7937078421246));
#26342=CARTESIAN_POINT('Ctrl Pts',(-1.18347498097302,-1.60725040063283,
9.79815336068585));
#26343=CARTESIAN_POINT('Ctrl Pts',(-1.12605397614748,-1.64652057542639,
9.8025988792471));
#26344=CARTESIAN_POINT('Ctrl Pts',(-1.06853277006565,-1.68585927777117,
9.80705215536234));
#26345=CARTESIAN_POINT('Ctrl Pts',(-1.00902478978249,-1.72212745539155,
9.81150543147757));
#26346=CARTESIAN_POINT('Ctrl Pts',(-0.947897277366771,-1.75514053968925,
9.81595870759281));
#26347=CARTESIAN_POINT('Ctrl Pts',(-0.915165252298684,-1.77281809698061,
9.81834330889063));
#26348=CARTESIAN_POINT('Ctrl Pts',(-0.881969234569759,-1.78956313413351,
9.82072791018845));
#26349=CARTESIAN_POINT('Ctrl Pts',(-0.848367782930476,-1.80535305892937,
9.82311251148626));
#26350=CARTESIAN_POINT('Ctrl Pts',(-0.785605858444948,-1.83484601293351,
9.82756655020425));
#26351=CARTESIAN_POINT('Ctrl Pts',(-0.721179850639054,-1.86112065847741,
9.83202058892224));
#26352=CARTESIAN_POINT('Ctrl Pts',(-0.655452944263182,-1.88398752659266,
9.83647462764022));
#26353=CARTESIAN_POINT('Ctrl Pts',(-0.589824835639725,-1.90682002225226,
9.84092197124598));
#26354=CARTESIAN_POINT('Ctrl Pts',(-0.522900168142998,-1.92625474766008,
9.84536931485173));
#26355=CARTESIAN_POINT('Ctrl Pts',(-0.455064067573062,-1.94214939098512,
9.84981665845749));
#26356=CARTESIAN_POINT('Ctrl Pts',(-0.387307938792854,-1.95802529615948,
9.85425875910228));
#26357=CARTESIAN_POINT('Ctrl Pts',(-0.318642985354545,-1.97036929698977,
9.85870085974706));
#26358=CARTESIAN_POINT('Ctrl Pts',(-0.249469819512031,-1.97908877306013,
9.86314296039185));
#26359=CARTESIAN_POINT('Ctrl Pts',(-0.18034028840896,-1.98780274884635,
9.86758225893987));
#26360=CARTESIAN_POINT('Ctrl Pts',(-0.110703665453911,-1.99289667441333,
9.8720215574879));
#26361=CARTESIAN_POINT('Ctrl Pts',(-0.0409695867473876,-1.99432922444158,
9.87646085603592));
#26362=CARTESIAN_POINT('Ctrl Pts',(0.0287441991996099,-1.99576135759484,
9.88089886273898));
#26363=CARTESIAN_POINT('Ctrl Pts',(0.0985548953920414,-1.99353422028129,
9.88533686944205));
#26364=CARTESIAN_POINT('Ctrl Pts',(0.168050714418184,-1.98765855213705,
9.88977487614511));
#26365=CARTESIAN_POINT('Ctrl Pts',(0.237549924174972,-1.98178259731645,
9.89421309938042));
#26366=CARTESIAN_POINT('Ctrl Pts',(0.306733738645927,-1.97225780187023,
9.89865132261572));
#26367=CARTESIAN_POINT('Ctrl Pts',(0.375195133089241,-1.95914679761526,
9.90308954585102));
#26368=CARTESIAN_POINT('Ctrl Pts',(0.4437290548247,-1.9460219036982,9.90753247089405));
#26369=CARTESIAN_POINT('Ctrl Pts',(0.511538547200051,-1.92930331023155,
9.91197539593709));
#26370=CARTESIAN_POINT('Ctrl Pts',(0.57822738240554,-1.90910467411728,9.91641832098011));
#26371=CARTESIAN_POINT('Ctrl Pts',(0.644955146629108,-1.88889424722772,
9.92086383954137));
#26372=CARTESIAN_POINT('Ctrl Pts',(0.710560491034047,-1.86519990068222,
9.92530935810261));
#26373=CARTESIAN_POINT('Ctrl Pts',(0.774665598169962,-1.83818409674112,
9.92975487666387));
#26374=CARTESIAN_POINT('Ctrl Pts',(0.838882570507318,-1.81112114946801,
9.9342081527791));
#26375=CARTESIAN_POINT('Ctrl Pts',(0.901593639171837,-1.78072538837797,
9.93866142889434));
#26376=CARTESIAN_POINT('Ctrl Pts',(0.962444797519434,-1.74720564737749,
9.94311470500958));
#26377=CARTESIAN_POINT('Ctrl Pts',(0.995028842930854,-1.72925678999173,
9.94549930630738));
#26378=CARTESIAN_POINT('Ctrl Pts',(1.02708007614375,-1.71041294983575,9.94788390760518));
#26379=CARTESIAN_POINT('Ctrl Pts',(1.05854779817916,-1.69071112892476,9.95026850890298));
#26380=CARTESIAN_POINT('Ctrl Pts',(1.11732427055702,-1.6539114034389,9.95472254762097));
#26381=CARTESIAN_POINT('Ctrl Pts',(1.17429588030865,-1.61397015705659,9.95917658633896));
#26382=CARTESIAN_POINT('Ctrl Pts',(1.22910669744718,-1.57109015934493,9.96363062505694));
#26383=CARTESIAN_POINT('Ctrl Pts',(1.28383512541142,-1.52827461693224,9.96807796866269));
#26384=CARTESIAN_POINT('Ctrl Pts',(1.33640882480859,-1.48252938982695,9.97252531226844));
#26385=CARTESIAN_POINT('Ctrl Pts',(1.38649963422563,-1.43410122613161,9.9769726558742));
#26386=CARTESIAN_POINT('Ctrl Pts',(1.43653139172723,-1.38573015426331,9.98141475651899));
#26387=CARTESIAN_POINT('Ctrl Pts',(1.48408572251719,-1.33468276637419,9.98585685716378));
#26388=CARTESIAN_POINT('Ctrl Pts',(1.528867859064,-1.28124573444014,9.99029895780856));
#26389=CARTESIAN_POINT('Ctrl Pts',(1.5736217468407,-1.22784241082256,9.99473825635658));
#26390=CARTESIAN_POINT('Ctrl Pts',(1.61560659569774,-1.17205280784211,9.99917755490461));
#26391=CARTESIAN_POINT('Ctrl Pts',(1.65456587922435,-1.11419895611447,10.0036168534526));
#26392=CARTESIAN_POINT('Ctrl Pts',(1.69351382551975,-1.05636193997601,10.0080548601557));
#26393=CARTESIAN_POINT('Ctrl Pts',(1.72943768099633,-0.996462273439538,
10.0124928668588));
#26394=CARTESIAN_POINT('Ctrl Pts',(1.76212352850102,-0.934851984435565,
10.0169308735618));
#26395=CARTESIAN_POINT('Ctrl Pts',(1.79481097076216,-0.873238689439306,
10.0213690967971));
#26396=CARTESIAN_POINT('Ctrl Pts',(1.82425986407292,-0.809915039861802,
10.0258073200324));
#26397=CARTESIAN_POINT('Ctrl Pts',(1.85030249858752,-0.745257154424411,
10.0302455432677));
#26398=CARTESIAN_POINT('Ctrl Pts',(1.87637272239938,-0.680530771092921,
10.0346884683108));
#26399=CARTESIAN_POINT('Ctrl Pts',(1.89902930164196,-0.614467785687102,
10.0391313933538));
#26400=CARTESIAN_POINT('Ctrl Pts',(1.91815327178053,-0.54746286491199,10.0435743183968));
#26401=CARTESIAN_POINT('Ctrl Pts',(1.93728840536764,-0.480418830606623,
10.0480198369581));
#26402=CARTESIAN_POINT('Ctrl Pts',(1.95288671590791,-0.41243224383394,10.0524653555193));
#26403=CARTESIAN_POINT('Ctrl Pts',(1.9648802399255,-0.343908716450044,10.0569108740806));
#26404=CARTESIAN_POINT('Ctrl Pts',(1.97689469297729,-0.275265613598047,
10.0613641501958));
#26405=CARTESIAN_POINT('Ctrl Pts',(1.98529174365158,-0.206084185705428,
10.065817426311));
#26406=CARTESIAN_POINT('Ctrl Pts',(1.99005530723546,-0.136775131672311,
10.0702707024263));
#26407=CARTESIAN_POINT('Ctrl Pts',(1.99260605854986,-0.099662126343055,
10.0726553037241));
#26408=CARTESIAN_POINT('Ctrl Pts',(1.994115875531,-0.0625125326038895,10.0750399050219));
#26409=CARTESIAN_POINT('Ctrl Pts',(1.99458841887371,-0.0253890093321778,
10.0774245063197));
#26410=CARTESIAN_POINT('Ctrl Pts',(1.99547105126442,0.043951559320546,10.0818785450377));
#26411=CARTESIAN_POINT('Ctrl Pts',(1.99273525232063,0.113475532771467,10.0863325837557));
#26412=CARTESIAN_POINT('Ctrl Pts',(1.98635879736995,0.182773878360721,10.0907866224737));
#26413=CARTESIAN_POINT('Ctrl Pts',(1.97999192722178,0.251968057769495,10.0952339660794));
#26414=CARTESIAN_POINT('Ctrl Pts',(1.96999530705612,0.320936798924369,10.0996813096852));
#26415=CARTESIAN_POINT('Ctrl Pts',(1.95639872171989,0.389270605302754,10.104128653291));
#26416=CARTESIAN_POINT('Ctrl Pts',(1.94281816536018,0.457523853147437,10.1085707539357));
#26417=CARTESIAN_POINT('Ctrl Pts',(1.92564616800158,0.525143175045106,10.1130128545805));
#26418=CARTESIAN_POINT('Ctrl Pts',(1.90496416063095,0.591725535372297,10.1174549552253));
#26419=CARTESIAN_POINT('Ctrl Pts',(1.88429519956219,0.658265895251632,10.1218942537733));
#26420=CARTESIAN_POINT('Ctrl Pts',(1.86012076569267,0.723770124743734,10.1263335523214));
#26421=CARTESIAN_POINT('Ctrl Pts',(1.83257272224743,0.787848196148626,10.1307728508694));
#26422=CARTESIAN_POINT('Ctrl Pts',(1.80503269533918,0.851907620703676,10.1352108575725));
#26423=CARTESIAN_POINT('Ctrl Pts',(1.77412120099737,0.914541261513069,10.1396488642755));
#26424=CARTESIAN_POINT('Ctrl Pts',(1.74001839207206,0.975378674029203,10.1440868709786));
#26425=CARTESIAN_POINT('Ctrl Pts',(1.70591391925615,1.03621905482865,10.1485250942139));
#26426=CARTESIAN_POINT('Ctrl Pts',(1.66861806419197,1.09526260746632,10.1529633174492));
#26427=CARTESIAN_POINT('Ctrl Pts',(1.62835625142678,1.15216469349626,10.1574015406845));
#26428=CARTESIAN_POINT('Ctrl Pts',(1.58805178571418,1.20912706100673,10.1618444657275));
#26429=CARTESIAN_POINT('Ctrl Pts',(1.54477537414292,1.26394303336169,10.1662873907706));
#26430=CARTESIAN_POINT('Ctrl Pts',(1.49879442690592,1.31629891300409,10.1707303158136));
#26431=CARTESIAN_POINT('Ctrl Pts',(1.4527866386974,1.36868535492846,10.1751758343749));
#26432=CARTESIAN_POINT('Ctrl Pts',(1.40407151451476,1.41860849534032,10.1796213529361));
#26433=CARTESIAN_POINT('Ctrl Pts',(1.35295327934652,1.46579159037208,10.1840668714974));
#26434=CARTESIAN_POINT('Ctrl Pts',(1.30174584143096,1.51305702122177,10.1885201476126));
#26435=CARTESIAN_POINT('Ctrl Pts',(1.2481272981871,1.557572549363,10.1929734237278));
#26436=CARTESIAN_POINT('Ctrl Pts',(1.1924342393508,1.59910229420256,10.1974266998431));
#26437=CARTESIAN_POINT('Ctrl Pts',(1.16261220789733,1.62134027830216,10.1998113011409));
#26438=CARTESIAN_POINT('Ctrl Pts',(1.13219584028356,1.64272289842867,10.2021959024387));
#26439=CARTESIAN_POINT('Ctrl Pts',(1.10123979937559,1.66321930808033,10.2045805037365));
#26440=CARTESIAN_POINT('Ctrl Pts',(1.04341906226252,1.70150319321129,10.2090345424545));
#26441=CARTESIAN_POINT('Ctrl Pts',(0.983485064595533,1.73684415250669,10.2134885811725));
#26442=CARTESIAN_POINT('Ctrl Pts',(0.921769670959649,1.76900204527834,10.2179426198904));
#26443=CARTESIAN_POINT('Ctrl Pts',(0.860147045149284,1.8011115997407,10.2223899634962));
#26444=CARTESIAN_POINT('Ctrl Pts',(0.796748768587733,1.83004735962786,10.226837307102));
#26445=CARTESIAN_POINT('Ctrl Pts',(0.731935254425973,1.85561266050552,10.2312846507077));
#26446=CARTESIAN_POINT('Ctrl Pts',(0.667198148735234,1.88114782252131,10.2357267513525));
#26447=CARTESIAN_POINT('Ctrl Pts',(0.601049572350844,1.90332023848129,10.2401688519973));
#26448=CARTESIAN_POINT('Ctrl Pts',(0.533872468206237,1.92198016383921,10.2446109526421));
#26449=CARTESIAN_POINT('Ctrl Pts',(0.466737739676511,1.94062831843354,10.2490502511901));
#26450=CARTESIAN_POINT('Ctrl Pts',(0.398576241062933,1.95576824713277,10.2534895497381));
#26451=CARTESIAN_POINT('Ctrl Pts',(0.329787283400593,1.96729964931814,10.2579288482861));
#26452=CARTESIAN_POINT('Ctrl Pts',(0.261018343465655,1.97882769584188,10.2623668549892));
#26453=CARTESIAN_POINT('Ctrl Pts',(0.191622789532616,1.98674921954684,10.2668048616923));
#26454=CARTESIAN_POINT('Ctrl Pts',(0.122009612528938,1.9910151222305,10.2712428683953));
#26455=CARTESIAN_POINT('Ctrl Pts',(0.0523930390686258,1.99528123304937,
10.2756810916306));
#26456=CARTESIAN_POINT('Ctrl Pts',(-0.017440689752863,1.99589134118134,
10.2801193148659));
#26457=CARTESIAN_POINT('Ctrl Pts',(-0.0870797690490117,1.992848382673,10.2845575381012));
#26458=CARTESIAN_POINT('Ctrl Pts',(-0.156792623264412,1.98980220048593,
10.2890004631443));
#26459=CARTESIAN_POINT('Ctrl Pts',(-0.226309926300341,1.9830952486958,10.2934433881873));
#26460=CARTESIAN_POINT('Ctrl Pts',(-0.295223155529433,1.97278251486048,
10.2978863132303));
#26461=CARTESIAN_POINT('Ctrl Pts',(-0.364176612246978,1.96246376105793,
10.3023318317916));
#26462=CARTESIAN_POINT('Ctrl Pts',(-0.432524813455108,1.94853513354754,
10.3067773503528));
#26463=CARTESIAN_POINT('Ctrl Pts',(-0.499870373652458,1.93110257936873,
10.3112228689141));
#26464=CARTESIAN_POINT('Ctrl Pts',(-0.567333453732282,1.91363960489625,
10.3156761450293));
#26465=CARTESIAN_POINT('Ctrl Pts',(-0.633789933410183,1.89266064557725,
10.3201294211446));
#26466=CARTESIAN_POINT('Ctrl Pts',(-0.69885926063248,1.86832098321681,10.3245826972598));
#26467=CARTESIAN_POINT('Ctrl Pts',(-0.733702014175411,1.85528779395321,
10.3269672985576));
#26468=CARTESIAN_POINT('Ctrl Pts',(-0.768147394660999,1.84129180790358,
10.3293518998554));
#26469=CARTESIAN_POINT('Ctrl Pts',(-0.80213987253757,1.82636228262232,10.3317365011532));
#26470=CARTESIAN_POINT('Ctrl Pts',(-0.865632169015673,1.79847641184594,
10.3361905398712));
#26471=CARTESIAN_POINT('Ctrl Pts',(-0.927794322756352,1.76722046645013,
10.3406445785892));
#26472=CARTESIAN_POINT('Ctrl Pts',(-0.9882447582517,1.73274344906799,10.3450986173072));
#26473=CARTESIAN_POINT('Ctrl Pts',(-1.04860432735014,1.69831825599977,10.3495459609129));
#26474=CARTESIAN_POINT('Ctrl Pts',(-1.10725686313481,1.660681841223,10.3539933045187));
#26475=CARTESIAN_POINT('Ctrl Pts',(-1.16384188655351,1.62003074835127,10.3584406481244));
#26476=CARTESIAN_POINT('Ctrl Pts',(-1.22036020204599,1.57942757893949,10.3628827487692));
#26477=CARTESIAN_POINT('Ctrl Pts',(-1.27481545044851,1.53581707437227,10.367324849414));
#26478=CARTESIAN_POINT('Ctrl Pts',(-1.32687440306657,1.48944012333049,10.3717669500588));
#26479=CARTESIAN_POINT('Ctrl Pts',(-1.37890051666667,1.4430924270749,10.3762062486068));
#26480=CARTESIAN_POINT('Ctrl Pts',(-1.42853296843998,1.39398207108725,10.3806455471548));
#26481=CARTESIAN_POINT('Ctrl Pts',(-1.4754712381619,1.34239047518112,10.3850848457029));
#26482=CARTESIAN_POINT('Ctrl Pts',(-1.52239584875132,1.29081389253493,10.3895228524059));
#26483=CARTESIAN_POINT('Ctrl Pts',(-1.56662750439063,1.23675786527721,10.393960859109));
#26484=CARTESIAN_POINT('Ctrl Pts',(-1.60790349286346,1.18053967325859,10.3983988658121));
#26485=CARTESIAN_POINT('Ctrl Pts',(-1.64918149520935,1.12431873833043,10.4028370890474));
#26486=CARTESIAN_POINT('Ctrl Pts',(-1.6875032562771,1.06593582523333,10.4072753122827));
#26487=CARTESIAN_POINT('Ctrl Pts',(-1.72264828852599,1.00573875163408,10.411713535518));
#26488=CARTESIAN_POINT('Ctrl Pts',(-1.75783055305802,0.945477905878553,
10.416156460561));
#26489=CARTESIAN_POINT('Ctrl Pts',(-1.78982912428108,0.883399487218074,
10.420599385604));
#26490=CARTESIAN_POINT('Ctrl Pts',(-1.8184690544081,0.819876735040153,10.425042310647));
#26491=CARTESIAN_POINT('Ctrl Pts',(-1.8471257028412,0.756316902017108,10.4294878292083));
#26492=CARTESIAN_POINT('Ctrl Pts',(-1.87241963029432,0.691311513727324,
10.4339333477696));
#26493=CARTESIAN_POINT('Ctrl Pts',(-1.89422476331989,0.625252036002861,
10.4383788663308));
#26494=CARTESIAN_POINT('Ctrl Pts',(-1.91606794691126,0.55907728264574,10.442832142446));
#26495=CARTESIAN_POINT('Ctrl Pts',(-1.93441005440984,0.491845240301353,
10.4472854185613));
#26496=CARTESIAN_POINT('Ctrl Pts',(-1.94917560477138,0.423959932380545,
10.4517386946765));
#26497=CARTESIAN_POINT('Ctrl Pts',(-1.95708213238025,0.387609302152085,
10.4541232959743));
#26498=CARTESIAN_POINT('Ctrl Pts',(-1.9639640388674,0.351071496725345,10.4565078972722));
#26499=CARTESIAN_POINT('Ctrl Pts',(-1.96981585838471,0.314409043375201,
10.45889249857));
#26500=CARTESIAN_POINT('Ctrl Pts',(-1.98630072391942,0.211129095683448,
10.4656100385816));
#26501=CARTESIAN_POINT('Ctrl Pts',(-1.99466579522122,0.106519654372821,
10.4723275785932));
#26502=CARTESIAN_POINT('Ctrl Pts',(-1.99474936733483,0.00158871561359909,
10.4790451186048));
#26503=CARTESIAN_POINT('',(-1.99474901028124,0.00181008058995216,8.0796215781142));
#26504=CARTESIAN_POINT('Ctrl Pts',(-1.99474944855383,-0.00148323773318863,
9.67792750393623));
#26505=CARTESIAN_POINT('Ctrl Pts',(-1.99486336953519,0.151724713795801,
9.66888523581739));
#26506=CARTESIAN_POINT('Ctrl Pts',(-1.97732707703499,0.304441334498287,
9.6602202180674));
#26507=CARTESIAN_POINT('Ctrl Pts',(-1.93172749597254,0.499691205536763,
9.64826446450008));
#26508=CARTESIAN_POINT('Ctrl Pts',(-1.91934370848134,0.545327112525534,
9.64540865916488));
#26509=CARTESIAN_POINT('Ctrl Pts',(-1.89970424492805,0.608699655848255,
9.6413303975882));
#26510=CARTESIAN_POINT('Ctrl Pts',(-1.89379623677535,0.626839105852974,
9.64014992783809));
#26511=CARTESIAN_POINT('Ctrl Pts',(-1.88299127327452,0.658465810929409,
9.63806704965448));
#26512=CARTESIAN_POINT('Ctrl Pts',(-1.8782072115945,0.671990336719134,9.63716834279593));
#26513=CARTESIAN_POINT('Ctrl Pts',(-1.87104445499723,0.691565216930016,
9.6358554469013));
#26514=CARTESIAN_POINT('Ctrl Pts',(-1.86878132904338,0.697657612615147,
9.63544510599797));
#26515=CARTESIAN_POINT('Ctrl Pts',(-1.8647663648102,0.708306286143245,9.63472482129508));
#26516=CARTESIAN_POINT('Ctrl Pts',(-1.86302749063099,0.712867420196114,
9.63441531338033));
#26517=CARTESIAN_POINT('Ctrl Pts',(-1.85962358977727,0.72169846274358,9.63381411915987));
#26518=CARTESIAN_POINT('Ctrl Pts',(-1.8579605533933,0.725969109700604,9.63352250131237));
#26519=CARTESIAN_POINT('Ctrl Pts',(-1.85350206960992,0.737302747064408,
9.63274622118121));
#26520=CARTESIAN_POINT('Ctrl Pts',(-1.85068099148227,0.744355511834768,
9.6322606978397));
#26521=CARTESIAN_POINT('Ctrl Pts',(-1.84045298877569,0.769508171744016,
9.63052023989566));
#26522=CARTESIAN_POINT('Ctrl Pts',(-1.8328204523368,0.787514555075603,9.62925769992512));
#26523=CARTESIAN_POINT('Ctrl Pts',(-1.75158546050174,0.971580563808394,
9.61617593931634));
#26524=CARTESIAN_POINT('Ctrl Pts',(-1.65590593230408,1.12692811677535,9.60353424567096));
#26525=CARTESIAN_POINT('Ctrl Pts',(-1.49593765891223,1.32141400560299,9.58598725502769));
#26526=CARTESIAN_POINT('Ctrl Pts',(-1.44846449981781,1.37328670888208,9.58111673887083));
#26527=CARTESIAN_POINT('Ctrl Pts',(-1.38075488412061,1.4398445186779,9.57470467126326));
#26528=CARTESIAN_POINT('Ctrl Pts',(-1.36283960395149,1.45681317385472,9.57305451644416));
#26529=CARTESIAN_POINT('Ctrl Pts',(-1.33352065474393,1.48356858302032,9.57043377577451));
#26530=CARTESIAN_POINT('Ctrl Pts',(-1.32231369304064,1.49356607064646,9.56945008067372));
#26531=CARTESIAN_POINT('Ctrl Pts',(-1.30749423639179,1.50648861665987,9.56817394597322));
#26532=CARTESIAN_POINT('Ctrl Pts',(-1.30398328942877,1.50952863910247,9.56787339353341));
#26533=CARTESIAN_POINT('Ctrl Pts',(-1.29854068529335,1.51420806676782,9.56741027341006));
#26534=CARTESIAN_POINT('Ctrl Pts',(-1.29661649785109,1.51585607446859,9.56724707683529));
#26535=CARTESIAN_POINT('Ctrl Pts',(-1.29263640341932,1.51925178036044,9.56691062614857));
#26536=CARTESIAN_POINT('Ctrl Pts',(-1.29058011519985,1.52099895132617,9.56673741410326));
#26537=CARTESIAN_POINT('Ctrl Pts',(-1.28588044539942,1.52497573780478,9.56634292316337));
#26538=CARTESIAN_POINT('Ctrl Pts',(-1.28323481259262,1.52720265090973,9.56612184352126));
#26539=CARTESIAN_POINT('Ctrl Pts',(-1.27633252856082,1.532981923205,9.56554760550749));
#26540=CARTESIAN_POINT('Ctrl Pts',(-1.27206679865696,1.53652346608833,9.56519522332301));
#26541=CARTESIAN_POINT('Ctrl Pts',(-1.24502018350139,1.55878858073761,9.56297634307845));
#26542=CARTESIAN_POINT('Ctrl Pts',(-1.22183981665658,1.57702402741135,9.56114324914027));
#26543=CARTESIAN_POINT('Ctrl Pts',(-1.1122436033823,1.65937287633308,9.55274492284177));
#26544=CARTESIAN_POINT('Ctrl Pts',(-1.02112705945747,1.71694748922594,9.54651209429306));
#26545=CARTESIAN_POINT('Ctrl Pts',(-0.847640943653099,1.8078492242881,9.53515261173411));
#26546=CARTESIAN_POINT('Ctrl Pts',(-0.766850938651475,1.84357059554135,
9.53004181610148));
#26547=CARTESIAN_POINT('Ctrl Pts',(-0.636580822203791,1.89112052854411,
9.52179483033571));
#26548=CARTESIAN_POINT('Ctrl Pts',(-0.588560410152748,1.90661167015163,
9.51875473565148));
#26549=CARTESIAN_POINT('Ctrl Pts',(-0.510881436795937,1.92845614645175,
9.51380052290897));
#26550=CARTESIAN_POINT('Ctrl Pts',(-0.481574526245821,1.93598263761458,
9.51192342289343));
#26551=CARTESIAN_POINT('Ctrl Pts',(-0.443666096149035,1.94480412887344,
9.50948074370206));
#26552=CARTESIAN_POINT('Ctrl Pts',(-0.435210621159321,1.94671374782314,
9.50893498088891));
#26553=CARTESIAN_POINT('Ctrl Pts',(-0.421539082459801,1.9497078614206,9.50805095112077));
#26554=CARTESIAN_POINT('Ctrl Pts',(-0.416330587801435,1.95082669237658,
9.50771378704969));
#26555=CARTESIAN_POINT('Ctrl Pts',(-0.406377063005334,1.95292312084013,
9.50706872451976));
#26556=CARTESIAN_POINT('Ctrl Pts',(-0.40163282429066,1.95390432391677,9.50676094398615));
#26557=CARTESIAN_POINT('Ctrl Pts',(-0.390765200748853,1.95611071190383,
9.50605516097626));
#26558=CARTESIAN_POINT('Ctrl Pts',(-0.384639566684875,1.95732443953873,
9.50565679564035));
#26559=CARTESIAN_POINT('Ctrl Pts',(-0.365741056470827,1.96097683191608,
9.50442604439248));
#26560=CARTESIAN_POINT('Ctrl Pts',(-0.35295015794745,1.96331933938194,9.50359060745366));
#26561=CARTESIAN_POINT('Ctrl Pts',(-0.212729013835741,1.98758470919543,
9.49440389526563));
#26562=CARTESIAN_POINT('Ctrl Pts',(-0.0835038945242882,1.99718852518692,
9.48565250788074));
#26563=CARTESIAN_POINT('Ctrl Pts',(0.199241833779904,1.99070637977901,9.46604142701777));
#26564=CARTESIAN_POINT('Ctrl Pts',(0.351849080245797,1.9694709525747,9.45515173709032));
#26565=CARTESIAN_POINT('Ctrl Pts',(0.512109552224375,1.92793020432786,9.44418031865727));
#26566=CARTESIAN_POINT('Ctrl Pts',(0.523678643368025,1.92481992944447,9.44339126209958));
#26567=CARTESIAN_POINT('Ctrl Pts',(0.540984731063669,1.91999971399818,9.4422160844827));
#26568=CARTESIAN_POINT('Ctrl Pts',(0.546742962334904,1.91836793037592,9.44182593098086));
#26569=CARTESIAN_POINT('Ctrl Pts',(0.557069618074718,1.91539126041386,9.4411278976481));
#26570=CARTESIAN_POINT('Ctrl Pts',(0.561640707318694,1.91405589178286,9.44081949860981));
#26571=CARTESIAN_POINT('Ctrl Pts',(0.569101392256097,1.91184734727703,9.44031715321085));
#26572=CARTESIAN_POINT('Ctrl Pts',(0.57199383216599,1.91098396911628,9.44012264630375));
#26573=CARTESIAN_POINT('Ctrl Pts',(0.577468076498849,1.90933639351579,9.43975500622046));
#26574=CARTESIAN_POINT('Ctrl Pts',(0.580050219461494,1.90855353238875,9.439581800778));
#26575=CARTESIAN_POINT('Ctrl Pts',(0.585937042773836,1.90675569884789,9.43918738597544));
#26576=CARTESIAN_POINT('Ctrl Pts',(0.589240671398546,1.90573737560933,9.4389663755741));
#26577=CARTESIAN_POINT('Ctrl Pts',(0.599355158121452,1.90259083184598,9.43829069211669));
#26578=CARTESIAN_POINT('Ctrl Pts',(0.606157351188761,1.90043462089591,9.4378376292902));
#26579=CARTESIAN_POINT('Ctrl Pts',(0.660146832836769,1.88300125697074,9.43425128168266));
#26580=CARTESIAN_POINT('Ctrl Pts',(0.706765523435961,1.86600402430718,9.4312131466318));
#26581=CARTESIAN_POINT('Ctrl Pts',(0.779133320424617,1.83651658718984,9.42651872848952));
#26582=CARTESIAN_POINT('Ctrl Pts',(0.805327206027938,1.82518221225195,9.42482422109435));
#26583=CARTESIAN_POINT('Ctrl Pts',(0.95484966681138,1.75663634334875,9.41513065598344));
#26584=CARTESIAN_POINT('Ctrl Pts',(1.07231442600455,1.687498914872,9.40740715138574));
#26585=CARTESIAN_POINT('Ctrl Pts',(1.25047742352823,1.55646834964144,9.39432100124064));
#26586=CARTESIAN_POINT('Ctrl Pts',(1.31580481980559,1.50164655647361,9.38917315177025));
#26587=CARTESIAN_POINT('Ctrl Pts',(1.38581084034302,1.43481370363919,9.38312228310928));
#26588=CARTESIAN_POINT('Ctrl Pts',(1.39412881194766,1.42673294487213,9.38239419207877));
#26589=CARTESIAN_POINT('Ctrl Pts',(1.40661567089511,1.41438872416205,9.38128698759398));
#26590=CARTESIAN_POINT('Ctrl Pts',(1.41083677900199,1.41017824774195,9.38091020358462));
#26591=CARTESIAN_POINT('Ctrl Pts',(1.41840166453435,1.40256445251813,9.38023039137447));
#26592=CARTESIAN_POINT('Ctrl Pts',(1.42175224075325,1.39916792797931,9.379927666485));
#26593=CARTESIAN_POINT('Ctrl Pts',(1.42892689674726,1.39184250043757,9.37927590381884));
#26594=CARTESIAN_POINT('Ctrl Pts',(1.43274702059242,1.38790979399437,9.3789266966069));
#26595=CARTESIAN_POINT('Ctrl Pts',(1.44304976063602,1.37721555804097,9.37797893727992));
#26596=CARTESIAN_POINT('Ctrl Pts',(1.44950097864109,1.37042409966146,9.37737903229982));
#26597=CARTESIAN_POINT('Ctrl Pts',(1.47868666582193,1.33926250709052,9.37463514795554));
#26598=CARTESIAN_POINT('Ctrl Pts',(1.50085486365954,1.31437162691787,9.37246727035655));
#26599=CARTESIAN_POINT('Ctrl Pts',(1.52668728368815,1.28386049386743,9.36983604305288));
#26600=CARTESIAN_POINT('Ctrl Pts',(1.530960988755,1.27876122832517,9.36939714683275));
#26601=CARTESIAN_POINT('Ctrl Pts',(1.6667754524153,1.11505446950515,9.35533393798749));
#26602=CARTESIAN_POINT('Ctrl Pts',(1.77296149708675,0.937049072963789,9.34066303333356));
#26603=CARTESIAN_POINT('Ctrl Pts',(1.86475313706949,0.709422682285681,9.32384215273139));
#26604=CARTESIAN_POINT('Ctrl Pts',(1.87842333062044,0.672392009293282,9.32116778176887));
#26605=CARTESIAN_POINT('Ctrl Pts',(1.89544833692532,0.621690929561978,9.3176106430329));
#26606=CARTESIAN_POINT('Ctrl Pts',(1.89976994451975,0.608356961732152,9.3166847887765));
#26607=CARTESIAN_POINT('Ctrl Pts',(1.90688191491739,0.585598408311192,9.31512216619474));
#26608=CARTESIAN_POINT('Ctrl Pts',(1.90974376681167,0.576196917699078,9.3144817304523));
#26609=CARTESIAN_POINT('Ctrl Pts',(1.9136549941804,0.562998786128454,9.31359013646199));
#26610=CARTESIAN_POINT('Ctrl Pts',(1.91476272412859,0.559219796566307,9.31333570308313));
#26611=CARTESIAN_POINT('Ctrl Pts',(1.91663149301684,0.552773890202215,9.31290319515993));
#26612=CARTESIAN_POINT('Ctrl Pts',(1.91739817080719,0.550108633486317,9.31272479335456));
#26613=CARTESIAN_POINT('Ctrl Pts',(1.91885361076846,0.545008975550902,9.31238427857065));
#26614=CARTESIAN_POINT('Ctrl Pts',(1.91954330093344,0.542574860279767,9.31222211047175));
#26615=CARTESIAN_POINT('Ctrl Pts',(1.92116396323076,0.536813307652533,9.31183910197306));
#26616=CARTESIAN_POINT('Ctrl Pts',(1.92209092835677,0.533484736852513,9.31161849454324));
#26617=CARTESIAN_POINT('Ctrl Pts',(1.92482763183762,0.523557982274807,9.31096251287666));
#26618=CARTESIAN_POINT('Ctrl Pts',(1.92661210011941,0.516952794753302,9.31052856908641));
#26619=CARTESIAN_POINT('Ctrl Pts',(1.95931462873756,0.393383164968282,9.30245552124495));
#26620=CARTESIAN_POINT('Ctrl Pts',(1.97956778746662,0.273834093442378,9.29539201102278));
#26621=CARTESIAN_POINT('Ctrl Pts',(1.99659794082646,0.052703355300665,9.2825133151697));
#26622=CARTESIAN_POINT('Ctrl Pts',(1.99671137894172,-0.0482030712533112,
9.27670469174242));
#26623=CARTESIAN_POINT('Ctrl Pts',(1.98537697876301,-0.199845422790136,
9.26766790235005));
#26624=CARTESIAN_POINT('Ctrl Pts',(1.97958048428358,-0.250839473240393,
9.2645776546791));
#26625=CARTESIAN_POINT('Ctrl Pts',(1.96719463000029,-0.331829966342706,
9.25954889572562));
#26626=CARTESIAN_POINT('Ctrl Pts',(1.96186740813082,-0.36199717175393,9.25764885547487));
#26627=CARTESIAN_POINT('Ctrl Pts',(1.95413690913784,-0.400564977595431,
9.25518035314113));
#26628=CARTESIAN_POINT('Ctrl Pts',(1.95237002626808,-0.409090011598,9.25463223447236));
#26629=CARTESIAN_POINT('Ctrl Pts',(1.94943037190413,-0.422820597511132,
9.25374531146253));
#26630=CARTESIAN_POINT('Ctrl Pts',(1.9482924087709,-0.428033551961868,9.25340762333217));
#26631=CARTESIAN_POINT('Ctrl Pts',(1.94608178495891,-0.437968833899344,
9.25276217215791));
#26632=CARTESIAN_POINT('Ctrl Pts',(1.94501281473625,-0.442691950512122,
9.25245452962264));
#26633=CARTESIAN_POINT('Ctrl Pts',(1.94252965578907,-0.453480862444908,
9.25174993034045));
#26634=CARTESIAN_POINT('Ctrl Pts',(1.94110423975489,-0.45954399699574,9.25135261503699));
#26635=CARTESIAN_POINT('Ctrl Pts',(1.9366347083908,-0.478163676977603,9.25012827452099));
#26636=CARTESIAN_POINT('Ctrl Pts',(1.93349702260022,-0.490697204252851,
9.24929824414072));
#26637=CARTESIAN_POINT('Ctrl Pts',(1.9024132313487,-0.609932528231575,9.24134433307812));
#26638=CARTESIAN_POINT('Ctrl Pts',(1.86578895098847,-0.714155400904201,
9.23393437542665));
#26639=CARTESIAN_POINT('Ctrl Pts',(1.75049223543347,-0.971795668455693,
9.21448487254357));
#26640=CARTESIAN_POINT('Ctrl Pts',(1.66023016327808,-1.11903825025194,9.20221411777309));
#26641=CARTESIAN_POINT('Ctrl Pts',(1.54047957564099,-1.26739831390781,9.18956985716378));
#26642=CARTESIAN_POINT('Ctrl Pts',(1.52855488167458,-1.28175498627609,9.18834386125351));
#26643=CARTESIAN_POINT('Ctrl Pts',(1.51317003808025,-1.29975735275129,9.18680571452252));
#26644=CARTESIAN_POINT('Ctrl Pts',(1.50989570677115,-1.30355962509467,9.18648079599734));
#26645=CARTESIAN_POINT('Ctrl Pts',(1.50463601229805,-1.30962096699599,9.18596281283034));
#26646=CARTESIAN_POINT('Ctrl Pts',(1.50265985434682,-1.31188794076649,9.18576908020964));
#26647=CARTESIAN_POINT('Ctrl Pts',(1.49889083893141,-1.31619192331911,9.18540127419574));
#26648=CARTESIAN_POINT('Ctrl Pts',(1.49709897390799,-1.31822971763192,9.18522713491098));
#26649=CARTESIAN_POINT('Ctrl Pts',(1.49297019082687,-1.32290588994334,9.18482753253087));
#26650=CARTESIAN_POINT('Ctrl Pts',(1.4906304364177,-1.32554173334375,9.18460228456331));
#26651=CARTESIAN_POINT('Ctrl Pts',(1.48436043481582,-1.3325675894896,9.18400183547347));
#26652=CARTESIAN_POINT('Ctrl Pts',(1.48041766471036,-1.3369464540924,9.1836275539037));
#26653=CARTESIAN_POINT('Ctrl Pts',(1.45228802088711,-1.36791038759687,9.1809800082683));
#26654=CARTESIAN_POINT('Ctrl Pts',(1.42740413507433,-1.39385693296275,9.1787566260397));
#26655=CARTESIAN_POINT('Ctrl Pts',(1.34747306490184,-1.47281427228912,9.1719207254313));
#26656=CARTESIAN_POINT('Ctrl Pts',(1.29007038151825,-1.52334693184688,9.16744040352308));
#26657=CARTESIAN_POINT('Ctrl Pts',(1.14781660199042,-1.63475261993657,9.15692783015908));
#26658=CARTESIAN_POINT('Ctrl Pts',(1.06081636022466,-1.69250317833966,9.15093547937382));
#26659=CARTESIAN_POINT('Ctrl Pts',(0.920949581230171,-1.77030837267695,
9.14145738766702));
#26660=CARTESIAN_POINT('Ctrl Pts',(0.871084241938938,-1.79536942107091,
9.13810794791522));
#26661=CARTESIAN_POINT('Ctrl Pts',(0.79057738974391,-1.83168601482136,9.13269576415827));
#26662=CARTESIAN_POINT('Ctrl Pts',(0.760596270751748,-1.84433711367415,
9.13067950184846));
#26663=CARTESIAN_POINT('Ctrl Pts',(0.722046727561138,-1.85950400284161,
9.12808047227522));
#26664=CARTESIAN_POINT('Ctrl Pts',(0.713751442382475,-1.86270381106109,
9.12752082905616));
#26665=CARTESIAN_POINT('Ctrl Pts',(0.700405721877602,-1.86774952768151,
9.12661975012612));
#26666=CARTESIAN_POINT('Ctrl Pts',(0.695368667308701,-1.86963068251336,
9.12627949674023));
#26667=CARTESIAN_POINT('Ctrl Pts',(0.685789263783826,-1.87316417087338,
9.12563207607209));
#26668=CARTESIAN_POINT('Ctrl Pts',(0.681248387359192,-1.87482040724166,
9.12532504174964));
#26669=CARTESIAN_POINT('Ctrl Pts',(0.670913657572252,-1.87854738647071,
9.12462591112992));
#26670=CARTESIAN_POINT('Ctrl Pts',(0.665116174512405,-1.88060785176839,
9.12423347623666));
#26671=CARTESIAN_POINT('Ctrl Pts',(0.647477075305257,-1.88678514180739,
9.12303868461662));
#26672=CARTESIAN_POINT('Ctrl Pts',(0.635606275763195,-1.89081712089569,
9.12223352953804));
#26673=CARTESIAN_POINT('Ctrl Pts',(0.47442830436635,-1.94387274980272,9.11128508193633));
#26674=CARTESIAN_POINT('Ctrl Pts',(0.319907204669216,-1.97518669737377,
9.1005327593222));
#26675=CARTESIAN_POINT('Ctrl Pts',(0.072849997082817,-1.99548641573738,
9.08325253933275));
#26676=CARTESIAN_POINT('Ctrl Pts',(-0.0180556654180757,-1.99673444006547,
9.07689179547007));
#26677=CARTESIAN_POINT('Ctrl Pts',(-0.142959150029688,-1.98991586999494,
9.06835712747401));
#26678=CARTESIAN_POINT('Ctrl Pts',(-0.177133731720543,-1.98716542376212,
9.06604396697868));
#26679=CARTESIAN_POINT('Ctrl Pts',(-0.230279291309521,-1.98150606657555,
9.06249739820565));
#26680=CARTESIAN_POINT('Ctrl Pts',(-0.24930678216805,-1.97920212188548,
9.06123783706724));
#26681=CARTESIAN_POINT('Ctrl Pts',(-0.273316924148852,-1.97594308252605,
9.05966382509495));
#26682=CARTESIAN_POINT('Ctrl Pts',(-0.278332345629832,-1.9752428491579,
9.05933588499108));
#26683=CARTESIAN_POINT('Ctrl Pts',(-0.286332198725828,-1.97409486623535,
9.05881422209364));
#26684=CARTESIAN_POINT('Ctrl Pts',(-0.289318332913555,-1.97365943654459,
9.05861981483929));
#26685=CARTESIAN_POINT('Ctrl Pts',(-0.294985115165702,-1.9728199850055,
9.05825150292939));
#26686=CARTESIAN_POINT('Ctrl Pts',(-0.297665894506263,-1.97241728007503,
9.05807752915041));
#26687=CARTESIAN_POINT('Ctrl Pts',(-0.303811081637851,-1.97148134032565,
9.05767931879889));
#26688=CARTESIAN_POINT('Ctrl Pts',(-0.307274907112855,-1.97094443871356,
9.05745529228092));
#26689=CARTESIAN_POINT('Ctrl Pts',(-0.318223443835052,-1.96921782389349,
9.05674849518524));
#26690=CARTESIAN_POINT('Ctrl Pts',(-0.325702911167279,-1.96799456712226,
9.05626758716477));
#26691=CARTESIAN_POINT('Ctrl Pts',(-0.453220567830481,-1.94639232860153,
9.04809888668501));
#26692=CARTESIAN_POINT('Ctrl Pts',(-0.571172712391881,-1.91510403723221,
9.04099376209606));
#26693=CARTESIAN_POINT('Ctrl Pts',(-0.779933774678313,-1.83870399558062,
9.02808645854503));
#26694=CARTESIAN_POINT('Ctrl Pts',(-0.871570354730636,-1.79707903400079,
9.02229133038076));
#26695=CARTESIAN_POINT('Ctrl Pts',(-1.00437090827061,-1.72420008152258,
9.0132867311369));
#26696=CARTESIAN_POINT('Ctrl Pts',(-1.04810636664026,-1.69796916664244,
9.01021525285886));
#26697=CARTESIAN_POINT('Ctrl Pts',(-1.11631514555335,-1.65342001699696,
9.00521437845527));
#26698=CARTESIAN_POINT('Ctrl Pts',(-1.14145666655364,-1.63616434928798,
9.0033229059394));
#26699=CARTESIAN_POINT('Ctrl Pts',(-1.17324377663589,-1.61325824248199,
9.00086404565769));
#26700=CARTESIAN_POINT('Ctrl Pts',(-1.1802623499166,-1.60813055995689,9.00031680362441));
#26701=CARTESIAN_POINT('Ctrl Pts',(-1.19153231654802,-1.59978334090053,
8.9994309572435));
#26702=CARTESIAN_POINT('Ctrl Pts',(-1.19580475716871,-1.59659230269748,
8.9990934641401));
#26703=CARTESIAN_POINT('Ctrl Pts',(-1.20393313536772,-1.5904703788967,8.9984481581691));
#26704=CARTESIAN_POINT('Ctrl Pts',(-1.20779129986291,-1.58754250207034,
8.99814046485042));
#26705=CARTESIAN_POINT('Ctrl Pts',(-1.21659132142224,-1.58081371070847,
8.99743542782099));
#26706=CARTESIAN_POINT('Ctrl Pts',(-1.22152607962585,-1.57700363558835,
8.99703772396178));
#26707=CARTESIAN_POINT('Ctrl Pts',(-1.23665677514264,-1.56520775393851,
8.99581101343834));
#26708=CARTESIAN_POINT('Ctrl Pts',(-1.24679270414512,-1.55714586093694,
8.99497898469379));
#26709=CARTESIAN_POINT('Ctrl Pts',(-1.34444847600975,-1.47790784283936,
8.98686092462547));
#26710=CARTESIAN_POINT('Ctrl Pts',(-1.42584483262181,-1.39953987839287,
8.97927500335886));
#26711=CARTESIAN_POINT('Ctrl Pts',(-1.60699211115646,-1.19284135629211,
8.96031864009634));
#26712=CARTESIAN_POINT('Ctrl Pts',(-1.69855689737891,-1.05839469840758,
8.94878479315759));
#26713=CARTESIAN_POINT('Ctrl Pts',(-1.78433229483724,-0.892083856917428,
8.93628676229934));
#26714=CARTESIAN_POINT('Ctrl Pts',(-1.79539736412924,-0.86959979057228,
8.9346326838636));
#26715=CARTESIAN_POINT('Ctrl Pts',(-1.80838328685275,-0.841907360617288,
8.93264373074597));
#26716=CARTESIAN_POINT('Ctrl Pts',(-1.81070933271269,-0.836892962225977,
8.93228549014198));
#26717=CARTESIAN_POINT('Ctrl Pts',(-1.81431587354054,-0.829032695963559,
8.9317269888164));
#26718=CARTESIAN_POINT('Ctrl Pts',(-1.81561056280657,-0.826193430445362,
8.93152586944803));
#26719=CARTESIAN_POINT('Ctrl Pts',(-1.81801013270286,-0.820898271314013,
8.93115195878283));
#26720=CARTESIAN_POINT('Ctrl Pts',(-1.81911669125897,-0.818443204000036,
8.93097906729748));
#26721=CARTESIAN_POINT('Ctrl Pts',(-1.821608295118,-0.812885187404918,8.93058871376438));
#26722=CARTESIAN_POINT('Ctrl Pts',(-1.82299038184303,-0.809780943757151,
8.9303714348269));
#26723=CARTESIAN_POINT('Ctrl Pts',(-1.82704226519411,-0.800617241873368,
8.92973216490358));
#26724=CARTESIAN_POINT('Ctrl Pts',(-1.82968986340451,-0.794547930283797,
8.92931151022863));
#26725=CARTESIAN_POINT('Ctrl Pts',(-1.84771682724285,-0.752655243065184,
8.92642611871348));
#26726=CARTESIAN_POINT('Ctrl Pts',(-1.86207456535152,-0.716398067446356,
8.92401987158389));
#26727=CARTESIAN_POINT('Ctrl Pts',(-1.93366208434713,-0.518892600116926,
8.91127701331208));
#26728=CARTESIAN_POINT('Ctrl Pts',(-1.97103251553399,-0.351200055704026,
8.9016911687405));
#26729=CARTESIAN_POINT('Ctrl Pts',(-1.99199024446832,-0.12090296704569,
8.88803967058595));
#26730=CARTESIAN_POINT('Ctrl Pts',(-1.9947289275133,-0.0608133368123225,
8.88444065486108));
#26731=CARTESIAN_POINT('Ctrl Pts',(-1.99476161125608,0.0329699460048473,
8.87870197308211));
#26732=CARTESIAN_POINT('Ctrl Pts',(-1.99392110303576,0.0666282866475172,
8.87661823930357));
#26733=CARTESIAN_POINT('Ctrl Pts',(-1.99176245128306,0.109527292600944,
8.87392530536294));
#26734=CARTESIAN_POINT('Ctrl Pts',(-1.99123068921559,0.118803315593194,
8.8733408047614));
#26735=CARTESIAN_POINT('Ctrl Pts',(-1.99027977418863,0.133583105184661,
8.87240584832657));
#26736=CARTESIAN_POINT('Ctrl Pts',(-1.98990254356016,0.139089509561404,
8.87205670925127));
#26737=CARTESIAN_POINT('Ctrl Pts',(-1.98915357968622,0.149394661073251,
8.87140175749735));
#26738=CARTESIAN_POINT('Ctrl Pts',(-1.98878732072905,0.154193776062166,
8.87109611897631));
#26739=CARTESIAN_POINT('Ctrl Pts',(-1.98793081888436,0.164905490873897,
8.87041250649036));
#26740=CARTESIAN_POINT('Ctrl Pts',(-1.98743156075167,0.170817304926972,
8.87003425176789));
#26741=CARTESIAN_POINT('Ctrl Pts',(-1.98589097350591,0.188137840307838,
8.86892314950701));
#26742=CARTESIAN_POINT('Ctrl Pts',(-1.98477773979606,0.199539770771446,
8.86818804918902));
#26743=CARTESIAN_POINT('Ctrl Pts',(-1.97508248833094,0.290712470781469,
8.86227979049387));
#26744=CARTESIAN_POINT('Ctrl Pts',(-1.96179425111047,0.369898507814767,
8.85695840979102));
#26745=CARTESIAN_POINT('Ctrl Pts',(-1.9207610851264,0.547908397673107,8.84455584237897));
#26746=CARTESIAN_POINT('Ctrl Pts',(-1.89008778119344,0.645826338051234,
8.83740989865913));
#26747=CARTESIAN_POINT('Ctrl Pts',(-1.80895452013098,0.848623136024026,
8.82217341303137));
#26748=CARTESIAN_POINT('Ctrl Pts',(-1.75656177873735,0.952352465779989,
8.81411058645937));
#26749=CARTESIAN_POINT('Ctrl Pts',(-1.69139590018277,1.05748121009304,8.80603352311556));
#26750=CARTESIAN_POINT('Ctrl Pts',(-1.6873099296381,1.06398863098044,8.80553401987475));
#26751=CARTESIAN_POINT('Ctrl Pts',(-1.68129477589268,1.07344672143961,8.80480889054404));
#26752=CARTESIAN_POINT('Ctrl Pts',(-1.67939527370162,1.07641604519397,8.80458136472026));
#26753=CARTESIAN_POINT('Ctrl Pts',(-1.67601953023632,1.08166235972264,8.80417960732177));
#26754=CARTESIAN_POINT('Ctrl Pts',(-1.67454650238217,1.08394139043119,8.80400516397716));
#26755=CARTESIAN_POINT('Ctrl Pts',(-1.67143129852943,1.08873964734929,8.80363807338506));
#26756=CARTESIAN_POINT('Ctrl Pts',(-1.66978807940505,1.09125816174925,8.80344549790757));
#26757=CARTESIAN_POINT('Ctrl Pts',(-1.66538832820323,1.09796832689279,8.80293266143679));
#26758=CARTESIAN_POINT('Ctrl Pts',(-1.66262164532838,1.10215334521897,8.80261307400977));
#26759=CARTESIAN_POINT('Ctrl Pts',(-1.649494892678,1.12184759452823,8.80111013527543));
#26760=CARTESIAN_POINT('Ctrl Pts',(-1.63893300793373,1.13722209028045,8.79993980505107));
#26761=CARTESIAN_POINT('Ctrl Pts',(-1.52880177567023,1.29281355286047,8.78810141382086));
#26762=CARTESIAN_POINT('Ctrl Pts',(-1.41169775995678,1.41976397825655,8.77843980124234));
#26763=CARTESIAN_POINT('Ctrl Pts',(-1.19512894980028,1.60089393871845,8.76192491045458));
#26764=CARTESIAN_POINT('Ctrl Pts',(-1.10480549707487,1.66451021201874,8.75534717208111));
#26765=CARTESIAN_POINT('Ctrl Pts',(-0.998552948221976,1.72687188638907,
8.74765682610446));
#26766=CARTESIAN_POINT('Ctrl Pts',(-0.987346840240081,1.73330340880107,
8.7468465121535));
#26767=CARTESIAN_POINT('Ctrl Pts',(-0.970647350391145,1.74267325624923,
8.74563975210611));
#26768=CARTESIAN_POINT('Ctrl Pts',(-0.965201257934812,1.74569553104751,
8.74524632182401));
#26769=CARTESIAN_POINT('Ctrl Pts',(-0.955495897152954,1.75102215971219,
8.74454537470062));
#26770=CARTESIAN_POINT('Ctrl Pts',(-0.951242205081797,1.75333661339536,
8.74423822151205));
#26771=CARTESIAN_POINT('Ctrl Pts',(-0.942284050171711,1.75816859290734,
8.74359147037491));
#26772=CARTESIAN_POINT('Ctrl Pts',(-0.937577836024628,1.76068277460109,
8.7432517566204));
#26773=CARTESIAN_POINT('Ctrl Pts',(-0.925166217813102,1.76724950933876,
8.74235596188253));
#26774=CARTESIAN_POINT('Ctrl Pts',(-0.917444337608731,1.77127051639334,
8.74179877111921));
#26775=CARTESIAN_POINT('Ctrl Pts',(-0.882436955258173,1.78920954343265,
8.73927309228567));
#26776=CARTESIAN_POINT('Ctrl Pts',(-0.854860650210472,1.80254788160963,
8.73728444286876));
#26777=CARTESIAN_POINT('Ctrl Pts',(-0.780301653924716,1.83651546453293,
8.73190664659693));
#26778=CARTESIAN_POINT('Ctrl Pts',(-0.732814385000913,1.85597468827633,
8.72847992372128));
#26779=CARTESIAN_POINT('Ctrl Pts',(-0.589948609551209,1.90817988266176,
8.71817056031528));
#26780=CARTESIAN_POINT('Ctrl Pts',(-0.49278504584196,1.93554886662691,8.71115099238238));
#26781=CARTESIAN_POINT('Ctrl Pts',(-0.310560107016956,1.97226295060287,
8.69818173724003));
#26782=CARTESIAN_POINT('Ctrl Pts',(-0.226145848879563,1.98371586973232,
8.69225142046983));
#26783=CARTESIAN_POINT('Ctrl Pts',(-0.104001861381776,1.99238697340105,
8.68397475229841));
#26784=CARTESIAN_POINT('Ctrl Pts',(-0.0666802713103355,1.99398506090668,
8.6814869693489));
#26785=CARTESIAN_POINT('Ctrl Pts',(-0.0233728218016821,1.99462197052304,
8.67866417476682));
#26786=CARTESIAN_POINT('Ctrl Pts',(-0.0174121730664553,1.99468291026621,
8.67827706458009));
#26787=CARTESIAN_POINT('Ctrl Pts',(-0.00790675197565317,1.99473747888062,
8.67766208035376));
#26788=CARTESIAN_POINT('Ctrl Pts',(-0.00436217265854273,1.99474837969709,
8.67743327078668));
#26789=CARTESIAN_POINT('Ctrl Pts',(0.00189891029603759,1.99475094580639,
8.67703004386315));
#26790=CARTESIAN_POINT('Ctrl Pts',(0.00461538983852243,1.99474651025942,
8.6768554094708));
#26791=CARTESIAN_POINT('Ctrl Pts',(0.0103288690540395,1.99472550966838,
8.67648877198016));
#26792=CARTESIAN_POINT('Ctrl Pts',(0.0133258358558936,1.99470773970702,
8.67629683738261));
#26793=CARTESIAN_POINT('Ctrl Pts',(0.0212939527049333,1.99464253547758,
8.67578752598992));
#26794=CARTESIAN_POINT('Ctrl Pts',(0.0262650249644415,1.99458327138868,
8.67547080654992));
#26795=CARTESIAN_POINT('Ctrl Pts',(0.049403338615265,1.99422090297092,8.67400116187692));
#26796=CARTESIAN_POINT('Ctrl Pts',(0.0675668319085981,1.99368815999893,
8.67286056755772));
#26797=CARTESIAN_POINT('Ctrl Pts',(0.24167046082842,1.98619940962763,8.66203128675586));
#26798=CARTESIAN_POINT('Ctrl Pts',(0.396316964882176,1.96120890941292,8.65317990975153));
#26799=CARTESIAN_POINT('Ctrl Pts',(0.668225200603352,1.88375322562802,8.63672065419262));
#26800=CARTESIAN_POINT('Ctrl Pts',(0.786370314024065,1.83757067680839,8.62923327181646));
#26801=CARTESIAN_POINT('Ctrl Pts',(0.910950587665771,1.77464529714492,8.62052209064799));
#26802=CARTESIAN_POINT('Ctrl Pts',(0.922508174800024,1.76866490848215,8.61970602907216));
#26803=CARTESIAN_POINT('Ctrl Pts',(0.939525742298678,1.75964711296118,8.61849233979297));
#26804=CARTESIAN_POINT('Ctrl Pts',(0.945031456888975,1.7566963672311,8.61809777903834));
#26805=CARTESIAN_POINT('Ctrl Pts',(0.954782650850639,1.75141118107601,8.6173955581035));
#26806=CARTESIAN_POINT('Ctrl Pts',(0.959033675027193,1.74908703186797,8.61708826636628));
#26807=CARTESIAN_POINT('Ctrl Pts',(0.967940320115646,1.7441752978075,8.61644197698908));
#26808=CARTESIAN_POINT('Ctrl Pts',(0.972594122218522,1.74158450995239,8.61610286640846));
#26809=CARTESIAN_POINT('Ctrl Pts',(0.984790676098834,1.7347305135737,8.61521036886468));
#26810=CARTESIAN_POINT('Ctrl Pts',(0.99231606140882,1.73043678324184,8.61465588688509));
#26811=CARTESIAN_POINT('Ctrl Pts',(1.02595719426972,1.71095068204773,8.6121598239611));
#26812=CARTESIAN_POINT('Ctrl Pts',(1.05175254864138,1.69521585962313,8.61019865661296));
#26813=CARTESIAN_POINT('Ctrl Pts',(1.11955391700747,1.65171466421718,8.6049129604975));
#26814=CARTESIAN_POINT('Ctrl Pts',(1.16088057742308,1.62293495655182,8.6015524203319));
#26815=CARTESIAN_POINT('Ctrl Pts',(1.28094406655226,1.53238955643415,8.59136816200825));
#26816=CARTESIAN_POINT('Ctrl Pts',(1.35616534088264,1.46623589685976,8.58440720851115));
#26817=CARTESIAN_POINT('Ctrl Pts',(1.51227094783563,1.30661869258721,8.56882970224325));
#26818=CARTESIAN_POINT('Ctrl Pts',(1.59010087746871,1.21070330433734,8.56023316941198));
#26819=CARTESIAN_POINT('Ctrl Pts',(1.6627831072815,1.10192422069179,8.55169187303433));
#26820=CARTESIAN_POINT('Ctrl Pts',(1.66694507816974,1.0956179812349,8.55120077147977));
#26821=CARTESIAN_POINT('Ctrl Pts',(1.67298290993694,1.0863553751997,8.55048554142526));
#26822=CARTESIAN_POINT('Ctrl Pts',(1.67488691736652,1.08341757077333,8.55025958471084));
#26823=CARTESIAN_POINT('Ctrl Pts',(1.67825123673067,1.07819650084249,8.54985961483974));
#26824=CARTESIAN_POINT('Ctrl Pts',(1.67971463947711,1.07591525609307,8.54968539635086));
#26825=CARTESIAN_POINT('Ctrl Pts',(1.68279889422886,1.07108569443712,8.5493177112261));
#26826=CARTESIAN_POINT('Ctrl Pts',(1.68441860539452,1.06853668413568,8.54912432046628));
#26827=CARTESIAN_POINT('Ctrl Pts',(1.68874437851215,1.06169474812195,8.54860699794448));
#26828=CARTESIAN_POINT('Ctrl Pts',(1.69143988087485,1.05739512240872,8.54828376061073));
#26829=CARTESIAN_POINT('Ctrl Pts',(1.70429856525839,1.03670910262367,8.54673729501149));
#26830=CARTESIAN_POINT('Ctrl Pts',(1.71424062576099,1.02018552572916,8.54552802047596));
#26831=CARTESIAN_POINT('Ctrl Pts',(1.7413353765104,0.973639573314195,8.54218603395861));
#26832=CARTESIAN_POINT('Ctrl Pts',(1.75795009904916,0.943310476370931,8.54008194936214));
#26833=CARTESIAN_POINT('Ctrl Pts',(1.8157046992711,0.831051579067874,8.53250257829814));
#26834=CARTESIAN_POINT('Ctrl Pts',(1.85197481438699,0.746740811799411,8.52720246169032));
#26835=CARTESIAN_POINT('Ctrl Pts',(1.93387666849153,0.51323801473111,8.5128510081281));
#26836=CARTESIAN_POINT('Ctrl Pts',(1.96803229135681,0.360737933199634,8.50377564713194));
#26837=CARTESIAN_POINT('Ctrl Pts',(1.98540009027258,0.193318909351684,8.49326493829502));
#26838=CARTESIAN_POINT('Ctrl Pts',(1.98657939738878,0.18079824526646,8.49247601157161));
#26839=CARTESIAN_POINT('Ctrl Pts',(1.98815988852135,0.162128877200572,8.49129507007666));
#26840=CARTESIAN_POINT('Ctrl Pts',(1.98865111940251,0.155987945249319,8.49090588447729));
#26841=CARTESIAN_POINT('Ctrl Pts',(1.98947704983553,0.145024143425738,8.49020969148506));
#26842=CARTESIAN_POINT('Ctrl Pts',(1.98982267983578,0.140202126002045,8.48990302979203));
#26843=CARTESIAN_POINT('Ctrl Pts',(1.99051539237544,0.130018840068612,8.48925440513547));
#26844=CARTESIAN_POINT('Ctrl Pts',(1.99085835083834,0.12465733842149,8.4889123152375));
#26845=CARTESIAN_POINT('Ctrl Pts',(1.99171018317356,0.110439161075678,8.48800353259536));
#26846=CARTESIAN_POINT('Ctrl Pts',(1.99218163615962,0.101580442934999,8.48743567116195));
#26847=CARTESIAN_POINT('Ctrl Pts',(1.99409664364856,0.0604256341091231,
8.48478972903826));
#26848=CARTESIAN_POINT('Ctrl Pts',(1.99481396211781,0.0281022087461893,
8.48268906038251));
#26849=CARTESIAN_POINT('Ctrl Pts',(1.99462848562754,-0.0595109098138776,
8.4769303124561));
#26850=CARTESIAN_POINT('Ctrl Pts',(1.99221291203987,-0.114765515024974,
8.47322777901343));
#26851=CARTESIAN_POINT('Ctrl Pts',(1.97865686090083,-0.273397295996829,
8.46240256571958));
#26852=CARTESIAN_POINT('Ctrl Pts',(1.96172880981232,-0.376092937774062,
8.45514507698912));
#26853=CARTESIAN_POINT('Ctrl Pts',(1.91982084963911,-0.546264644558422,
8.44292368359057));
#26854=CARTESIAN_POINT('Ctrl Pts',(1.89905641030154,-0.614575560317481,
8.43796567661446));
#26855=CARTESIAN_POINT('Ctrl Pts',(1.87180631681041,-0.689520967815815,
8.43255693756747));
#26856=CARTESIAN_POINT('Ctrl Pts',(1.86888752402926,-0.697393346221799,
8.43198921226483));
#26857=CARTESIAN_POINT('Ctrl Pts',(1.85393830506228,-0.736945483102642,
8.42913973618636));
#26858=CARTESIAN_POINT('Ctrl Pts',(1.84115083480158,-0.768335750457242,
8.42688751182878));
#26859=CARTESIAN_POINT('Ctrl Pts',(1.82524927528295,-0.804690093931946,
8.42430240594606));
#26860=CARTESIAN_POINT('Ctrl Pts',(1.82290662936808,-0.809983016368391,
8.42392662198763));
#26861=CARTESIAN_POINT('Ctrl Pts',(1.81911300946868,-0.818454414053066,
8.42332620723367));
#26862=CARTESIAN_POINT('Ctrl Pts',(1.81767668725229,-0.821639355299856,
8.42310070797001));
#26863=CARTESIAN_POINT('Ctrl Pts',(1.81511170099361,-0.827287384048021,
8.4227012573476));
#26864=CARTESIAN_POINT('Ctrl Pts',(1.81398637935532,-0.829751962185732,
8.42252710253392));
#26865=CARTESIAN_POINT('Ctrl Pts',(1.81159442905761,-0.834962472968344,
8.42215923527944));
#26866=CARTESIAN_POINT('Ctrl Pts',(1.81032658033501,-0.837707812718036,
8.42196559993562));
#26867=CARTESIAN_POINT('Ctrl Pts',(1.806907079768,-0.845068219551413,8.42144693106417));
#26868=CARTESIAN_POINT('Ctrl Pts',(1.80474397342986,-0.849677987449023,
8.42112259827667));
#26869=CARTESIAN_POINT('Ctrl Pts',(1.79422248832292,-0.871878733638613,
8.4195628079825));
#26870=CARTESIAN_POINT('Ctrl Pts',(1.78562408911488,-0.889355690942119,
8.41834159660963));
#26871=CARTESIAN_POINT('Ctrl Pts',(1.76083223517264,-0.937937594563641,
8.41495799131184));
#26872=CARTESIAN_POINT('Ctrl Pts',(1.74407198214679,-0.968746776647528,
8.41282509621319));
#26873=CARTESIAN_POINT('Ctrl Pts',(1.67937658776836,-1.08054446994269,8.40507465326996));
#26874=CARTESIAN_POINT('Ctrl Pts',(1.62653889385068,-1.15855758517278,8.39964068520289));
#26875=CARTESIAN_POINT('Ctrl Pts',(1.47417826549765,-1.35243202908758,8.38533812765868));
#26876=CARTESIAN_POINT('Ctrl Pts',(1.36655174808003,-1.46109588468636,8.3764396728853));
#26877=CARTESIAN_POINT('Ctrl Pts',(1.23772448628793,-1.56436126146682,8.36613057473746));
#26878=CARTESIAN_POINT('Ctrl Pts',(1.22776438609564,-1.5721904021998,8.36533588962999));
#26879=CARTESIAN_POINT('Ctrl Pts',(1.21283657536215,-1.58369605148948,8.36414799128888));
#26880=CARTESIAN_POINT('Ctrl Pts',(1.20792513076438,-1.58744531216401,8.36375765691701));
#26881=CARTESIAN_POINT('Ctrl Pts',(1.1991383696673,-1.59408849350911,8.36306018192563));
#26882=CARTESIAN_POINT('Ctrl Pts',(1.19526978170201,-1.59699126579369,8.36275339186002));
#26883=CARTESIAN_POINT('Ctrl Pts',(1.18708993489509,-1.60308259384868,8.36210529679687));
#26884=CARTESIAN_POINT('Ctrl Pts',(1.18277630545501,-1.60626788754496,8.36176386793664));
#26885=CARTESIAN_POINT('Ctrl Pts',(1.17150393293358,-1.6145216663641,8.36087250536558));
#26886=CARTESIAN_POINT('Ctrl Pts',(1.16452518652817,-1.61956252183275,8.36032150811027));
#26887=CARTESIAN_POINT('Ctrl Pts',(1.14915316373773,-1.6305152447406,8.35910958069409));
#26888=CARTESIAN_POINT('Ctrl Pts',(1.14074647789215,-1.63640778037673,8.35844792822141));
#26889=CARTESIAN_POINT('Ctrl Pts',(1.11577752559575,-1.65362347355213,8.35648586631564));
#26890=CARTESIAN_POINT('Ctrl Pts',(1.09908988997372,-1.66476167784118,8.35517856503502));
#26891=CARTESIAN_POINT('Ctrl Pts',(1.03959916074087,-1.70318453369781,8.35053104701778));
#26892=CARTESIAN_POINT('Ctrl Pts',(0.995928506377608,-1.72908347034398,
8.34714205558288));
#26893=CARTESIAN_POINT('Ctrl Pts',(0.819951350029455,-1.82456737958286,
8.33357818182985));
#26894=CARTESIAN_POINT('Ctrl Pts',(0.680992712462007,-1.88085271223676,
8.32302151972718));
#26895=CARTESIAN_POINT('Ctrl Pts',(0.466750660034543,-1.94074825477413,
8.30765391027668));
#26896=CARTESIAN_POINT('Ctrl Pts',(0.3953883743506,-1.95653535277602,8.30268566346477));
#26897=CARTESIAN_POINT('Ctrl Pts',(0.315812298603969,-1.96960603556065,
8.29741940566992));
#26898=CARTESIAN_POINT('Ctrl Pts',(0.308304314995621,-1.97079521948055,
8.29692521328095));
#26899=CARTESIAN_POINT('Ctrl Pts',(0.297266882110772,-1.97247881138701,
8.29620281578304));
#26900=CARTESIAN_POINT('Ctrl Pts',(0.293742725015352,-1.97300670869494,
8.29597277504676));
#26901=CARTESIAN_POINT('Ctrl Pts',(0.287526788764371,-1.97392079444671,
8.2955681331199));
#26902=CARTESIAN_POINT('Ctrl Pts',(0.284835611458565,-1.97431092582046,
8.29539330984282));
#26903=CARTESIAN_POINT('Ctrl Pts',(0.279186049892442,-1.9751181325976,8.29502708018251));
#26904=CARTESIAN_POINT('Ctrl Pts',(0.276227530411742,-1.97553406447497,
8.29483573923658));
#26905=CARTESIAN_POINT('Ctrl Pts',(0.268385272949907,-1.97661862922778,
8.29432969271231));
#26906=CARTESIAN_POINT('Ctrl Pts',(0.263499933038235,-1.97727581451999,
8.29401562961622));
#26907=CARTESIAN_POINT('Ctrl Pts',(0.241393976438014,-1.98016616580136,
8.29259963257806));
#26908=CARTESIAN_POINT('Ctrl Pts',(0.224146437898077,-1.98219260412814,
8.29150889652619));
#26909=CARTESIAN_POINT('Ctrl Pts',(0.17702406174122,-1.98710612367152,8.28856177474792));
#26910=CARTESIAN_POINT('Ctrl Pts',(0.147106050608735,-1.98954474101159,
8.28672659729548));
#26911=CARTESIAN_POINT('Ctrl Pts',(0.0438186785867573,-1.99562083486986,
8.28047989771616));
#26912=CARTESIAN_POINT('Ctrl Pts',(-0.0296930805824241,-1.99588136608064,
8.27618697264572));
#26913=CARTESIAN_POINT('Ctrl Pts',(-0.231585628778115,-1.98543690349676,
8.26443880589486));
#26914=CARTESIAN_POINT('Ctrl Pts',(-0.359160631457635,-1.96636536369612,
8.2570428749965));
#26915=CARTESIAN_POINT('Ctrl Pts',(-0.489150578478365,-1.93385299103681,
8.24897111936738));
#26916=CARTESIAN_POINT('Ctrl Pts',(-0.494289470719627,-1.93254588504606,
8.24865116903215));
#26917=CARTESIAN_POINT('Ctrl Pts',(-0.547488380592045,-1.91878837140432,
8.24532988630469));
#26918=CARTESIAN_POINT('Ctrl Pts',(-0.595069395803439,-1.90456927310555,
8.24228172938183));
#26919=CARTESIAN_POINT('Ctrl Pts',(-0.651222371040707,-1.88547884652929,
8.23856989857006));
#26920=CARTESIAN_POINT('Ctrl Pts',(-0.66035416690302,-1.88230003618962,
8.23796260912844));
#26921=CARTESIAN_POINT('Ctrl Pts',(-0.675234450898315,-1.87699854683614,
8.23696688406439));
#26922=CARTESIAN_POINT('Ctrl Pts',(-0.6809969788628,-1.87491552394316,8.23657976593404));
#26923=CARTESIAN_POINT('Ctrl Pts',(-0.691285142901009,-1.87114289920849,
8.23588587099605));
#26924=CARTESIAN_POINT('Ctrl Pts',(-0.695814430400161,-1.86946333899012,
8.23557943115927));
#26925=CARTESIAN_POINT('Ctrl Pts',(-0.705385772902589,-1.86587447100627,
8.23492980894162));
#26926=CARTESIAN_POINT('Ctrl Pts',(-0.71042626958217,-1.86396114356299,
8.23458649397921));
#26927=CARTESIAN_POINT('Ctrl Pts',(-0.72338041391765,-1.8589836884265,8.23370102251431));
#26928=CARTESIAN_POINT('Ctrl Pts',(-0.731282313437865,-1.8558894771609,
8.23315785919395));
#26929=CARTESIAN_POINT('Ctrl Pts',(-0.767162417072151,-1.84157488672986,
8.23067747780603));
#26930=CARTESIAN_POINT('Ctrl Pts',(-0.794902547802253,-1.82977212014478,
8.22872069884412));
#26931=CARTESIAN_POINT('Ctrl Pts',(-0.868280492224898,-1.79656801944158,
8.22343593686068));
#26932=CARTESIAN_POINT('Ctrl Pts',(-0.913390069155155,-1.77405905319881,
8.22007172664467));
#26933=CARTESIAN_POINT('Ctrl Pts',(-1.03576364877011,-1.7070914519208,8.21062386344293));
#26934=CARTESIAN_POINT('Ctrl Pts',(-1.11097090444453,-1.65912890939449,
8.20444247386381));
#26935=CARTESIAN_POINT('Ctrl Pts',(-1.28321835246041,-1.53230394471539,
8.18952343736462));
#26936=CARTESIAN_POINT('Ctrl Pts',(-1.37656523210199,-1.44902690209786,
8.1807785162497));
#26937=CARTESIAN_POINT('Ctrl Pts',(-1.47114728672341,-1.34720199912272,
8.17161054949819));
#26938=CARTESIAN_POINT('Ctrl Pts',(-1.48066192470102,-1.33673776714208,
8.17068461922947));
#26939=CARTESIAN_POINT('Ctrl Pts',(-1.49319634116289,-1.32265431466557,
8.16946092396867));
#26940=CARTESIAN_POINT('Ctrl Pts',(-1.49631545968456,-1.31912463231378,
8.16915608689455));
#26941=CARTESIAN_POINT('Ctrl Pts',(-1.50116706651944,-1.31359506746867,
8.16868146333302));
#26942=CARTESIAN_POINT('Ctrl Pts',(-1.50290810217116,-1.31160275979795,
8.16851104631438));
#26943=CARTESIAN_POINT('Ctrl Pts',(-1.50624488345896,-1.3077690356633,8.16818426126638));
#26944=CARTESIAN_POINT('Ctrl Pts',(-1.50784120043325,-1.30592818100249,
8.16802785236674));
#26945=CARTESIAN_POINT('Ctrl Pts',(-1.51165353612885,-1.30151552959572,
8.16765412854783));
#26946=CARTESIAN_POINT('Ctrl Pts',(-1.51386636423064,-1.29894099894453,
8.1674370514186));
#26947=CARTESIAN_POINT('Ctrl Pts',(-1.52050779157342,-1.29117395897596,
8.16678502410681));
#26948=CARTESIAN_POINT('Ctrl Pts',(-1.52491638398229,-1.28596429253909,
8.16635152416989));
#26949=CARTESIAN_POINT('Ctrl Pts',(-1.55774099516945,-1.24676903601589,
8.16311781141746));
#26950=CARTESIAN_POINT('Ctrl Pts',(-1.58504705682597,-1.21186491114171,
8.16039348472467));
#26951=CARTESIAN_POINT('Ctrl Pts',(-1.65353669864764,-1.11803734452872,
8.15338136523548));
#26952=CARTESIAN_POINT('Ctrl Pts',(-1.69273901638744,-1.05774626794611,
8.14917900838138));
#26953=CARTESIAN_POINT('Ctrl Pts',(-1.76233778252968,-0.936889740923381,
8.14107225821186));
#26954=CARTESIAN_POINT('Ctrl Pts',(-1.79307195736845,-0.876635450618172,
8.13717013608704));
#26955=CARTESIAN_POINT('Ctrl Pts',(-1.86718057963606,-0.711066236539654,
8.12657180756088));
#26956=CARTESIAN_POINT('Ctrl Pts',(-1.90469293798104,-0.603421726607212,
8.11979724302245));
#26957=CARTESIAN_POINT('Ctrl Pts',(-1.9360277503575,-0.480616404137664,
8.11188639262492));
#26958=CARTESIAN_POINT('Ctrl Pts',(-1.93910989809191,-0.468026034075575,
8.11107349899703));
#26959=CARTESIAN_POINT('Ctrl Pts',(-1.94349290696159,-0.449334818143309,
8.1098636284517));
#26960=CARTESIAN_POINT('Ctrl Pts',(-1.94488825177285,-0.443256297063917,
8.10946969024776));
#26961=CARTESIAN_POINT('Ctrl Pts',(-1.94731658958484,-0.432445514673095,
8.10876817118136));
#26962=CARTESIAN_POINT('Ctrl Pts',(-1.94836089968368,-0.427715825214534,
8.10846095612334));
#26963=CARTESIAN_POINT('Ctrl Pts',(-1.95051849723119,-0.417772161922642,
8.10781441431247));
#26964=CARTESIAN_POINT('Ctrl Pts',(-1.95162812643588,-0.412557441470851,
8.10747497304597));
#26965=CARTESIAN_POINT('Ctrl Pts',(-1.95383722178578,-0.401967381924348,
8.10678484522419));
#26966=CARTESIAN_POINT('Ctrl Pts',(-1.95493544207345,-0.396591832612719,
8.10643412198102));
#26967=CARTESIAN_POINT('Ctrl Pts',(-1.95759428288649,-0.383297953845802,
8.10556572686589));
#26968=CARTESIAN_POINT('Ctrl Pts',(-1.95912904073472,-0.375374608062704,
8.10504723430336));
#26969=CARTESIAN_POINT('Ctrl Pts',(-1.96623800066139,-0.337442286318332,
8.10256045980665));
#26970=CARTESIAN_POINT('Ctrl Pts',(-1.97117077455213,-0.307318691573248,
8.10057196547371));
#26971=CARTESIAN_POINT('Ctrl Pts',(-1.98837368424034,-0.184679196643107,
8.09241690771572));
#26972=CARTESIAN_POINT('Ctrl Pts',(-1.99483390533887,-0.0914821070513714,
8.08607550797391));
#26973=CARTESIAN_POINT('Ctrl Pts',(-1.99474917736509,0.00181160185376153,
8.07962176510059));
#26974=CARTESIAN_POINT('Ctrl Pts',(-1.99474917872771,0.00181010085837489,
8.07962186893436));
#26975=CARTESIAN_POINT('Ctrl Pts',(-1.9946025293401,0.163419186970004,8.06844230140074));
#26976=CARTESIAN_POINT('Ctrl Pts',(-1.97481767100195,0.324419899408584,
8.05695069916315));
#26977=CARTESIAN_POINT('Ctrl Pts',(-1.93294149260101,0.492856029737398,
8.04544972196648));
#26978=CARTESIAN_POINT('Ctrl Pts',(-1.92995930451566,0.504407552142277,
8.04466399087229));
#26979=CARTESIAN_POINT('Ctrl Pts',(-1.92533025109995,0.521695880331543,
8.04349328407203));
#26980=CARTESIAN_POINT('Ctrl Pts',(-1.92376104353685,0.527452952278365,
8.04310431076097));
#26981=CARTESIAN_POINT('Ctrl Pts',(-1.92083256771947,0.538009938727879,
8.04239275368518));
#26982=CARTESIAN_POINT('Ctrl Pts',(-1.91948108787714,0.542811939781313,
8.04206974689217));
#26983=CARTESIAN_POINT('Ctrl Pts',(-1.91728779025176,0.550494411208243,
8.04155409221742));
#26984=CARTESIAN_POINT('Ctrl Pts',(-1.91645747300161,0.553378100297498,
8.04136078670241));
#26985=CARTESIAN_POINT('Ctrl Pts',(-1.91486342421142,0.558867607301989,
8.04099329444896));
#26986=CARTESIAN_POINT('Ctrl Pts',(-1.91410088865785,0.561473707303415,
8.04081904387778));
#26987=CARTESIAN_POINT('Ctrl Pts',(-1.91233280873882,0.567470970047757,
8.04041853087533));
#26988=CARTESIAN_POINT('Ctrl Pts',(-1.91132356510089,0.570861019151871,
8.04019248688016));
#26989=CARTESIAN_POINT('Ctrl Pts',(-1.90859668106549,0.579932321825721,
8.03958852422362));
#26990=CARTESIAN_POINT('Ctrl Pts',(-1.90686267654961,0.585608678036491,
8.03921154215899));
#26991=CARTESIAN_POINT('Ctrl Pts',(-1.89419058119865,0.626438338313878,
8.03650619561362));
#26992=CARTESIAN_POINT('Ctrl Pts',(-1.88230565389973,0.66129327250839,8.03423019557212));
#26993=CARTESIAN_POINT('Ctrl Pts',(-1.86528982749034,0.707010941722775,
8.03126481654285));
#26994=CARTESIAN_POINT('Ctrl Pts',(-1.86101705341103,0.718182532563603,
8.0305418025732));
#26995=CARTESIAN_POINT('Ctrl Pts',(-1.84774248716042,0.751976072845238,
8.02835770295901));
#26996=CARTESIAN_POINT('Ctrl Pts',(-1.83842659081066,0.7744727598571,8.02690780186416));
#26997=CARTESIAN_POINT('Ctrl Pts',(-1.79448605436488,0.875319537144692,
8.02040335955909));
#26998=CARTESIAN_POINT('Ctrl Pts',(-1.75524759950036,0.951562643050326,
8.01546884739643));
#26999=CARTESIAN_POINT('Ctrl Pts',(-1.68091433781392,1.07565534714707,8.00706789488677));
#27000=CARTESIAN_POINT('Ctrl Pts',(-1.64837179985535,1.12488995013763,8.00362780691618));
#27001=CARTESIAN_POINT('Ctrl Pts',(-1.56949188028581,1.23344132063484,7.99567643151273));
#27002=CARTESIAN_POINT('Ctrl Pts',(-1.52188725163734,1.2917195962136,7.99113573531167));
#27003=CARTESIAN_POINT('Ctrl Pts',(-1.46022150789559,1.35905874779749,7.98545699528291));
#27004=CARTESIAN_POINT('Ctrl Pts',(-1.44918883549138,1.37081699255257,7.98444836763508));
#27005=CARTESIAN_POINT('Ctrl Pts',(-1.43432196233404,1.38628152546335,7.98309825374717));
#27006=CARTESIAN_POINT('Ctrl Pts',(-1.43061348903908,1.39010827044605,7.98276220790587));
#27007=CARTESIAN_POINT('Ctrl Pts',(-1.42373137236618,1.39715316628911,7.98213990366135));
#27008=CARTESIAN_POINT('Ctrl Pts',(-1.42056203155644,1.40037548703302,7.98185383421981));
#27009=CARTESIAN_POINT('Ctrl Pts',(-1.41398765699366,1.40701447617827,7.98126146095665));
#27010=CARTESIAN_POINT('Ctrl Pts',(-1.41058112968504,1.41042961760265,7.98095509223284));
#27011=CARTESIAN_POINT('Ctrl Pts',(-1.40286737486535,1.41810698104987,7.9802626114396));
#27012=CARTESIAN_POINT('Ctrl Pts',(-1.39855306062161,1.42236198502735,7.97987618528826));
#27013=CARTESIAN_POINT('Ctrl Pts',(-1.38746237706074,1.43320095667876,7.97888500699063));
#27014=CARTESIAN_POINT('Ctrl Pts',(-1.38065855552888,1.43975649952544,7.97827902368101));
#27015=CARTESIAN_POINT('Ctrl Pts',(-1.34032739810685,1.47806714801907,7.97469873357842));
#27016=CARTESIAN_POINT('Ctrl Pts',(-1.30575454047324,1.50869629807674,7.97167672610601));
#27017=CARTESIAN_POINT('Ctrl Pts',(-1.26283585013824,1.54413834072007,7.96797671452249));
#27018=CARTESIAN_POINT('Ctrl Pts',(-1.25547638730432,1.55012794174535,7.96734402969188));
#27019=CARTESIAN_POINT('Ctrl Pts',(-1.22679009621421,1.57313638715877,7.96488475978215));
#27020=CARTESIAN_POINT('Ctrl Pts',(-1.20515839703623,1.58976890294754,7.96304477372632));
#27021=CARTESIAN_POINT('Ctrl Pts',(-1.10753266317454,1.66169515020721,7.95480713527513));
#27022=CARTESIAN_POINT('Ctrl Pts',(-1.02803304333606,1.71201776459951,7.94826585803189));
#27023=CARTESIAN_POINT('Ctrl Pts',(-0.876291992230998,1.79367760921354,
7.9362428620975));
#27024=CARTESIAN_POINT('Ctrl Pts',(-0.805162579032059,1.82671330701595,
7.93077786864641));
#27025=CARTESIAN_POINT('Ctrl Pts',(-0.702994978091094,1.86703406455688,
7.9233041551115));
#27026=CARTESIAN_POINT('Ctrl Pts',(-0.673447865357886,1.87789412473065,
7.92118540627067));
#27027=CARTESIAN_POINT('Ctrl Pts',(-0.6266526728255,1.89384704910893,7.91790909128924));
#27028=CARTESIAN_POINT('Ctrl Pts',(-0.609572626527827,1.89941345849472,
7.9167295592809));
#27029=CARTESIAN_POINT('Ctrl Pts',(-0.587650386738246,1.9062317605298,7.91523843614937));
#27030=CARTESIAN_POINT('Ctrl Pts',(-0.582876158117747,1.90769701144958,
7.91491507263978));
#27031=CARTESIAN_POINT('Ctrl Pts',(-0.575223208898215,1.91001435457658,
7.91439898346653));
#27032=CARTESIAN_POINT('Ctrl Pts',(-0.572348019207229,1.91087789247409,
7.91420559824399));
#27033=CARTESIAN_POINT('Ctrl Pts',(-0.566868807868184,1.91251004929935,
7.91383804783387));
#27034=CARTESIAN_POINT('Ctrl Pts',(-0.564265198602791,1.91327983309568,
7.91366381842855));
#27035=CARTESIAN_POINT('Ctrl Pts',(-0.558268311546124,1.91503956846406,
7.91326347715789));
#27036=CARTESIAN_POINT('Ctrl Pts',(-0.554873970463672,1.91602581763185,
7.91303758310535));
#27037=CARTESIAN_POINT('Ctrl Pts',(-0.545780922296382,1.91864167516669,
7.91243428278966));
#27038=CARTESIAN_POINT('Ctrl Pts',(-0.540077489353895,1.92025493110966,
7.91205780989862));
#27039=CARTESIAN_POINT('Ctrl Pts',(-0.499056828586545,1.93166069346229,
7.90936343277446));
#27040=CARTESIAN_POINT('Ctrl Pts',(-0.463480176268807,1.94050439091535,
7.90709741710329));
#27041=CARTESIAN_POINT('Ctrl Pts',(-0.357583343705635,1.96374937824469,
7.90050569743404));
#27042=CARTESIAN_POINT('Ctrl Pts',(-0.286704296100162,1.97534294145181,
7.8962899757783));
#27043=CARTESIAN_POINT('Ctrl Pts',(-0.0893911502836425,1.99676974638069,
7.88473122412065));
#27044=CARTESIAN_POINT('Ctrl Pts',(0.0375774038532549,1.99841604968019,
7.87747373598929));
#27045=CARTESIAN_POINT('Ctrl Pts',(0.207362399899169,1.98442314765283,7.86728265923098));
#27046=CARTESIAN_POINT('Ctrl Pts',(0.250750109838614,1.97940859373567,7.86463756706073));
#27047=CARTESIAN_POINT('Ctrl Pts',(0.311766672483799,1.97031827015229,7.86084012952415));
#27048=CARTESIAN_POINT('Ctrl Pts',(0.329559825385252,1.96742034981685,7.8597233972209));
#27049=CARTESIAN_POINT('Ctrl Pts',(0.360680664408105,1.96191777649685,7.85775243846465));
#27050=CARTESIAN_POINT('Ctrl Pts',(0.37402574833505,1.95941742069155,7.85690150559883));
#27051=CARTESIAN_POINT('Ctrl Pts',(0.393572800850712,1.95554808966998,7.85564625189801));
#27052=CARTESIAN_POINT('Ctrl Pts',(0.399795608883394,1.95428538094766,7.85524531920287));
#27053=CARTESIAN_POINT('Ctrl Pts',(0.410788306005286,1.95200008375483,7.85453468121337));
#27054=CARTESIAN_POINT('Ctrl Pts',(0.415560694392999,1.95098966371247,7.85422536725562));
#27055=CARTESIAN_POINT('Ctrl Pts',(0.424815090048621,1.9489948073615,7.85362399355915));
#27056=CARTESIAN_POINT('Ctrl Pts',(0.429297504977026,1.94801238997494,7.85333200030103));
#27057=CARTESIAN_POINT('Ctrl Pts',(0.44122022567228,1.94535612033029,7.85255340612052));
#27058=CARTESIAN_POINT('Ctrl Pts',(0.4486543330149,1.94365506436704,7.85206593458927));
#27059=CARTESIAN_POINT('Ctrl Pts',(0.475306606335467,1.93739549638792,7.85031098214982));
#27060=CARTESIAN_POINT('Ctrl Pts',(0.494466059297516,1.93259435706872,7.84903572782634));
#27061=CARTESIAN_POINT('Ctrl Pts',(0.518108170231655,1.9262953390674,7.8474445873111));
#27062=CARTESIAN_POINT('Ctrl Pts',(0.522661483108442,1.92506487756013,7.84713733540794));
#27063=CARTESIAN_POINT('Ctrl Pts',(0.532138269811713,1.92246782349646,7.84649615864681));
#27064=CARTESIAN_POINT('Ctrl Pts',(0.537060937400058,1.9210984408134,7.84616214695425));
#27065=CARTESIAN_POINT('Ctrl Pts',(0.746345873839542,1.86201249870024,7.83192089689819));
#27066=CARTESIAN_POINT('Ctrl Pts',(0.940164487803027,1.77205301469311,7.81685369619351));
#27067=CARTESIAN_POINT('Ctrl Pts',(1.1532751652314,1.6281882477511,7.79916118757827));
#27068=CARTESIAN_POINT('Ctrl Pts',(1.18960682236419,1.6018354348985,7.7961081150366));
#27069=CARTESIAN_POINT('Ctrl Pts',(1.24322178798088,1.56011505952547,7.79158010553127));
#27070=CARTESIAN_POINT('Ctrl Pts',(1.26117648862968,1.54563688869602,7.79005977236567));
#27071=CARTESIAN_POINT('Ctrl Pts',(1.28303408269369,1.5273769826986,7.78820814173184));
#27072=CARTESIAN_POINT('Ctrl Pts',(1.28717707353678,1.52388716368912,7.78785713867878));
#27073=CARTESIAN_POINT('Ctrl Pts',(1.29366567441279,1.51837619553806,7.7873074238131));
#27074=CARTESIAN_POINT('Ctrl Pts',(1.29602084360717,1.51636642062099,7.78710789644053));
#27075=CARTESIAN_POINT('Ctrl Pts',(1.30041801124789,1.51259638588108,7.78673539416489));
#27076=CARTESIAN_POINT('Ctrl Pts',(1.30246109770228,1.51083748949078,7.78656232628851));
#27077=CARTESIAN_POINT('Ctrl Pts',(1.30709781903029,1.50682933330186,7.78616956982153));
#27078=CARTESIAN_POINT('Ctrl Pts',(1.30968921108559,1.50457752176844,7.78595007376364));
#27079=CARTESIAN_POINT('Ctrl Pts',(1.31638831081193,1.49872586197163,7.78538263175004));
#27080=CARTESIAN_POINT('Ctrl Pts',(1.32048710376361,1.495115783026,7.78503543205357));
#27081=CARTESIAN_POINT('Ctrl Pts',(1.34561738247554,1.47279792261024,7.78290623279078));
#27082=CARTESIAN_POINT('Ctrl Pts',(1.36626702633225,1.45366243325787,7.78115462483105));
#27083=CARTESIAN_POINT('Ctrl Pts',(1.52841096151801,1.29689909791467,7.7673169105405));
#27084=CARTESIAN_POINT('Ctrl Pts',(1.64918321079767,1.13938744966882,7.75638668982092));
#27085=CARTESIAN_POINT('Ctrl Pts',(1.76937324823784,0.922444401457525,7.7416392628026));
#27086=CARTESIAN_POINT('Ctrl Pts',(1.79218957401354,0.877292033853806,7.73859148550451));
#27087=CARTESIAN_POINT('Ctrl Pts',(1.82589766243223,0.80376873190401,7.73362584582013));
#27088=CARTESIAN_POINT('Ctrl Pts',(1.83790051631615,0.775930399940775,7.73174522202751));
#27089=CARTESIAN_POINT('Ctrl Pts',(1.85251591493174,0.739788882466196,7.72929857487841));
#27090=CARTESIAN_POINT('Ctrl Pts',(1.85571536734314,0.731726231095351,7.72875244837687));
#27091=CARTESIAN_POINT('Ctrl Pts',(1.86079517630101,0.718677444068249,7.72786797196837));
#27092=CARTESIAN_POINT('Ctrl Pts',(1.86270834192547,0.713704132522616,7.72753072699844));
#27093=CARTESIAN_POINT('Ctrl Pts',(1.86632270786699,0.704194987350592,7.72688560477938));
#27094=CARTESIAN_POINT('Ctrl Pts',(1.86802735942135,0.699660499015529,7.72657784585518));
#27095=CARTESIAN_POINT('Ctrl Pts',(1.87189071716629,0.689268939315709,7.72587224707978));
#27096=CARTESIAN_POINT('Ctrl Pts',(1.87403847334495,0.683407877242711,7.72547404503841));
#27097=CARTESIAN_POINT('Ctrl Pts',(1.88057105385983,0.665318592664034,7.72424429204972));
#27098=CARTESIAN_POINT('Ctrl Pts',(1.88486389381281,0.653057736258307,7.72340969724007));
#27099=CARTESIAN_POINT('Ctrl Pts',(1.93000999235424,0.519960857251873,7.71433674047399));
#27100=CARTESIAN_POINT('Ctrl Pts',(1.9592948635304,0.395537911909164,7.70570965164376));
#27101=CARTESIAN_POINT('Ctrl Pts',(1.99745146459902,0.115380156957704,7.68611358089036));
#27102=CARTESIAN_POINT('Ctrl Pts',(2.00037508819516,-0.0403563045860061,
7.67509902156652));
#27103=CARTESIAN_POINT('Ctrl Pts',(1.98343883447003,-0.212900253517525,
7.66360846772554));
#27104=CARTESIAN_POINT('Ctrl Pts',(1.98142224128465,-0.230915757020227,
7.66241813209591));
#27105=CARTESIAN_POINT('Ctrl Pts',(1.97854046158315,-0.253830410825299,
7.6609182013289));
#27106=CARTESIAN_POINT('Ctrl Pts',(1.97790224697928,-0.258756523134797,
7.66059658440132));
#27107=CARTESIAN_POINT('Ctrl Pts',(1.97684958858511,-0.266650038477074,
7.66008262272875));
#27108=CARTESIAN_POINT('Ctrl Pts',(1.97644685378661,-0.269618941020809,
7.65988962783192));
#27109=CARTESIAN_POINT('Ctrl Pts',(1.97566617639554,-0.275278227902444,
7.65952236046447));
#27110=CARTESIAN_POINT('Ctrl Pts',(1.97528943124526,-0.277968714426434,
7.65934802566489));
#27111=CARTESIAN_POINT('Ctrl Pts',(1.97440821277893,-0.284169577311775,
7.65894683552531));
#27112=CARTESIAN_POINT('Ctrl Pts',(1.97389987403908,-0.287679382476234,
7.65872020107659));
#27113=CARTESIAN_POINT('Ctrl Pts',(1.97251111259077,-0.297091029008319,
7.65811362781496));
#27114=CARTESIAN_POINT('Ctrl Pts',(1.97161355511333,-0.302990363338583,
7.65773463836136));
#27115=CARTESIAN_POINT('Ctrl Pts',(1.96488643825788,-0.34590934590038,7.65498569517072));
#27116=CARTESIAN_POINT('Ctrl Pts',(1.95804068784878,-0.382765063830779,
7.65267001918923));
#27117=CARTESIAN_POINT('Ctrl Pts',(1.93229138985211,-0.502493724484299,
7.64523037877867));
#27118=CARTESIAN_POINT('Ctrl Pts',(1.90912983891965,-0.584359183644491,
7.64027244590276));
#27119=CARTESIAN_POINT('Ctrl Pts',(1.84724716953405,-0.7595123019111,7.62948548526538));
#27120=CARTESIAN_POINT('Ctrl Pts',(1.80652975264624,-0.851839292848211,
7.6236768459733));
#27121=CARTESIAN_POINT('Ctrl Pts',(1.73481795577841,-0.985934399525989,
7.61464001874356));
#27122=CARTESIAN_POINT('Ctrl Pts',(1.70888742779654,-1.03022479743342,7.61154974901048));
#27123=CARTESIAN_POINT('Ctrl Pts',(1.66479580844147,-1.09928193160132,7.60652095730684));
#27124=CARTESIAN_POINT('Ctrl Pts',(1.6477199030193,-1.12471543544125,7.60462090701549));
#27125=CARTESIAN_POINT('Ctrl Pts',(1.62504772493893,-1.15685921912941,7.60215239339524));
#27126=CARTESIAN_POINT('Ctrl Pts',(1.61998311364871,-1.16394074970994,7.60160427371356));
#27127=CARTESIAN_POINT('Ctrl Pts',(1.61174010199157,-1.17530841750219,7.60071734946718));
#27128=CARTESIAN_POINT('Ctrl Pts',(1.60859054000238,-1.17961540610982,7.600379661119));
#27129=CARTESIAN_POINT('Ctrl Pts',(1.60254961938989,-1.18780711001371,7.59973420979597));
#27130=CARTESIAN_POINT('Ctrl Pts',(1.59966131654855,-1.19169403995506,7.59942656733087));
#27131=CARTESIAN_POINT('Ctrl Pts',(1.593025832747,-1.20055614293285,7.59872196858692));
#27132=CARTESIAN_POINT('Ctrl Pts',(1.58926946065408,-1.20552434073758,7.59832465375341));
#27133=CARTESIAN_POINT('Ctrl Pts',(1.57764953090503,-1.2207442207174,7.59710031606074));
#27134=CARTESIAN_POINT('Ctrl Pts',(1.56970971372106,-1.2309369993507,7.59627028805374));
#27135=CARTESIAN_POINT('Ctrl Pts',(1.49304880361492,-1.32740289390338,7.58831656084079));
#27136=CARTESIAN_POINT('Ctrl Pts',(1.41739454947651,-1.40789858258302,7.58090679990818));
#27137=CARTESIAN_POINT('Ctrl Pts',(1.20773035090262,-1.59687097541437,7.5614575864931));
#27138=CARTESIAN_POINT('Ctrl Pts',(1.06561927147637,-1.69501209220942,7.54918691046629));
#27139=CARTESIAN_POINT('Ctrl Pts',(0.896085428783181,-1.78224769282635,
7.53654244970378));
#27140=CARTESIAN_POINT('Ctrl Pts',(0.879369189107662,-1.79055461397138,
7.53531623013543));
#27141=CARTESIAN_POINT('Ctrl Pts',(0.858013412657452,-1.80079585933755,
7.53377784409858));
#27142=CARTESIAN_POINT('Ctrl Pts',(0.853480507869025,-1.80294863136012,
7.53345290517926));
#27143=CARTESIAN_POINT('Ctrl Pts',(0.846217994505851,-1.80636422487075,
7.53293489718037));
#27144=CARTESIAN_POINT('Ctrl Pts',(0.843493607544295,-1.80763800066408,
7.53274116001116));
#27145=CARTESIAN_POINT('Ctrl Pts',(0.838305576563201,-1.81004936016725,
7.53237335064943));
#27146=CARTESIAN_POINT('Ctrl Pts',(0.835842522534803,-1.81118806410125,
7.53219921254341));
#27147=CARTESIAN_POINT('Ctrl Pts',(0.830175094530202,-1.81379417129579,
7.53179961980711));
#27148=CARTESIAN_POINT('Ctrl Pts',(0.826969152283247,-1.81525810975824,
7.53157438026967));
#27149=CARTESIAN_POINT('Ctrl Pts',(0.81676408767738,-1.81988543089769,7.53085989683099));
#27150=CARTESIAN_POINT('Ctrl Pts',(0.809750460589579,-1.82301693702622,
7.5303725734955));
#27151=CARTESIAN_POINT('Ctrl Pts',(0.696330574289468,-1.87287394304048,
7.52254897282997));
#27152=CARTESIAN_POINT('Ctrl Pts',(0.586040790476462,-1.91026122767459,
7.5157428035951));
#27153=CARTESIAN_POINT('Ctrl Pts',(0.373676905080303,-1.96210825393127,
7.50303926839564));
#27154=CARTESIAN_POINT('Ctrl Pts',(0.272529802133945,-1.97869395972625,
7.49714765933331));
#27155=CARTESIAN_POINT('Ctrl Pts',(0.11743306430779,-1.99200405124301,7.48791171169632));
#27156=CARTESIAN_POINT('Ctrl Pts',(0.0641497227846041,-1.99443094861027,
7.48470480224453));
#27157=CARTESIAN_POINT('Ctrl Pts',(-0.0206603140407525,-1.99489166703058,
7.47950309081823));
#27158=CARTESIAN_POINT('Ctrl Pts',(-0.0521548189967926,-1.99431675360186,
7.47755026087937));
#27159=CARTESIAN_POINT('Ctrl Pts',(-0.0924049868206681,-1.99262795614422,
7.47502241075901));
#27160=CARTESIAN_POINT('Ctrl Pts',(-0.101186123352513,-1.99220134967634,
7.4744689740873));
#27161=CARTESIAN_POINT('Ctrl Pts',(-0.115310620668992,-1.99142152652569,
7.47357551926709));
#27162=CARTESIAN_POINT('Ctrl Pts',(-0.120655946880693,-1.99110481319271,
7.47323664764734));
#27163=CARTESIAN_POINT('Ctrl Pts',(-0.130828425318791,-1.99046097519389,
7.4725903012896));
#27164=CARTESIAN_POINT('Ctrl Pts',(-0.135655796568988,-1.99013780297264,
7.47228295284327));
#27165=CARTESIAN_POINT('Ctrl Pts',(-0.146659270269622,-1.98936094536326,
7.47158094174434));
#27166=CARTESIAN_POINT('Ctrl Pts',(-0.152834508065125,-1.98889605666247,
7.47118592996382));
#27167=CARTESIAN_POINT('Ctrl Pts',(-0.171705395743079,-1.98738700034668,
7.46997558648977));
#27168=CARTESIAN_POINT('Ctrl Pts',(-0.184393097421516,-1.98624998557144,
7.46915734852765));
#27169=CARTESIAN_POINT('Ctrl Pts',(-0.209670990787775,-1.9837404111223,
7.46751797197997));
#27170=CARTESIAN_POINT('Ctrl Pts',(-0.222260734065426,-1.98236931395097,
7.46669691583978));
#27171=CARTESIAN_POINT('Ctrl Pts',(-0.38156347461975,-1.96348371749504,
7.45624877698675));
#27172=CARTESIAN_POINT('Ctrl Pts',(-0.52587553495734,-1.92984398222032,
7.44609659852811));
#27173=CARTESIAN_POINT('Ctrl Pts',(-0.748316912022514,-1.85117160980462,
7.42964325228764));
#27174=CARTESIAN_POINT('Ctrl Pts',(-0.829469929568279,-1.81625864781452,
7.42346728003289));
#27175=CARTESIAN_POINT('Ctrl Pts',(-0.937921367151235,-1.76081141297538,
7.41516244500048));
#27176=CARTESIAN_POINT('Ctrl Pts',(-0.967407481519828,-1.74478547793121,
7.41289960836647));
#27177=CARTESIAN_POINT('Ctrl Pts',(-1.01282854440652,-1.71859308378748,
7.40942150905995));
#27178=CARTESIAN_POINT('Ctrl Pts',(-1.02904621907731,-1.70893176901858,
7.40818123109543));
#27179=CARTESIAN_POINT('Ctrl Pts',(-1.04941579923842,-1.69640190399817,
7.40662781135966));
#27180=CARTESIAN_POINT('Ctrl Pts',(-1.05369662289857,-1.69374625248754,
7.40630159716159));
#27181=CARTESIAN_POINT('Ctrl Pts',(-1.06052067691524,-1.68947699812598,
7.40578203600991));
#27182=CARTESIAN_POINT('Ctrl Pts',(-1.06307035713122,-1.68787382509658,
7.40558801402943));
#27183=CARTESIAN_POINT('Ctrl Pts',(-1.06790935240903,-1.68481587560035,
7.40521999250112));
#27184=CARTESIAN_POINT('Ctrl Pts',(-1.07019930282471,-1.68336222244463,
7.40504592567276));
#27185=CARTESIAN_POINT('Ctrl Pts',(-1.07545097219631,-1.68001343204309,
7.40464692703962));
#27186=CARTESIAN_POINT('Ctrl Pts',(-1.07841064781337,-1.67811513329362,
7.40442220816449));
#27187=CARTESIAN_POINT('Ctrl Pts',(-1.08778261404218,-1.67206903807546,
7.40371103035528));
#27188=CARTESIAN_POINT('Ctrl Pts',(-1.09417620866053,-1.66789217649824,
7.40322646692585));
#27189=CARTESIAN_POINT('Ctrl Pts',(-1.199550715814,-1.59818552283159,7.39524751672005));
#27190=CARTESIAN_POINT('Ctrl Pts',(-1.29252888094534,-1.52397412721782,
7.38830656887432));
#27191=CARTESIAN_POINT('Ctrl Pts',(-1.45175047739315,-1.37177063494622,
7.37551168840027));
#27192=CARTESIAN_POINT('Ctrl Pts',(-1.51967208927657,-1.29612106912868,
7.3696634208893));
#27193=CARTESIAN_POINT('Ctrl Pts',(-1.61338804195452,-1.17419677909837,
7.36053179236581));
#27194=CARTESIAN_POINT('Ctrl Pts',(-1.64359545555285,-1.13152657637209,
7.35738607992213));
#27195=CARTESIAN_POINT('Ctrl Pts',(-1.68901933550856,-1.06169910861576,
7.35227501593395));
#27196=CARTESIAN_POINT('Ctrl Pts',(-1.7053369941738,-1.03528589456422,7.35034977868486));
#27197=CARTESIAN_POINT('Ctrl Pts',(-1.72545341794302,-1.00095683167633,
7.34785293604103));
#27198=CARTESIAN_POINT('Ctrl Pts',(-1.72982608226541,-0.99338099315371,
7.34730226121661));
#27199=CARTESIAN_POINT('Ctrl Pts',(-1.73679007586518,-0.981130145509479,
7.34641219867722));
#27200=CARTESIAN_POINT('Ctrl Pts',(-1.73941272233597,-0.976472995284484,
7.34607394170442));
#27201=CARTESIAN_POINT('Ctrl Pts',(-1.74437477011429,-0.967578241645158,
7.34542806312506));
#27202=CARTESIAN_POINT('Ctrl Pts',(-1.74671752959149,-0.963342547308899,
7.34512056481494));
#27203=CARTESIAN_POINT('Ctrl Pts',(-1.75203120730047,-0.953652341848402,
7.34441722356562));
#27204=CARTESIAN_POINT('Ctrl Pts',(-1.75499210152084,-0.948192418565323,
7.34402102664981));
#27205=CARTESIAN_POINT('Ctrl Pts',(-1.76399174693945,-0.931410401122638,
7.34280349353485));
#27206=CARTESIAN_POINT('Ctrl Pts',(-1.76994669419615,-0.920043969330585,
7.34197920047895));
#27207=CARTESIAN_POINT('Ctrl Pts',(-1.82317548411611,-0.816014654065569,
7.33443685126731));
#27208=CARTESIAN_POINT('Ctrl Pts',(-1.86323512525757,-0.71985924465018,
7.32746571093228));
#27209=CARTESIAN_POINT('Ctrl Pts',(-1.94773810326278,-0.461926290934635,
7.30881056135202));
#27210=CARTESIAN_POINT('Ctrl Pts',(-1.97962347072231,-0.296898718610514,
7.29687699468382));
#27211=CARTESIAN_POINT('Ctrl Pts',(-1.99236283329669,-0.101583539268264,
7.28376167222506));
#27212=CARTESIAN_POINT('Ctrl Pts',(-1.99360388469226,-0.0732982310438227,
7.28188860540407));
#27213=CARTESIAN_POINT('Ctrl Pts',(-1.99437183414486,-0.0392611292870622,
7.27967368621796));
#27214=CARTESIAN_POINT('Ctrl Pts',(-1.99447646566995,-0.033527286803309,
7.2793018961564));
#27215=CARTESIAN_POINT('Ctrl Pts',(-1.99460047899178,-0.0246275037247389,
7.27872697230926));
#27216=CARTESIAN_POINT('Ctrl Pts',(-1.99463705276389,-0.0214618922179287,
7.27852289669645));
#27217=CARTESIAN_POINT('Ctrl Pts',(-1.99469075502728,-0.0156072229377242,
7.2781462645416));
#27218=CARTESIAN_POINT('Ctrl Pts',(-1.99470998212934,-0.0129182411510024,
7.277973594608));
#27219=CARTESIAN_POINT('Ctrl Pts',(-1.99474089383202,-0.00689035509265752,
7.27758721691371));
#27220=CARTESIAN_POINT('Ctrl Pts',(-1.99474963291213,-0.00355146651014842,
7.27737367630814));
#27221=CARTESIAN_POINT('Ctrl Pts',(-1.99475068666648,0.00633823593360937,
7.27674254497808));
#27222=CARTESIAN_POINT('Ctrl Pts',(-1.99471911543883,0.0128890874863369,
7.27632627015099));
#27223=CARTESIAN_POINT('Ctrl Pts',(-1.99419126750845,0.0670499353735925,
7.27289846024733));
#27224=CARTESIAN_POINT('Ctrl Pts',(-1.99202276093881,0.114632811185366,
7.26997536760017));
#27225=CARTESIAN_POINT('Ctrl Pts',(-1.98147388664981,0.24401713358489,7.26215838591947));
#27226=CARTESIAN_POINT('Ctrl Pts',(-1.96973748999983,0.325452349299354,
7.25738005423522));
#27227=CARTESIAN_POINT('Ctrl Pts',(-1.92122301949776,0.558861592470391,
7.24354819242071));
#27228=CARTESIAN_POINT('Ctrl Pts',(-1.87159159017216,0.707503951896778,
7.23452215364744));
#27229=CARTESIAN_POINT('Ctrl Pts',(-1.79612706465119,0.86798809244787,7.22355013073217));
#27230=CARTESIAN_POINT('Ctrl Pts',(-1.78681411569341,0.887001140432456,
7.22223040976254));
#27231=CARTESIAN_POINT('Ctrl Pts',(-1.77363745262787,0.912852294724462,
7.22040713363302));
#27232=CARTESIAN_POINT('Ctrl Pts',(-1.77003314117497,0.919821614036633,
7.21991267046705));
#27233=CARTESIAN_POINT('Ctrl Pts',(-1.76423606591414,0.930870622779886,
7.21912402839341));
#27234=CARTESIAN_POINT('Ctrl Pts',(-1.76207002266776,0.934964302661715,
7.21883079525606));
#27235=CARTESIAN_POINT('Ctrl Pts',(-1.75760286108029,0.943336283696662,
7.21822895207724));
#27236=CARTESIAN_POINT('Ctrl Pts',(-1.75530033296402,0.947613793602898,
7.21792029344933));
#27237=CARTESIAN_POINT('Ctrl Pts',(-1.74995552530238,0.957456762304467,
7.21720734272551));
#27238=CARTESIAN_POINT('Ctrl Pts',(-1.7469022927326,0.963016183834959,7.21680266180658));
#27239=CARTESIAN_POINT('Ctrl Pts',(-1.73726225020492,0.980372371082721,
7.2155329401265));
#27240=CARTESIAN_POINT('Ctrl Pts',(-1.73058217739676,0.992116638460261,
7.21466456191485));
#27241=CARTESIAN_POINT('Ctrl Pts',(-1.66396023288622,1.10652461966725,7.20611292792303));
#27242=CARTESIAN_POINT('Ctrl Pts',(-1.59508437398908,1.20368477488011,7.19809532983916));
#27243=CARTESIAN_POINT('Ctrl Pts',(-1.43637289912589,1.38985052728461,7.18118149466509));
#27244=CARTESIAN_POINT('Ctrl Pts',(-1.34589232997853,1.47764178287968,7.17229882799095));
#27245=CARTESIAN_POINT('Ctrl Pts',(-1.20754913031707,1.58855506330613,7.16018793139051));
#27246=CARTESIAN_POINT('Ctrl Pts',(-1.16611324212138,1.61921680435236,7.15672526981292));
#27247=CARTESIAN_POINT('Ctrl Pts',(-1.11758002107271,1.65229971701209,7.15289299311178));
#27248=CARTESIAN_POINT('Ctrl Pts',(-1.11160548206492,1.65632506303091,7.15242496799704));
#27249=CARTESIAN_POINT('Ctrl Pts',(-1.10272055999878,1.66224155073488,7.15173462521528));
#27250=CARTESIAN_POINT('Ctrl Pts',(-1.0998269210096,1.66415754984446,7.15151067966071));
#27251=CARTESIAN_POINT('Ctrl Pts',(-1.09467350338531,1.66755053035037,7.15111343651087));
#27252=CARTESIAN_POINT('Ctrl Pts',(-1.0924157176492,1.66903048217886,7.15093994048077));
#27253=CARTESIAN_POINT('Ctrl Pts',(-1.08758235901016,1.6721846821442,7.15056969018291));
#27254=CARTESIAN_POINT('Ctrl Pts',(-1.08500592966238,1.67385756016979,7.15037302776044));
#27255=CARTESIAN_POINT('Ctrl Pts',(-1.07796762688584,1.67840445835585,7.1498376613282));
#27256=CARTESIAN_POINT('Ctrl Pts',(-1.07349809126748,1.68126665940922,7.14949973832222));
#27257=CARTESIAN_POINT('Ctrl Pts',(-1.05040169332083,1.69592747719877,7.14776376948652));
#27258=CARTESIAN_POINT('Ctrl Pts',(-1.0315906753481,1.70743506527776,7.14638414192533));
#27259=CARTESIAN_POINT('Ctrl Pts',(-0.976506181248834,1.73989006721012,
7.14243073808672));
#27260=CARTESIAN_POINT('Ctrl Pts',(-0.939757365411546,1.76001089346714,
7.13989985853828));
#27261=CARTESIAN_POINT('Ctrl Pts',(-0.785700343710376,1.83815821510842,
7.12961006741691));
#27262=CARTESIAN_POINT('Ctrl Pts',(-0.663454394023345,1.88573132329631,
7.12217070924366));
#27263=CARTESIAN_POINT('Ctrl Pts',(-0.435752793124694,1.94943407117073,
7.10831591615025));
#27264=CARTESIAN_POINT('Ctrl Pts',(-0.331998051581029,1.96975792856896,
7.10200553299235));
#27265=CARTESIAN_POINT('Ctrl Pts',(-0.214359720014107,1.98324046306529,
7.09461381602594));
#27266=CARTESIAN_POINT('Ctrl Pts',(-0.201574317927565,1.98458071287914,
7.09380754432778));
#27267=CARTESIAN_POINT('Ctrl Pts',(-0.182589241293978,1.9863855031038,7.09260565996354));
#27268=CARTESIAN_POINT('Ctrl Pts',(-0.176398736218186,1.98694481111507,
7.09221302739874));
#27269=CARTESIAN_POINT('Ctrl Pts',(-0.165382424496781,1.98788823918704,
7.09151297733458));
#27270=CARTESIAN_POINT('Ctrl Pts',(-0.1605576219764,1.98828374413182,7.09120592011053));
#27271=CARTESIAN_POINT('Ctrl Pts',(-0.150405362365629,1.9890787643456,7.09055883422007));
#27272=CARTESIAN_POINT('Ctrl Pts',(-0.145077651741275,1.98947444764908,
7.09021868770202));
#27273=CARTESIAN_POINT('Ctrl Pts',(-0.131033727629096,1.99046076219768,
7.08932052721176));
#27274=CARTESIAN_POINT('Ctrl Pts',(-0.122315187592673,1.99101553848319,
7.08876139281826));
#27275=CARTESIAN_POINT('Ctrl Pts',(-0.0827107702847989,1.99327452464209,
7.08621423956927));
#27276=CARTESIAN_POINT('Ctrl Pts',(-0.051792890060909,1.99431735687546,
7.08420563688783));
#27277=CARTESIAN_POINT('Ctrl Pts',(0.0311375349021303,1.99518483835903,
7.07876063889943));
#27278=CARTESIAN_POINT('Ctrl Pts',(0.0831369344897313,1.99369494899308,
7.07528550194827));
#27279=CARTESIAN_POINT('Ctrl Pts',(0.236146732048212,1.98331463699855,7.06488504609092));
#27280=CARTESIAN_POINT('Ctrl Pts',(0.336600332260701,1.96875573466987,7.05782308017482));
#27281=CARTESIAN_POINT('Ctrl Pts',(0.551908815801065,1.92058655224867,7.04243041712817));
#27282=CARTESIAN_POINT('Ctrl Pts',(0.66575901982097,1.88415182408532,7.03412492786596));
#27283=CARTESIAN_POINT('Ctrl Pts',(0.782012012049444,1.83508364595316,7.02588567682527));
#27284=CARTESIAN_POINT('Ctrl Pts',(0.788328602413289,1.83237899807135,7.02543882882449));
#27285=CARTESIAN_POINT('Ctrl Pts',(0.797807196215396,1.82826235255206,7.02476968361696));
#27286=CARTESIAN_POINT('Ctrl Pts',(0.80097962344079,1.82687470707954,7.0245459599067));
#27287=CARTESIAN_POINT('Ctrl Pts',(0.806465424282125,1.82445813655712,7.02415952189054));
#27288=CARTESIAN_POINT('Ctrl Pts',(0.8087804688011,1.82343306048631,7.02399657474294));
#27289=CARTESIAN_POINT('Ctrl Pts',(0.813625677936984,1.82127661279221,7.02365582594433));
#27290=CARTESIAN_POINT('Ctrl Pts',(0.816155441351031,1.82014437333398,7.02347808076424));
#27291=CARTESIAN_POINT('Ctrl Pts',(0.822265552123668,1.81739438761081,7.0230491562741));
#27292=CARTESIAN_POINT('Ctrl Pts',(0.825843520910581,1.81577131763351,7.02279830319067));
#27293=CARTESIAN_POINT('Ctrl Pts',(0.838302711073343,1.81007502420444,7.02192581134149));
#27294=CARTESIAN_POINT('Ctrl Pts',(0.847158961074161,1.80594704590415,7.02130745159122));
#27295=CARTESIAN_POINT('Ctrl Pts',(0.972007338894504,1.74663356459625,7.01261124055757));
#27296=CARTESIAN_POINT('Ctrl Pts',(1.08245438858042,1.68042562113706,7.00516380797185));
#27297=CARTESIAN_POINT('Ctrl Pts',(1.3085558397663,1.51328155150371,6.98885390347805));
#27298=CARTESIAN_POINT('Ctrl Pts',(1.42048995154919,1.40873720834088,6.98001442590273));
#27299=CARTESIAN_POINT('Ctrl Pts',(1.53269722152463,1.27682725685387,6.96930091877563));
#27300=CARTESIAN_POINT('Ctrl Pts',(1.54575010852392,1.26099372312026,6.96802219236812));
#27301=CARTESIAN_POINT('Ctrl Pts',(1.56368323574309,1.23854341395479,6.9662176781642));
#27302=CARTESIAN_POINT('Ctrl Pts',(1.56877066100798,1.23209320260194,6.96570019559267));
#27303=CARTESIAN_POINT('Ctrl Pts',(1.57670836275463,1.22190033573453,6.96488388698674));
#27304=CARTESIAN_POINT('Ctrl Pts',(1.57958553017727,1.21817865844236,6.96458613003455));
#27305=CARTESIAN_POINT('Ctrl Pts',(1.58509773155024,1.21099614557565,6.96401203939623));
#27306=CARTESIAN_POINT('Ctrl Pts',(1.58773466549602,1.20753679639785,6.96373578288426));
#27307=CARTESIAN_POINT('Ctrl Pts',(1.59392805115474,1.19935643847254,6.963083077779));
#27308=CARTESIAN_POINT('Ctrl Pts',(1.59747486087811,1.19462821261838,6.96270625426327));
#27309=CARTESIAN_POINT('Ctrl Pts',(1.60777069899071,1.18077506552362,6.96160343448227));
#27310=CARTESIAN_POINT('Ctrl Pts',(1.61446283901,1.17160834262333,6.96087523625416));
#27311=CARTESIAN_POINT('Ctrl Pts',(1.66581681700103,1.09998946973615,6.95519705379899));
#27312=CARTESIAN_POINT('Ctrl Pts',(1.70691196067171,1.03507073769376,6.95011169183221));
#27313=CARTESIAN_POINT('Ctrl Pts',(1.79296326601329,0.880014278648866,6.93809529956556));
#27314=CARTESIAN_POINT('Ctrl Pts',(1.83504170557687,0.788518249625135,6.93109369109041));
#27315=CARTESIAN_POINT('Ctrl Pts',(1.8820732772755,0.661833312060828,6.9216653500211));
#27316=CARTESIAN_POINT('Ctrl Pts',(1.89326276460418,0.629109938013492,6.91925381924777));
#27317=CARTESIAN_POINT('Ctrl Pts',(1.92949110039182,0.513420053017111,6.91083889901536));
#27318=CARTESIAN_POINT('Ctrl Pts',(1.9499738739975,0.429117469235799,6.90490062476081));
#27319=CARTESIAN_POINT('Ctrl Pts',(1.96625931665297,0.336025593520275,6.89872759464816));
#27320=CARTESIAN_POINT('Ctrl Pts',(1.96756349581628,0.328302900811625,6.89821836449237));
#27321=CARTESIAN_POINT('Ctrl Pts',(1.96939308725892,0.317066318167938,6.89748179541153));
#27322=CARTESIAN_POINT('Ctrl Pts',(1.96995462975499,0.313558510403451,6.89725247236131));
#27323=CARTESIAN_POINT('Ctrl Pts',(1.97092921167129,0.30736458901631,6.89684865593484));
#27324=CARTESIAN_POINT('Ctrl Pts',(1.97134613622403,0.304679109155858,6.89667394341581));
#27325=CARTESIAN_POINT('Ctrl Pts',(1.97221070370737,0.299034213570926,6.89630747940421));
#27326=CARTESIAN_POINT('Ctrl Pts',(1.97265717360171,0.296074646721272,6.89611579512523));
#27327=CARTESIAN_POINT('Ctrl Pts',(1.97382488240029,0.288214216243301,6.89560785931549));
#27328=CARTESIAN_POINT('Ctrl Pts',(1.97453453561625,0.283311612459413,6.89529225886045));
#27329=CARTESIAN_POINT('Ctrl Pts',(1.97773611920141,0.260597149070922,6.89383539031632));
#27330=CARTESIAN_POINT('Ctrl Pts',(1.98000544312203,0.242754055066817,6.89270619366479));
#27331=CARTESIAN_POINT('Ctrl Pts',(1.98556877822048,0.193720709666876,6.88963882631248));
#27332=CARTESIAN_POINT('Ctrl Pts',(1.98836918642222,0.162478587686997,6.88772389278685));
#27333=CARTESIAN_POINT('Ctrl Pts',(1.99563531842221,0.0522288974078525,
6.88106462330119));
#27334=CARTESIAN_POINT('Ctrl Pts',(1.99613691718685,-0.0269693157510462,
6.87645628370727));
#27335=CARTESIAN_POINT('Ctrl Pts',(1.9834004018424,-0.266328035117351,6.86254317604347));
#27336=CARTESIAN_POINT('Ctrl Pts',(1.95554448664742,-0.425025067664789,
6.85328606102782));
#27337=CARTESIAN_POINT('Ctrl Pts',(1.90489378778237,-0.592119051995601,
6.84248185364553));
#27338=CARTESIAN_POINT('Ctrl Pts',(1.90067227458819,-0.605532991200891,
6.84160730521256));
#27339=CARTESIAN_POINT('Ctrl Pts',(1.89306982741216,-0.628826852087737,
6.84007542127812));
#27340=CARTESIAN_POINT('Ctrl Pts',(1.88975245308941,-0.638727047173065,
6.83942016256767));
#27341=CARTESIAN_POINT('Ctrl Pts',(1.88431154579514,-0.654551110063635,
6.83836590224008));
#27342=CARTESIAN_POINT('Ctrl Pts',(1.88223740923146,-0.66049185545241,6.83796853414694));
#27343=CARTESIAN_POINT('Ctrl Pts',(1.87850946895029,-0.671009253072189,
6.83726220510875));
#27344=CARTESIAN_POINT('Ctrl Pts',(1.87686695384153,-0.675589875245848,
6.83695362122606));
#27345=CARTESIAN_POINT('Ctrl Pts',(1.87341622441068,-0.685103508038202,
6.83631069877948));
#27346=CARTESIAN_POINT('Ctrl Pts',(1.87160525065326,-0.690035471166528,
6.83597627017356));
#27347=CARTESIAN_POINT('Ctrl Pts',(1.86686985145359,-0.702775956782002,
6.83510939743517));
#27348=CARTESIAN_POINT('Ctrl Pts',(1.86391593557773,-0.710573338436012,
6.83457597042715));
#27349=CARTESIAN_POINT('Ctrl Pts',(1.85113523944515,-0.743682136118935,
6.83229847058753));
#27350=CARTESIAN_POINT('Ctrl Pts',(1.84084148645247,-0.76880901074337,6.83053878005297));
#27351=CARTESIAN_POINT('Ctrl Pts',(1.81271389500614,-0.833661568358566,
6.82591252252434));
#27352=CARTESIAN_POINT('Ctrl Pts',(1.79408729919948,-0.873025523795212,
6.82302005798224));
#27353=CARTESIAN_POINT('Ctrl Pts',(1.6945271571241,-1.06676199560036,6.808355877972));
#27354=CARTESIAN_POINT('Ctrl Pts',(1.5948941023617,-1.21066165863627,6.79597968835468));
#27355=CARTESIAN_POINT('Ctrl Pts',(1.43768831303722,-1.38407297265698,6.77991314323283));
#27356=CARTESIAN_POINT('Ctrl Pts',(1.39553477671232,-1.4265657836734,6.77587334301589));
#27357=CARTESIAN_POINT('Ctrl Pts',(1.34659752025626,-1.47164794256912,6.77153015647505));
#27358=CARTESIAN_POINT('Ctrl Pts',(1.34164155168241,-1.476167503477,6.77109407605614));
#27359=CARTESIAN_POINT('Ctrl Pts',(1.33412347058594,-1.48295442642768,6.77043833648228));
#27360=CARTESIAN_POINT('Ctrl Pts',(1.33157822835514,-1.48524027949247,6.77021732800031));
#27361=CARTESIAN_POINT('Ctrl Pts',(1.32714697978876,-1.48919938660804,6.76983429231993));
#27362=CARTESIAN_POINT('Ctrl Pts',(1.32526366855471,-1.4908756245977,6.76967204186657));
#27363=CARTESIAN_POINT('Ctrl Pts',(1.3212957029328,-1.49439384583382,6.76933134337173));
#27364=CARTESIAN_POINT('Ctrl Pts',(1.31921036722535,-1.49623504443829,6.7691529561751));
#27365=CARTESIAN_POINT('Ctrl Pts',(1.31413105912476,-1.50070082764237,6.768720046878));
#27366=CARTESIAN_POINT('Ctrl Pts',(1.31113304648571,-1.50332084058045,6.76846586606313));
#27367=CARTESIAN_POINT('Ctrl Pts',(1.30050239528803,-1.51255515181899,6.76756920815715));
#27368=CARTESIAN_POINT('Ctrl Pts',(1.29282722909961,-1.51912057894822,6.76693025792698));
#27369=CARTESIAN_POINT('Ctrl Pts',(1.24141590694143,-1.56242656697028,6.76270342425805));
#27370=CARTESIAN_POINT('Ctrl Pts',(1.1961644194305,-1.59733598396568,6.75923636779827));
#27371=CARTESIAN_POINT('Ctrl Pts',(1.02556110511555,-1.71762602727148,6.74680698745791));
#27372=CARTESIAN_POINT('Ctrl Pts',(0.892090093568565,-1.79058504929666,
6.73824555030284));
#27373=CARTESIAN_POINT('Ctrl Pts',(0.716234240689046,-1.86212156018101,
6.72701797584538));
#27374=CARTESIAN_POINT('Ctrl Pts',(0.680427989701769,-1.87550145784045,
6.72473694622258));
#27375=CARTESIAN_POINT('Ctrl Pts',(0.597422668638744,-1.9038285194621,6.71943515037275));
#27376=CARTESIAN_POINT('Ctrl Pts',(0.550009275411201,-1.91806309591593,
6.71639633892168));
#27377=CARTESIAN_POINT('Ctrl Pts',(0.492769956287579,-1.93295075998348,
6.71269482342136));
#27378=CARTESIAN_POINT('Ctrl Pts',(0.483403991971901,-1.93531430151124,
6.71208813518755));
#27379=CARTESIAN_POINT('Ctrl Pts',(0.468072283069895,-1.93906508658658,
6.71109319999435));
#27380=CARTESIAN_POINT('Ctrl Pts',(0.462116589323327,-1.94049306329855,
6.71070626699457));
#27381=CARTESIAN_POINT('Ctrl Pts',(0.451452101024465,-1.94299817173325,
6.71001257754239));
#27382=CARTESIAN_POINT('Ctrl Pts',(0.446745772305301,-1.94408567432939,
6.70970615728118));
#27383=CARTESIAN_POINT('Ctrl Pts',(0.436881860171351,-1.94632724257127,
6.70906331076621));
#27384=CARTESIAN_POINT('Ctrl Pts',(0.431723553822848,-1.94747792467844,
6.70872677852071));
#27385=CARTESIAN_POINT('Ctrl Pts',(0.41820087199882,-1.95043811236286,6.7078435812871));
#27386=CARTESIAN_POINT('Ctrl Pts',(0.409829387923799,-1.95221429881714,
6.70729585389748));
#27387=CARTESIAN_POINT('Ctrl Pts',(0.391412916538124,-1.95599806256989,
6.70608868774871));
#27388=CARTESIAN_POINT('Ctrl Pts',(0.381363421326324,-1.95798223341495,
6.70542851679255));
#27389=CARTESIAN_POINT('Ctrl Pts',(0.351647204436483,-1.96361194484257,
6.70347195743381));
#27390=CARTESIAN_POINT('Ctrl Pts',(0.331940898929404,-1.96703909918402,
6.7021687228488));
#27391=CARTESIAN_POINT('Ctrl Pts',(0.262270416187405,-1.97807886991449,
6.69753996073748));
#27392=CARTESIAN_POINT('Ctrl Pts',(0.21207519526325,-1.98408799545187,6.6941660901811));
#27393=CARTESIAN_POINT('Ctrl Pts',(0.043655013580932,-1.99778648180186,
6.68272047543573));
#27394=CARTESIAN_POINT('Ctrl Pts',(-0.0750107800357254,-1.99685377356109,
6.67443411863093));
#27395=CARTESIAN_POINT('Ctrl Pts',(-0.244166897664909,-1.98042050028122,
6.6625927489732));
#27396=CARTESIAN_POINT('Ctrl Pts',(-0.295244664471885,-1.97345227131158,
6.65901652919969));
#27397=CARTESIAN_POINT('Ctrl Pts',(-0.398610369668733,-1.95524713322919,
6.65183913742975));
#27398=CARTESIAN_POINT('Ctrl Pts',(-0.45083571632199,-1.94386982695586,
6.64824464390534));
#27399=CARTESIAN_POINT('Ctrl Pts',(-0.5095780399058,-1.92857734695514,6.64428377433788));
#27400=CARTESIAN_POINT('Ctrl Pts',(-0.51660005926903,-1.92670826661875,
6.6438116534999));
#27401=CARTESIAN_POINT('Ctrl Pts',(-0.526972403450067,-1.92388663326078,
6.64311644885455));
#27402=CARTESIAN_POINT('Ctrl Pts',(-0.530330599819436,-1.92296363641789,
6.64289170424983));
#27403=CARTESIAN_POINT('Ctrl Pts',(-0.536288848869815,-1.92130922238776,
6.64249357496844));
#27404=CARTESIAN_POINT('Ctrl Pts',(-0.53888984503603,-1.92058131634648,
6.64231998851144));
#27405=CARTESIAN_POINT('Ctrl Pts',(-0.544438688353919,-1.91901627595181,
6.64195012442986));
#27406=CARTESIAN_POINT('Ctrl Pts',(-0.547386077679175,-1.91817763385395,
6.64175393637243));
#27407=CARTESIAN_POINT('Ctrl Pts',(-0.555400255705559,-1.91587732564434,
6.64122120063175));
#27408=CARTESIAN_POINT('Ctrl Pts',(-0.560463244677572,-1.91440234116177,
6.64088542103152));
#27409=CARTESIAN_POINT('Ctrl Pts',(-0.586253432000998,-1.90677788540156,
6.6391786965708));
#27410=CARTESIAN_POINT('Ctrl Pts',(-0.606886485296367,-1.90031152123041,
6.6378254374689));
#27411=CARTESIAN_POINT('Ctrl Pts',(-0.66605306859671,-1.88070678072047,
6.6339691973003));
#27412=CARTESIAN_POINT('Ctrl Pts',(-0.704296488517449,-1.86672215136927,
6.63150663233279));
#27413=CARTESIAN_POINT('Ctrl Pts',(-0.884650774639296,-1.79443850019209,
6.61991914258434));
#27414=CARTESIAN_POINT('Ctrl Pts',(-1.02014269740057,-1.72102607436799,
6.61125317488648));
#27415=CARTESIAN_POINT('Ctrl Pts',(-1.17712688688369,-1.61085617140632,
6.59991259588884));
#27416=CARTESIAN_POINT('Ctrl Pts',(-1.20774180750381,-1.5880317425933,6.59763418900329));
#27417=CARTESIAN_POINT('Ctrl Pts',(-1.2767079609247,-1.53346690944367,6.59231920331009));
#27418=CARTESIAN_POINT('Ctrl Pts',(-1.31456215159463,-1.50114279331927,
6.5892640316761));
#27419=CARTESIAN_POINT('Ctrl Pts',(-1.35828461002956,-1.46088470342688,
6.58554445506575));
#27420=CARTESIAN_POINT('Ctrl Pts',(-1.36535529606649,-1.45427855267605,
6.58493671135866));
#27421=CARTESIAN_POINT('Ctrl Pts',(-1.37682599295557,-1.44340407420989,
6.58394038747499));
#27422=CARTESIAN_POINT('Ctrl Pts',(-1.38125494432265,-1.43916639543346,
6.5835531274377));
#27423=CARTESIAN_POINT('Ctrl Pts',(-1.38913938507402,-1.43155253823965,
6.58285907218617));
#27424=CARTESIAN_POINT('Ctrl Pts',(-1.39260228899916,-1.42818407948891,
6.58255261452684));
#27425=CARTESIAN_POINT('Ctrl Pts',(-1.39927757448958,-1.42164349036459,
6.58195869915859));
#27426=CARTESIAN_POINT('Ctrl Pts',(-1.40249149361131,-1.41847296553758,
6.58167131299408));
#27427=CARTESIAN_POINT('Ctrl Pts',(-1.40944639958939,-1.41156522021896,
6.58104626532935));
#27428=CARTESIAN_POINT('Ctrl Pts',(-1.41318333649937,-1.40782398786074,
6.58070842716295));
#27429=CARTESIAN_POINT('Ctrl Pts',(-1.4279587445258,-1.39291348870169,6.57936466420977));
#27430=CARTESIAN_POINT('Ctrl Pts',(-1.43887978834616,-1.3816291449958,6.57835360997683));
#27431=CARTESIAN_POINT('Ctrl Pts',(-1.49773550372064,-1.31936081581584,
6.57280511859302));
#27432=CARTESIAN_POINT('Ctrl Pts',(-1.54308986380432,-1.26601591592972,
6.56815940871857));
#27433=CARTESIAN_POINT('Ctrl Pts',(-1.62125493049575,-1.1636251635499,6.55943007336932));
#27434=CARTESIAN_POINT('Ctrl Pts',(-1.65487584720457,-1.11529197560446,
6.55537920419555));
#27435=CARTESIAN_POINT('Ctrl Pts',(-1.76854600651221,-0.935400164552377,
6.5406084665738));
#27436=CARTESIAN_POINT('Ctrl Pts',(-1.8354437169428,-0.796166047033757,
6.52969834963504));
#27437=CARTESIAN_POINT('Ctrl Pts',(-1.89030717688213,-0.637157031983151,
6.51860050737854));
#27438=CARTESIAN_POINT('Ctrl Pts',(-1.89480728673851,-0.623647080281074,
6.51766817237438));
#27439=CARTESIAN_POINT('Ctrl Pts',(-1.90060705794863,-0.605592834965986,
6.51643733635948));
#27440=CARTESIAN_POINT('Ctrl Pts',(-1.90203565951752,-0.601090859622062,
6.51613166090642));
#27441=CARTESIAN_POINT('Ctrl Pts',(-1.90424035390347,-0.594056606013305,
6.5156560340981));
#27442=CARTESIAN_POINT('Ctrl Pts',(-1.9050274046608,-0.591527822063384,
6.51548544782484));
#27443=CARTESIAN_POINT('Ctrl Pts',(-1.90652867546336,-0.586670184747108,
6.51515853882475));
#27444=CARTESIAN_POINT('Ctrl Pts',(-1.90724365771197,-0.584341617744951,
6.51500217448601));
#27445=CARTESIAN_POINT('Ctrl Pts',(-1.90894323872839,-0.578770040735878,
6.51462885408686));
#27446=CARTESIAN_POINT('Ctrl Pts',(-1.90992383860049,-0.575525829048528,
6.51441213436175));
#27447=CARTESIAN_POINT('Ctrl Pts',(-1.91284612196619,-0.56576803768594,
6.51376222326111));
#27448=CARTESIAN_POINT('Ctrl Pts',(-1.91476281268981,-0.559246933956545,
6.51333046828122));
#27449=CARTESIAN_POINT('Ctrl Pts',(-1.91907869260439,-0.544280813955333,
6.51234520752543));
#27450=CARTESIAN_POINT('Ctrl Pts',(-1.92145555607818,-0.535829436775219,
6.51179292195998));
#27451=CARTESIAN_POINT('Ctrl Pts',(-1.97072567241273,-0.356095946879005,
6.50012887838157));
#27452=CARTESIAN_POINT('Ctrl Pts',(-1.99459991883049,-0.179306569445352,
6.490166969518));
#27453=CARTESIAN_POINT('Ctrl Pts',(-1.99474929467261,-0.00167746926262795,
6.47978083014939));
#27454=CARTESIAN_POINT('Origin',(-6.93889390390723E-17,-2.77555756156289E-16,
5.));
#27455=CARTESIAN_POINT('',(4.,2.12302963502652E-16,5.));
#27456=CARTESIAN_POINT('Origin',(-6.93889390390723E-17,-2.77555756156289E-16,
5.));
#27457=CARTESIAN_POINT('',(4.,2.12302963502652E-16,5.5));
#27458=CARTESIAN_POINT('',(4.,2.12302963502652E-16,5.));
#27459=CARTESIAN_POINT('Origin',(-6.93889390390723E-17,-2.77555756156289E-16,
5.5));
#27460=CARTESIAN_POINT('Origin',(0.,0.,5.));
#27461=CARTESIAN_POINT('',(4.5,5.51091059616309E-16,5.5));
#27462=CARTESIAN_POINT('Origin',(0.,0.,5.5));
#27463=CARTESIAN_POINT('',(4.5,5.51091059616309E-16,5.));
#27464=CARTESIAN_POINT('',(4.5,5.51091059616309E-16,5.));
#27465=CARTESIAN_POINT('',(-4.5,5.51091059616309E-16,5.));
#27466=CARTESIAN_POINT('Origin',(0.,0.,5.));
#27467=CARTESIAN_POINT('Origin',(0.,0.,5.));
#27468=CARTESIAN_POINT('Origin',(0.,0.,5.5));
#27469=CARTESIAN_POINT('Ctrl Pts',(-0.873247375836237,1.78947949709258,
4.73478819788609));
#27470=CARTESIAN_POINT('Ctrl Pts',(-1.4690688679767,1.49873543257783,4.77718129246584));
#27471=CARTESIAN_POINT('Ctrl Pts',(-2.33695383301822,0.280390198345026,
4.86195971951784));
#27472=CARTESIAN_POINT('Ctrl Pts',(-1.4992907210582,-1.81727971168775,4.98912347904207));
#27473=CARTESIAN_POINT('Ctrl Pts',(0.715424845994203,-2.24230451559634,
5.11627947645882));
#27474=CARTESIAN_POINT('Ctrl Pts',(2.27294797015263,-0.613618701373298,
5.24343547387554));
#27475=CARTESIAN_POINT('Ctrl Pts',(1.74631047731586,1.57935716468537,5.37059147129228));
#27476=CARTESIAN_POINT('Ctrl Pts',(-0.382281089693881,2.32300256223768,
5.49774746870903));
#27477=CARTESIAN_POINT('Ctrl Pts',(-2.16010694979347,0.936454718196414,
5.62490346612576));
#27478=CARTESIAN_POINT('Ctrl Pts',(-1.95681075276908,-1.30920204522563,
5.75205946354249));
#27479=CARTESIAN_POINT('Ctrl Pts',(0.0412662141189832,-2.35397703574761,
5.87921546095925));
#27480=CARTESIAN_POINT('Ctrl Pts',(2.00147364547165,-1.23979915738411,6.00637145837596));
#27481=CARTESIAN_POINT('Ctrl Pts',(2.12598795827045,1.01152412810136,6.13352745579272));
#27482=CARTESIAN_POINT('Ctrl Pts',(0.300590670980986,2.33508519333647,6.26068345320944));
#27483=CARTESIAN_POINT('Ctrl Pts',(-1.80049820770884,1.51696997007267,6.38783945062618));
#27484=CARTESIAN_POINT('Ctrl Pts',(-2.25021438906683,-0.692478639950551,
6.51499544804292));
#27485=CARTESIAN_POINT('Ctrl Pts',(-0.636086407863099,-2.2667999029652,
6.64215144545965));
#27486=CARTESIAN_POINT('Ctrl Pts',(1.56144451584301,-1.76206723210801,6.76930744287639));
#27487=CARTESIAN_POINT('Ctrl Pts',(2.32685575557651,0.358792400677143,6.89646344029311));
#27488=CARTESIAN_POINT('Ctrl Pts',(0.958129905223776,2.15057580603736,7.02361943770987));
#27489=CARTESIAN_POINT('Ctrl Pts',(-1.28936992982972,1.9699022129551,7.15077543512658));
#27490=CARTESIAN_POINT('Ctrl Pts',(-2.35429024746335,-0.0175191102142973,
7.27793143254334));
#27491=CARTESIAN_POINT('Ctrl Pts',(-1.25991131263991,-1.98887227175793,
7.40508742996006));
#27492=CARTESIAN_POINT('Ctrl Pts',(0.990028418015555,-2.13607893341421,
7.5322434273768));
#27493=CARTESIAN_POINT('Ctrl Pts',(2.33193754512252,-0.324124593834741,
7.65939942479353));
#27494=CARTESIAN_POINT('Ctrl Pts',(1.53504880370339,1.78510913671325,7.78655542221029));
#27495=CARTESIAN_POINT('Ctrl Pts',(-0.669750329382192,2.25708306518675,
7.91371141962701));
#27496=CARTESIAN_POINT('Ctrl Pts',(-2.26027032938391,0.658913881193235,
8.04086741704374));
#27497=CARTESIAN_POINT('Ctrl Pts',(-1.77772393528634,-1.5435955020292,8.16802341446047));
#27498=CARTESIAN_POINT('Ctrl Pts',(0.335308732617007,-2.33035566358833,
8.29517941187722));
#27499=CARTESIAN_POINT('Ctrl Pts',(2.14080417550271,-0.9797688231252,8.42233540929394));
#27500=CARTESIAN_POINT('Ctrl Pts',(1.98280475043952,1.26943876818998,8.5494914067107));
#27501=CARTESIAN_POINT('Ctrl Pts',(0.00622378670963759,2.35434719809311,
8.67664740412742));
#27502=CARTESIAN_POINT('Ctrl Pts',(-1.97606548674515,1.27990415919458,8.80380340154417));
#27503=CARTESIAN_POINT('Ctrl Pts',(-2.1459543144859,-0.968436649845614,
8.93095939896089));
#27504=CARTESIAN_POINT('Ctrl Pts',(-0.347624688880569,-2.32855030873816,
9.05811539637764));
#27505=CARTESIAN_POINT('Ctrl Pts',(1.76953806512862,-1.55297279457662,9.18527139379437));
#27506=CARTESIAN_POINT('Ctrl Pts',(2.26372243130189,0.646954572327261,9.3124273912111));
#27507=CARTESIAN_POINT('Ctrl Pts',(0.681674217651123,2.25351053372882,9.43958338862785));
#27508=CARTESIAN_POINT('Ctrl Pts',(-1.52558943758558,1.7932000258094,9.56673938604457));
#27509=CARTESIAN_POINT('Ctrl Pts',(-2.33361860631759,-0.311791059660172,
9.69389538346132));
#27510=CARTESIAN_POINT('Ctrl Pts',(-1.00130807954425,-2.1308147724463,9.82105138087805));
#27511=CARTESIAN_POINT('Ctrl Pts',(1.24937849388772,-1.99550566114121,9.94820737829478));
#27512=CARTESIAN_POINT('Ctrl Pts',(2.35416471413455,-0.0299660367678983,
10.0753633757115));
#27513=CARTESIAN_POINT('Ctrl Pts',(1.29976683558327,1.96305772654644,10.2025193731283));
#27514=CARTESIAN_POINT('Ctrl Pts',(-0.946746389309996,2.15561145361688,
10.329675370545));
#27515=CARTESIAN_POINT('Ctrl Pts',(-2.32492625710246,0.371089428132024,
10.4568313679617));
#27516=CARTESIAN_POINT('Ctrl Pts',(-1.57073884614258,-1.75378702864814,
10.5839873653785));
#27517=CARTESIAN_POINT('Ctrl Pts',(0.624093019129565,-2.27013157506554,
10.7111433627952));
#27518=CARTESIAN_POINT('Ctrl Pts',(2.24652155383406,-0.704365226849547,
10.838299360212));
#27519=CARTESIAN_POINT('Ctrl Pts',(1.80849374598863,1.5074282189729,10.9654553576287));
#27520=CARTESIAN_POINT('Ctrl Pts',(-0.288241677203082,2.33664421771029,
11.0926113550454));
#27521=CARTESIAN_POINT('Ctrl Pts',(-2.12060866334743,1.02274550185841,11.2197673524622));
#27522=CARTESIAN_POINT('Ctrl Pts',(-2.00800362685378,-1.22919115648376,
11.3469233498789));
#27523=CARTESIAN_POINT('Ctrl Pts',(-0.0537052392534047,-2.35374280921101,
11.4740793472957));
#27524=CARTESIAN_POINT('Ctrl Pts',(1.94985032135694,-1.31949732433985,11.6012353447123));
#27525=CARTESIAN_POINT('Ctrl Pts',(2.1650493648414,0.924959843688164,11.7283913421291));
#27526=CARTESIAN_POINT('Ctrl Pts',(0.394516427207001,2.32106575807313,11.8555473395458));
#27527=CARTESIAN_POINT('Ctrl Pts',(-1.73785763022056,1.58834515194902,11.9827033369626));
#27528=CARTESIAN_POINT('Ctrl Pts',(-2.27630984410938,-0.601167995028458,
12.1098593343793));
#27529=CARTESIAN_POINT('Ctrl Pts',(-0.726984601378939,-2.23930410038336,
12.237015331796));
#27530=CARTESIAN_POINT('Ctrl Pts',(1.48911369335759,-1.82360354049086,12.3641713292128));
#27531=CARTESIAN_POINT('Ctrl Pts',(2.33943218997905,0.26466298027044,12.4913273266295));
#27532=CARTESIAN_POINT('Ctrl Pts',(1.04407890990149,2.1101868861631,12.6184833240463));
#27533=CARTESIAN_POINT('Ctrl Pts',(-1.20887880907301,2.02029737652902,12.745639321463));
#27534=CARTESIAN_POINT('Ctrl Pts',(-2.35308152621917,0.0774389798607678,
12.8727953188797));
#27535=CARTESIAN_POINT('Ctrl Pts',(-1.33909361885933,-1.93644461438122,
12.9999513162965));
#27536=CARTESIAN_POINT('Ctrl Pts',(0.903079228697448,-2.17426708831529,
13.1271073137132));
#27537=CARTESIAN_POINT('Ctrl Pts',(2.31696920426529,-0.417903303554905,
13.2542633111299));
#27538=CARTESIAN_POINT('Ctrl Pts',(1.60578992141732,1.72175148988184,13.3814193085467));
#27539=CARTESIAN_POINT('Ctrl Pts',(-0.578181831523024,2.28225661009723,
13.5085753059634));
#27540=CARTESIAN_POINT('Ctrl Pts',(-2.23185890739893,0.749530040825484,
13.6357313033802));
#27541=CARTESIAN_POINT('Ctrl Pts',(-1.83852787263449,-1.47064772334569,
13.7628873007969));
#27542=CARTESIAN_POINT('Ctrl Pts',(0.241057366840046,-2.34198223958423,
13.8900432982136));
#27543=CARTESIAN_POINT('Ctrl Pts',(2.09955050079873,-1.06530613404394,14.0171992956304));
#27544=CARTESIAN_POINT('Ctrl Pts',(2.03238565987995,1.18844351744209,14.1443552930471));
#27545=CARTESIAN_POINT('Ctrl Pts',(0.101164844844109,2.35218093241218,14.2715112904638));
#27546=CARTESIAN_POINT('Ctrl Pts',(-1.92284196899347,1.35855372617836,14.3986672878806));
#27547=CARTESIAN_POINT('Ctrl Pts',(-2.18326368658655,-0.881106769618909,
14.5258232852973));
#27548=CARTESIAN_POINT('Ctrl Pts',(-0.441247678706356,-2.31263701230264,
14.652979282714));
#27549=CARTESIAN_POINT('Ctrl Pts',(1.70547024564302,-1.62307138039649,14.7801352801308));
#27550=CARTESIAN_POINT('Ctrl Pts',(2.28797126823687,0.555136866329734,14.9072912775475));
#27551=CARTESIAN_POINT('Ctrl Pts',(0.77199925229478,2.22418673206457,15.0344472749642));
#27552=CARTESIAN_POINT('Ctrl Pts',(-1.45203218694544,1.85326522459962,15.161603272381));
#27553=CARTESIAN_POINT('Ctrl Pts',(-2.34429410718315,-0.217427237627146,
15.2887592697977));
#27554=CARTESIAN_POINT('Ctrl Pts',(-1.08642501545519,-2.08870058898564,
15.4159152672144));
#27555=CARTESIAN_POINT('Ctrl Pts',(1.16788735988121,-2.04426724751572,15.5430712646312));
#27556=CARTESIAN_POINT('Ctrl Pts',(2.35104111938139,-0.124880421258552,
15.6702272620479));
#27557=CARTESIAN_POINT('Ctrl Pts',(1.37787566718401,1.90904376859675,15.7973832594646));
#27558=CARTESIAN_POINT('Ctrl Pts',(-0.85904470107426,2.19203824469192,15.9245392568814));
#27559=CARTESIAN_POINT('Ctrl Pts',(-2.30806962277358,0.464547178514352,
16.0516952542981));
#27560=CARTESIAN_POINT('Ctrl Pts',(-1.64018777134433,-1.68901555332339,
16.1788512517149));
#27561=CARTESIAN_POINT('Ctrl Pts',(0.532035443145291,-2.29345323734167,
16.3060072491316));
#27562=CARTESIAN_POINT('Ctrl Pts',(2.21628835464842,-0.794389950644875,
16.4331632465483));
#27563=CARTESIAN_POINT('Ctrl Pts',(1.86781409758233,1.43326897737603,16.5603192439651));
#27564=CARTESIAN_POINT('Ctrl Pts',(-0.193774995840213,2.3463675576565,16.6874752413818));
#27565=CARTESIAN_POINT('Ctrl Pts',(-2.07763825417111,1.10743340632322,16.8146312387985));
#27566=CARTESIAN_POINT('Ctrl Pts',(-2.0559409310666,-1.1472124269728,16.9417872362153));
#27567=CARTESIAN_POINT('Ctrl Pts',(-0.148583297205478,-2.34966220304693,
17.068943233632));
#27568=CARTESIAN_POINT('Ctrl Pts',(1.89505141648223,-1.39705747681493,17.1960992310488));
#27569=CARTESIAN_POINT('Ctrl Pts',(2.20058987024978,0.836895266798587,17.3232552284655));
#27570=CARTESIAN_POINT('Ctrl Pts',(0.487799433395791,2.30326750018633,17.4504112258822));
#27571=CARTESIAN_POINT('Ctrl Pts',(-1.67238908638211,1.65713735350629,17.577567223299));
#27572=CARTESIAN_POINT('Ctrl Pts',(-2.29870195988975,-0.508879911408193,
17.7047232207157));
#27573=CARTESIAN_POINT('Ctrl Pts',(-0.816699858718716,-2.20816457842359,
17.8318792181324));
#27574=CARTESIAN_POINT('Ctrl Pts',(1.41436000287518,-1.88217301194729,17.9590352155492));
#27575=CARTESIAN_POINT('Ctrl Pts',(2.34820238013224,0.170103046936591,18.0861912129659));
#27576=CARTESIAN_POINT('Ctrl Pts',(1.12832917007305,2.06636462140593,18.2133472103826));
#27577=CARTESIAN_POINT('Ctrl Pts',(-1.12642082137883,2.06740552330695,18.3405032077994));
#27578=CARTESIAN_POINT('Ctrl Pts',(-2.34804432364603,0.17227106207802,18.4676592052161));
#27579=CARTESIAN_POINT('Ctrl Pts',(-1.41609720426133,-1.88086633568658,
18.5948152026329));
#27580=CARTESIAN_POINT('Ctrl Pts',(0.814660719412214,-2.20891769355098,
18.7219712000496));
#27581=CARTESIAN_POINT('Ctrl Pts',(2.2982311329217,-0.511002078572337,18.8491271974663));
#27582=CARTESIAN_POINT('Ctrl Pts',(1.67391840309234,1.65559253574803,18.976283194883));
#27583=CARTESIAN_POINT('Ctrl Pts',(-0.485672626059938,2.3037169020806,19.1034391922998));
#27584=CARTESIAN_POINT('Ctrl Pts',(-2.1998162295865,0.838926707575607,19.2305951897165));
#27585=CARTESIAN_POINT('Ctrl Pts',(-1.8963405073781,-1.39530718650511,19.3577511871333));
#27586=CARTESIAN_POINT('Ctrl Pts',(0.146413798377855,-2.34979838800702,
19.48490718455));
#27587=CARTESIAN_POINT('Ctrl Pts',(2.05488083723017,-1.14911018158402,19.6120631819667));
#27588=CARTESIAN_POINT('Ctrl Pts',(2.07865985827594,1.10551465762695,19.7392191793835));
#27589=CARTESIAN_POINT('Ctrl Pts',(0.19594130680613,2.34618764571867,19.8663751768002));
#27590=CARTESIAN_POINT('Ctrl Pts',(-1.86648996884708,1.43499291316336,19.9935311742169));
#27591=CARTESIAN_POINT('Ctrl Pts',(-2.21702086764734,-0.792343320191474,
20.1206871716337));
#27592=CARTESIAN_POINT('Ctrl Pts',(-0.534152754311119,-2.29296103318344,
20.2478431690504));
#27593=CARTESIAN_POINT('Ctrl Pts',(1.63862760964762,-1.6905292134525,20.3749991664672));
#27594=CARTESIAN_POINT('Ctrl Pts',(2.30849755388944,0.462415947305307,20.5021551638839));
#27595=CARTESIAN_POINT('Ctrl Pts',(0.861068236722175,2.19124415717281,20.6293111613006));
#27596=CARTESIAN_POINT('Ctrl Pts',(-1.37611246595686,1.91031514302587,20.7564671587174));
#27597=CARTESIAN_POINT('Ctrl Pts',(-2.3511554189652,-0.122709659385003,
20.8836231561341));
#27598=CARTESIAN_POINT('Ctrl Pts',(-1.1697743274058,-2.04318806955652,21.0107791535509));
#27599=CARTESIAN_POINT('Ctrl Pts',(1.08449606189562,-2.08970279139611,21.1379351509675));
#27600=CARTESIAN_POINT('Ctrl Pts',(2.34409235809092,-0.219591624101475,
21.2650911483843));
#27601=CARTESIAN_POINT('Ctrl Pts',(1.45374268180793,1.85192377805506,21.392247145801));
#27602=CARTESIAN_POINT('Ctrl Pts',(-0.769945338838868,2.2248985684377,21.5194031432178));
#27603=CARTESIAN_POINT('Ctrl Pts',(-2.2874577369461,0.557249106164581,21.6465591406345));
#27604=CARTESIAN_POINT('Ctrl Pts',(-1.70696809525024,-1.62149603343134,
21.7737151380513));
#27605=CARTESIAN_POINT('Ctrl Pts',(0.439112240372472,-2.31304342911907,
21.9008711354679));
#27606=CARTESIAN_POINT('Ctrl Pts',(2.18244923297112,-0.88312219434208,22.0280271328848));
#27607=CARTESIAN_POINT('Ctrl Pts',(1.92409549765578,1.35677779335326,22.1551831303014));
#27608=CARTESIAN_POINT('Ctrl Pts',(-0.0989930406933855,2.35227333499533,
22.2823391277182));
#27609=CARTESIAN_POINT('Ctrl Pts',(-2.0312875075515,1.19031950597351,22.4094951251349));
#27610=CARTESIAN_POINT('Ctrl Pts',(-2.10053319958978,-1.06336717179764,
22.5366511225517));
#27611=CARTESIAN_POINT('Ctrl Pts',(-0.243219608702475,-2.3417586738557,
22.6638071199684));
#27612=CARTESIAN_POINT('Ctrl Pts',(1.83716924470714,-1.47234460332425,22.7909631173852));
#27613=CARTESIAN_POINT('Ctrl Pts',(2.23254999475177,0.74746905325216,22.9181191148019));
#27614=CARTESIAN_POINT('Ctrl Pts',(0.580288785209907,2.2817218039006,23.0452751122186));
#27615=CARTESIAN_POINT('Ctrl Pts',(-1.60419954939816,1.72323337663434,23.1724311096353));
#27616=CARTESIAN_POINT('Ctrl Pts',(-2.31735406544925,-0.415763875272499,
23.2995871070521));
#27617=CARTESIAN_POINT('Ctrl Pts',(-0.905086337525095,-2.17343235143429,
23.4267431044688));
#27618=CARTESIAN_POINT('Ctrl Pts',(1.33730513505049,-1.93768016979155,23.5538991018855));
#27619=CARTESIAN_POINT('Ctrl Pts',(2.35315202240421,0.0752663543075803,
23.6810550993023));
#27620=CARTESIAN_POINT('Ctrl Pts',(1.21074362782129,2.01918036151453,23.808211096719));
#27621=CARTESIAN_POINT('Ctrl Pts',(-1.04213013616294,2.11114998139328,23.9353670941358));
#27622=CARTESIAN_POINT('Ctrl Pts',(-2.33918683035109,0.266822857618686,
24.0625230915525));
#27623=CARTESIAN_POINT('Ctrl Pts',(-1.49079678587771,-1.82222786935457,
24.1896790889692));
#27624=CARTESIAN_POINT('Ctrl Pts',(0.724916749292811,-2.2399743684316,24.316835086386));
#27625=CARTESIAN_POINT('Ctrl Pts',(2.27575381739723,-0.603269448287994,
24.4439910838027));
#27626=CARTESIAN_POINT('Ctrl Pts',(1.7393234034089,1.5867399166183,24.5711470812195));
#27627=CARTESIAN_POINT('Ctrl Pts',(-0.392373226558104,2.32142902448388,
24.6983030786362));
#27628=CARTESIAN_POINT('Ctrl Pts',(-2.16419442958846,0.926958432495279,
24.8254590760529));
#27629=CARTESIAN_POINT('Ctrl Pts',(-1.95106777785804,-1.31769647143789,
24.9526150734696));
#27630=CARTESIAN_POINT('Ctrl Pts',(0.0515320132559884,-2.35379139182843,
25.0797710708864));
#27631=CARTESIAN_POINT('Ctrl Pts',(2.00686786275484,-1.23104461579491,25.2069270683031));
#27632=CARTESIAN_POINT('Ctrl Pts',(2.12155205706895,1.02078711481988,25.3340830657199));
#27633=CARTESIAN_POINT('Ctrl Pts',(0.290398970375423,2.33637708913623,25.4612390631366));
#27634=CARTESIAN_POINT('Ctrl Pts',(-1.8071011715506,1.50909735286238,25.5883950605534));
#27635=CARTESIAN_POINT('Ctrl Pts',(-2.24717093441076,-0.702290720553313,
25.7155510579701));
#27636=CARTESIAN_POINT('Ctrl Pts',(-0.626188758241757,-2.26955438438638,
25.8427070553868));
#27637=CARTESIAN_POINT('Ctrl Pts',(1.56911891075444,-1.75523653920166,25.9698630528035));
#27638=CARTESIAN_POINT('Ctrl Pts',(2.3252678917954,0.368942673082406,26.0970190502203));
#27639=CARTESIAN_POINT('Ctrl Pts',(0.948736254837979,2.15473640693979,26.224175047637));
#27640=CARTESIAN_POINT('Ctrl Pts',(-1.2979537967368,1.96425696032171,26.3513310450538));
#27641=CARTESIAN_POINT('Ctrl Pts',(-2.35419137824343,-0.0277924313455661,
26.4784870424705));
#27642=CARTESIAN_POINT('Ctrl Pts',(-1.25122040526302,-1.9943512634662,26.6056430398872));
#27643=CARTESIAN_POINT('Ctrl Pts',(0.999340278375681,-2.13173836871502,
26.7327990373039));
#27644=CARTESIAN_POINT('Ctrl Pts',(2.33332973596469,-0.313945549257759,
26.8599550347207));
#27645=CARTESIAN_POINT('Ctrl Pts',(1.52724444309176,1.79179068969598,26.9871110321374));
#27646=CARTESIAN_POINT('Ctrl Pts',(-0.679593268124104,2.25413896079106,
27.1142670295542));
#27647=CARTESIAN_POINT('Ctrl Pts',(-2.26312413535676,0.649044384153771,
27.2414230269709));
#27648=CARTESIAN_POINT('Ctrl Pts',(-1.77097116563029,-1.55133832388099,
27.3685790243877));
#27649=CARTESIAN_POINT('Ctrl Pts',(0.345474597756808,-2.32887027696704,
27.4957350218043));
#27650=CARTESIAN_POINT('Ctrl Pts',(2.14505924537894,-0.970417589726265,
27.6228910192211));
#27651=CARTESIAN_POINT('Ctrl Pts',(1.97724637582914,1.27807911879756,27.7500470166378));
#27652=CARTESIAN_POINT('Ctrl Pts',(-0.00405002291626669,2.3543519409702,
27.8772030140546));
#27653=CARTESIAN_POINT('Ctrl Pts',(-1.9816318365997,1.27126894432701,28.0043590114713));
#27654=CARTESIAN_POINT('Ctrl Pts',(-2.14170788037307,-0.977791807995794,
28.131515008888));
#27655=CARTESIAN_POINT('Ctrl Pts',(-0.33746019955431,-2.33004508075543,
28.2586710063048));
#27656=CARTESIAN_POINT('Ctrl Pts',(1.77629798088247,-1.54523621098804,28.3858270037215));
#27657=CARTESIAN_POINT('Ctrl Pts',(2.26087773891706,0.65682670035945,28.5129830011383));
#27658=CARTESIAN_POINT('Ctrl Pts',(0.671834001583367,2.2564637242713,28.640138998555));
#27659=CARTESIAN_POINT('Ctrl Pts',(-1.53339996430195,1.78652568246711,28.7672949959717));
#27660=CARTESIAN_POINT('Ctrl Pts',(-2.33223581363256,-0.321971387308704,
28.8944509933885));
#27661=CARTESIAN_POINT('Ctrl Pts',(-0.992000232146069,-2.13516392908319,
29.0216069908052));
#27662=CARTESIAN_POINT('Ctrl Pts',(1.25807445889537,-1.99003470334338,29.148762988222));
#27663=CARTESIAN_POINT('Ctrl Pts',(2.35427306367935,-0.0196927974045315,
29.2759189856387));
#27664=CARTESIAN_POINT('Ctrl Pts',(1.29118819402983,1.96871087573412,29.4030749830554));
#27665=CARTESIAN_POINT('Ctrl Pts',(-0.956143895181802,2.1514595781335,29.5302309804722));
#27666=CARTESIAN_POINT('Ctrl Pts',(-2.32652345756126,0.360940529800938,
29.6573869778889));
#27667=CARTESIAN_POINT('Ctrl Pts',(-1.5630708267699,-1.76062462073453,29.7845429753057));
#27668=CARTESIAN_POINT('Ctrl Pts',(0.633993332642798,-2.2673865834481,29.9116989727223));
#27669=CARTESIAN_POINT('Ctrl Pts',(2.24957382850068,-0.694555292802842,
30.0388549701391));
#27670=CARTESIAN_POINT('Ctrl Pts',(1.80189850780172,1.51530565636686,30.1660109675558));
#27671=CARTESIAN_POINT('Ctrl Pts',(-0.298435432038931,2.33536415951361,
30.2931669649726));
#27672=CARTESIAN_POINT('Ctrl Pts',(-2.12505146441632,1.0134819871199,30.4203229623893));
#27673=CARTESIAN_POINT('Ctrl Pts',(-2.00262064227849,-1.23794185152384,
30.547478959806));
#27674=CARTESIAN_POINT('Ctrl Pts',(-0.0434336149472678,-2.35395475439451,
30.6746349572228));
#27675=CARTESIAN_POINT('Ctrl Pts',(1.95558969494388,-1.31097612855999,30.8017909546395));
#27676=CARTESIAN_POINT('Ctrl Pts',(2.16099247023974,0.934398741542428,30.9289469520563));
#27677=CARTESIAN_POINT('Ctrl Pts',(0.384384152021792,2.32276522454689,31.056102949473));
#27678=CARTESIAN_POINT('Ctrl Pts',(-1.74477220324497,1.58074647661569,31.1832589468898));
#27679=CARTESIAN_POINT('Ctrl Pts',(-2.2736648324357,-0.611095487107494,
31.3104149443064));
#27680=CARTESIAN_POINT('Ctrl Pts',(-0.717205947018836,-2.24245514883759,
31.4375709417232));
#27681=CARTESIAN_POINT('Ctrl Pts',(1.49705724025751,-1.81708807804335,31.5647269391399));
#27682=CARTESIAN_POINT('Ctrl Pts',(2.33825499650753,0.274869125275902,31.6918829365567));
#27683=CARTESIAN_POINT('Ctrl Pts',(1.03486066982954,2.11472288040308,31.8190389339733));
#27684=CARTESIAN_POINT('Ctrl Pts',(-1.21768334399615,2.01500291153206,31.9461949313902));
#27685=CARTESIAN_POINT('Ctrl Pts',(-2.35339704585751,0.0671700173426187,
32.0733509288068));
#27686=CARTESIAN_POINT('Ctrl Pts',(-1.33063073475968,-1.94226963266362,
32.2005069262237));
#27687=CARTESIAN_POINT('Ctrl Pts',(0.912558557239173,-2.17030557956596,
32.3276629236403));
#27688=CARTESIAN_POINT('Ctrl Pts',(2.31877076648926,-0.407788696506587,
32.4548189210572));
#27689=CARTESIAN_POINT('Ctrl Pts',(1.59826135801109,1.72874236832532,32.5819749184737));
#27690=CARTESIAN_POINT('Ctrl Pts',(-0.588135483178816,2.27971179455285,
32.7091309158906));
#27691=CARTESIAN_POINT('Ctrl Pts',(-2.23510842700854,0.739783761350988,
32.8362869133073));
#27692=CARTESIAN_POINT('Ctrl Pts',(-1.83209281455498,-1.47865676388438,
32.963442910724));
#27693=CARTESIAN_POINT('Ctrl Pts',(0.251274799212049,-2.34090766448235,
33.0905989081408));
#27694=CARTESIAN_POINT('Ctrl Pts',(2.10417935049844,-1.05613480412643,33.2177549055575));
#27695=CARTESIAN_POINT('Ctrl Pts',(2.02718001724375,1.19730232763188,33.3449109029743));
#27696=CARTESIAN_POINT('Ctrl Pts',(0.0909000378197398,2.35259745701308,
33.4720669003909));
#27697=CARTESIAN_POINT('Ctrl Pts',(-1.92875289630088,1.35015485239774,33.5992228978078));
#27698=CARTESIAN_POINT('Ctrl Pts',(-2.17939633307122,-0.890634789104744,
33.7263788952244));
#27699=CARTESIAN_POINT('Ctrl Pts',(-0.43115488299765,-2.31452289945943,
33.8535348926412));
#27700=CARTESIAN_POINT('Ctrl Pts',(1.71254265687404,-1.61564722812947,33.9806908900579));
#27701=CARTESIAN_POINT('Ctrl Pts',(2.28551558525492,0.56517960272398,34.1078468874747));
#27702=CARTESIAN_POINT('Ctrl Pts',(0.762307926725003,2.22741248100854,34.2350028848914));
#27703=CARTESIAN_POINT('Ctrl Pts',(-1.4601470665852,1.8471437087484,34.3621588823081));
#27704=CARTESIAN_POINT('Ctrl Pts',(-2.34324378646556,-0.228098537668562,
34.4893148797248));
#27705=CARTESIAN_POINT('Ctrl Pts',(-1.07745110930829,-2.09257290386258,
34.6164708771416));
#27706=CARTESIAN_POINT('Ctrl Pts',(1.17708439401579,-2.04079654697071,34.7436268745583));
#27707=CARTESIAN_POINT('Ctrl Pts',(2.35117936578161,-0.110982933612702,
34.8708003673951));
#27708=CARTESIAN_POINT('Ctrl Pts',(1.69716715890499,1.23460437476058,34.9555885277595));
#27709=CARTESIAN_POINT('Ctrl Pts',(1.15760455782972,1.6201078652314,34.9979913556517));
#27710=CARTESIAN_POINT('Ctrl Pts',(-0.940860907222522,1.92803476961866,
4.82379972005017));
#27711=CARTESIAN_POINT('Ctrl Pts',(-1.58281548406976,1.61477906238341,4.86619281462993));
#27712=CARTESIAN_POINT('Ctrl Pts',(-2.51789878139056,0.302100165074653,
4.95097124168192));
#27713=CARTESIAN_POINT('Ctrl Pts',(-1.6153773455708,-1.95798749074765,5.07813500120616));
#27714=CARTESIAN_POINT('Ctrl Pts',(0.770818542691949,-2.41592098549706,
5.2052909986229));
#27715=CARTESIAN_POINT('Ctrl Pts',(2.44893709210338,-0.661129782966532,
5.33244699603964));
#27716=CARTESIAN_POINT('Ctrl Pts',(1.88152327214964,1.70164314936676,5.45960299345635));
#27717=CARTESIAN_POINT('Ctrl Pts',(-0.41188023327182,2.50286729587259,5.58675899087311));
#27718=CARTESIAN_POINT('Ctrl Pts',(-2.32735905164794,1.00896224840214,5.71391498828984));
#27719=CARTESIAN_POINT('Ctrl Pts',(-2.10832209870648,-1.41057054174251,
5.84107098570658));
#27720=CARTESIAN_POINT('Ctrl Pts',(0.044461361955423,-2.53624005146705,
5.96822698312332));
#27721=CARTESIAN_POINT('Ctrl Pts',(2.15644313623853,-1.3357939482761,6.09538298054004));
#27722=CARTESIAN_POINT('Ctrl Pts',(2.29059830525902,1.08984410967345,6.2225389779568));
#27723=CARTESIAN_POINT('Ctrl Pts',(0.323864713742656,2.51588545724566,6.34969497537351));
#27724=CARTESIAN_POINT('Ctrl Pts',(-1.93990663359876,1.63442545808399,6.47685097279027));
#27725=CARTESIAN_POINT('Ctrl Pts',(-2.4244433022373,-0.746095664807696,
6.60400697020699));
#27726=CARTESIAN_POINT('Ctrl Pts',(-0.685337112179472,-2.44231299424555,
6.73116296762373));
#27727=CARTESIAN_POINT('Ctrl Pts',(1.68234356541504,-1.8985000361444,6.85831896504046));
#27728=CARTESIAN_POINT('Ctrl Pts',(2.50701883308963,0.386572869208354,6.98547496245721));
#27729=CARTESIAN_POINT('Ctrl Pts',(1.0323156951975,2.31708993340106,7.11263095987393));
#27730=CARTESIAN_POINT('Ctrl Pts',(-1.38920287136656,2.12242720047753,7.23978695729069));
#27731=CARTESIAN_POINT('Ctrl Pts',(-2.53657751444396,-0.0188755745349083,
7.36694295470739));
#27732=CARTESIAN_POINT('Ctrl Pts',(-1.35746334135277,-2.14286606720562,
7.49409895212416));
#27733=CARTESIAN_POINT('Ctrl Pts',(1.06668403630552,-2.30147060134743,7.62125494954088));
#27734=CARTESIAN_POINT('Ctrl Pts',(2.51249409388617,-0.349220813994871,
7.74841094695762));
#27735=CARTESIAN_POINT('Ctrl Pts',(1.65390409412917,1.92332602230935,7.87556694437436));
#27736=CARTESIAN_POINT('Ctrl Pts',(-0.721607553543116,2.43184380411619,
8.00272294179109));
#27737=CARTESIAN_POINT('Ctrl Pts',(-2.4352778508332,0.709932064149893,8.12987893920782));
#27738=CARTESIAN_POINT('Ctrl Pts',(-1.91536900175952,-1.66311254360542,
8.25703493662456));
#27739=CARTESIAN_POINT('Ctrl Pts',(0.361270914862585,-2.51078973091116,
8.3841909340413));
#27740=CARTESIAN_POINT('Ctrl Pts',(2.30656170803872,-1.05563006463211,8.51134693145805));
#27741=CARTESIAN_POINT('Ctrl Pts',(2.13632875169771,1.36772848582442,8.63850292887476));
#27742=CARTESIAN_POINT('Ctrl Pts',(0.00670568016803455,2.5366388746297,
8.76565892629152));
#27743=CARTESIAN_POINT('Ctrl Pts',(-2.12906768235024,1.3790041879306,8.89281492370824));
#27744=CARTESIAN_POINT('Ctrl Pts',(-2.31211061041173,-1.04342046729742,
9.01997092112498));
#27745=CARTESIAN_POINT('Ctrl Pts',(-0.374540467229969,-2.5088445915965,
9.14712691854171));
#27746=CARTESIAN_POINT('Ctrl Pts',(1.90654931854483,-1.67321589829907,9.27428291595846));
#27747=CARTESIAN_POINT('Ctrl Pts',(2.4389972410452,0.697046773565979,9.40143891337518));
#27748=CARTESIAN_POINT('Ctrl Pts',(0.734454680994803,2.42799465978255,9.52859491079192));
#27749=CARTESIAN_POINT('Ctrl Pts',(-1.64371231109775,1.9320433702978,9.65575090820866));
#27750=CARTESIAN_POINT('Ctrl Pts',(-2.51430531577452,-0.33593232269935,
9.7829069056254));
#27751=CARTESIAN_POINT('Ctrl Pts',(-1.07883705602549,-2.29579884853026,
9.91006290304212));
#27752=CARTESIAN_POINT('Ctrl Pts',(1.34611499072393,-2.15001306463813,10.0372189004589));
#27753=CARTESIAN_POINT('Ctrl Pts',(2.53644226135888,-0.0322862379199884,
10.1643748978756));
#27754=CARTESIAN_POINT('Ctrl Pts',(1.40040478556657,2.11505276126358,10.2915308952924));
#27755=CARTESIAN_POINT('Ctrl Pts',(-1.0200507798868,2.32251547956493,10.4186868927091));
#27756=CARTESIAN_POINT('Ctrl Pts',(-2.50493993799644,0.399822027153037,
10.5458428901259));
#27757=CARTESIAN_POINT('Ctrl Pts',(-1.69235753428521,-1.88957871561744,
10.6729988875426));
#27758=CARTESIAN_POINT('Ctrl Pts',(0.672415103002414,-2.44590263003674,
10.8001548849593));
#27759=CARTESIAN_POINT('Ctrl Pts',(2.42046453928486,-0.758902602730359,
10.927310882376));
#27760=CARTESIAN_POINT('Ctrl Pts',(1.94852124797693,1.62414491119137,11.0544668797928));
#27761=CARTESIAN_POINT('Ctrl Pts',(-0.31055956584235,2.51756519328303,11.1816228772095));
#27762=CARTESIAN_POINT('Ctrl Pts',(-2.28480250393,1.10193432853396,11.3087788746263));
#27763=CARTESIAN_POINT('Ctrl Pts',(-2.16347871902673,-1.32436459431867,
11.435934872043));
#27764=CARTESIAN_POINT('Ctrl Pts',(-0.0578635121326518,-2.53598768930965,
11.5630908694597));
#27765=CARTESIAN_POINT('Ctrl Pts',(2.10082273713468,-1.42166296058678,11.6902468668765));
#27766=CARTESIAN_POINT('Ctrl Pts',(2.33268414650022,0.996577352257691,11.8174028642932));
#27767=CARTESIAN_POINT('Ctrl Pts',(0.425062924764753,2.50078052942613,11.94455886171));
#27768=CARTESIAN_POINT('Ctrl Pts',(-1.87241594058851,1.71132705576591,12.0717148591266));
#27769=CARTESIAN_POINT('Ctrl Pts',(-2.4525592682111,-0.647715047129689,
12.1988708565434));
#27770=CARTESIAN_POINT('Ctrl Pts',(-0.783273343289587,-2.41268825505044,
12.3260268539601));
#27771=CARTESIAN_POINT('Ctrl Pts',(1.60441233407452,-1.96480095903783,12.4531828513769));
#27772=CARTESIAN_POINT('Ctrl Pts',(2.52056903181798,0.285155224757529,12.5803388487936));
#27773=CARTESIAN_POINT('Ctrl Pts',(1.12491953318614,2.27357379256154,12.7074948462104));
#27774=CARTESIAN_POINT('Ctrl Pts',(-1.30247950866994,2.17672434540097,12.8346508436271));
#27775=CARTESIAN_POINT('Ctrl Pts',(-2.53527520470006,0.083434901566532,
12.9618068410438));
#27776=CARTESIAN_POINT('Ctrl Pts',(-1.44277655101942,-2.08637905716934,
13.0889628384605));
#27777=CARTESIAN_POINT('Ctrl Pts',(0.973002571685308,-2.34261557705487,
13.2161188358773));
#27778=CARTESIAN_POINT('Ctrl Pts',(2.4963667888999,-0.450260593039129,13.343274833294));
#27779=CARTESIAN_POINT('Ctrl Pts',(1.73012253352216,1.85506273892967,13.4704308307108));
#27780=CARTESIAN_POINT('Ctrl Pts',(-0.622949117969492,2.45896647858148,
13.5975868281275));
#27781=CARTESIAN_POINT('Ctrl Pts',(-2.40466659793517,0.807564424142928,
13.7247428255442));
#27782=CARTESIAN_POINT('Ctrl Pts',(-1.98088084781725,-1.58451658657056,
13.851898822961));
#27783=CARTESIAN_POINT('Ctrl Pts',(0.259721883092581,-2.52331652588598,
13.9790548203777));
#27784=CARTESIAN_POINT('Ctrl Pts',(2.26211385639636,-1.14779033236301,14.1062108177944));
#27785=CARTESIAN_POINT('Ctrl Pts',(2.18974859666703,1.28046195951349,14.2333668152112));
#27786=CARTESIAN_POINT('Ctrl Pts',(0.108997805584984,2.53430487999057,14.3605228126279));
#27787=CARTESIAN_POINT('Ctrl Pts',(-2.07172319030473,1.46374340959063,14.4876788100447));
#27788=CARTESIAN_POINT('Ctrl Pts',(-2.35230876119222,-0.949328835749087,
14.6148348074614));
#27789=CARTESIAN_POINT('Ctrl Pts',(-0.475412469347375,-2.49169916529974,
14.7419908048781));
#27790=CARTESIAN_POINT('Ctrl Pts',(1.83752087547937,-1.74874205603454,14.8691468022949));
#27791=CARTESIAN_POINT('Ctrl Pts',(2.465123609528,0.598119834242293,14.9963027997116));
#27792=CARTESIAN_POINT('Ctrl Pts',(0.831773374862453,2.39640038374982,15.1234587971283));
#27793=CARTESIAN_POINT('Ctrl Pts',(-1.56445969209756,1.9967592789739,15.2506147945451));
#27794=CARTESIAN_POINT('Ctrl Pts',(-2.52580739606398,-0.234262127444595,
15.3777707919618));
#27795=CARTESIAN_POINT('Ctrl Pts',(-1.17054440008075,-2.25042386092176,
15.5049267893785));
#27796=CARTESIAN_POINT('Ctrl Pts',(1.25831418605672,-2.20255014824516,15.6320827867953));
#27797=CARTESIAN_POINT('Ctrl Pts',(2.53307681386418,-0.134549624414361,
15.759238784212));
#27798=CARTESIAN_POINT('Ctrl Pts',(1.48456140394928,2.05685662705754,15.8863947816287));
#27799=CARTESIAN_POINT('Ctrl Pts',(-0.925558552092357,2.36176271310543,
16.0135507790455));
#27800=CARTESIAN_POINT('Ctrl Pts',(-2.48677813332775,0.500515995717766,
16.1407067764622));
#27801=CARTESIAN_POINT('Ctrl Pts',(-1.76718372967845,-1.81979213426318,
16.267862773879));
#27802=CARTESIAN_POINT('Ctrl Pts',(0.573229721111829,-2.47103003486409,
16.3950187712957));
#27803=CARTESIAN_POINT('Ctrl Pts',(2.38789045317691,-0.855897733372941,
16.5221747687124));
#27804=CARTESIAN_POINT('Ctrl Pts',(2.01243463765503,1.54424369046231,16.6493307661292));
#27805=CARTESIAN_POINT('Ctrl Pts',(-0.208778547096946,2.52804138902797,
16.7764867635459));
#27806=CARTESIAN_POINT('Ctrl Pts',(-2.23850499502235,1.19317942222719,16.9036427609626));
#27807=CARTESIAN_POINT('Ctrl Pts',(-2.21512769820434,-1.23603844075105,
17.0307987583794));
#27808=CARTESIAN_POINT('Ctrl Pts',(-0.160087759408297,-2.53159113121649,
17.1579547557961));
#27809=CARTESIAN_POINT('Ctrl Pts',(2.04178087937262,-1.50522841688388,17.2851107532128));
#27810=CARTESIAN_POINT('Ctrl Pts',(2.37097647131784,0.901694138177437,17.4122667506296));
#27811=CARTESIAN_POINT('Ctrl Pts',(0.525568619095842,2.48160419345794,17.5394227480463));
#27812=CARTESIAN_POINT('Ctrl Pts',(-1.80187831831236,1.78544567891668,17.6665787454631));
#27813=CARTESIAN_POINT('Ctrl Pts',(-2.47668515390022,-0.548281309928203,
17.7937347428798));
#27814=CARTESIAN_POINT('Ctrl Pts',(-0.879935046202314,-2.37913767168513,
17.9208907402965));
#27815=CARTESIAN_POINT('Ctrl Pts',(1.52387063765299,-2.0279053296605,18.0480467377133));
#27816=CARTESIAN_POINT('Ctrl Pts',(2.53001827757856,0.183273733755983,18.17520273513));
#27817=CARTESIAN_POINT('Ctrl Pts',(1.21569309679729,2.22635847085903,18.3023587325467));
#27818=CARTESIAN_POINT('Ctrl Pts',(-1.21363698906272,2.2274799673948,18.4295147299635));
#27819=CARTESIAN_POINT('Ctrl Pts',(-2.52984798314295,0.185609613312194,
18.5566707273802));
#27820=CARTESIAN_POINT('Ctrl Pts',(-1.52574234653794,-2.02649748046901,
18.6838267247969));
#27821=CARTESIAN_POINT('Ctrl Pts',(0.877738021039851,-2.37994909878077,
18.8109827222137));
#27822=CARTESIAN_POINT('Ctrl Pts',(2.47617787188537,-0.550567791603931,
18.9381387196304));
#27823=CARTESIAN_POINT('Ctrl Pts',(1.80352604649014,1.78378124948045,19.0652947170472));
#27824=CARTESIAN_POINT('Ctrl Pts',(-0.523277137970608,2.48208839150496,
19.1924507144639));
#27825=CARTESIAN_POINT('Ctrl Pts',(-2.37014292944138,0.903882868731024,
19.3196067118806));
#27826=CARTESIAN_POINT('Ctrl Pts',(-2.04316978160497,-1.50334260563009,
19.4467627092973));
#27827=CARTESIAN_POINT('Ctrl Pts',(0.157750281287492,-2.53173786066411,
19.5739187067141));
#27828=CARTESIAN_POINT('Ctrl Pts',(2.21398552374585,-1.23808313412719,19.7010747041308));
#27829=CARTESIAN_POINT('Ctrl Pts',(2.23960569957805,1.1911121092424,19.8282307015476));
#27830=CARTESIAN_POINT('Ctrl Pts',(0.211112590527258,2.52784754692352,19.9553866989643));
#27831=CARTESIAN_POINT('Ctrl Pts',(-2.01100798468413,1.54610110662371,20.082542696381));
#27832=CARTESIAN_POINT('Ctrl Pts',(-2.38867968296877,-0.853692637041341,
20.2096986937978));
#27833=CARTESIAN_POINT('Ctrl Pts',(-0.575510970800485,-2.47049972047249,
20.3368546912145));
#27834=CARTESIAN_POINT('Ctrl Pts',(1.76550276825797,-1.82142299360686,20.4640106886313));
#27835=CARTESIAN_POINT('Ctrl Pts',(2.48723919816346,0.498219748189033,20.591166686048));
#27836=CARTESIAN_POINT('Ctrl Pts',(0.927738765440914,2.36090714122021,20.7183226834647));
#27837=CARTESIAN_POINT('Ctrl Pts',(-1.48266168211557,2.058226441078,20.8454786808814));
#27838=CARTESIAN_POINT('Ctrl Pts',(-2.5331999634013,-0.132210785452896,
20.9726346782982));
#27839=CARTESIAN_POINT('Ctrl Pts',(-1.26034725712697,-2.20138741202427,
21.0997906757149));
#27840=CARTESIAN_POINT('Ctrl Pts',(1.1684660920936,-2.25150366155463,21.2269466731317));
#27841=CARTESIAN_POINT('Ctrl Pts',(2.52559002600461,-0.236594097374377,
21.3541026705484));
#27842=CARTESIAN_POINT('Ctrl Pts',(1.56630262663429,1.99531396731565,21.4812586679652));
#27843=CARTESIAN_POINT('Ctrl Pts',(-0.829560431622247,2.39716733597241,
21.6084146653818));
#27844=CARTESIAN_POINT('Ctrl Pts',(-2.46457031669317,0.600395619938505,
21.7355706627986));
#27845=CARTESIAN_POINT('Ctrl Pts',(-1.8391347001289,-1.74704473358531,21.8627266602153));
#27846=CARTESIAN_POINT('Ctrl Pts',(0.473111688945822,-2.49213705003341,
21.9898826576321));
#27847=CARTESIAN_POINT('Ctrl Pts',(2.35143124631078,-0.9515003101627,22.1170386550488));
#27848=CARTESIAN_POINT('Ctrl Pts',(2.07307377680177,1.46182997038069,22.2441946524656));
#27849=CARTESIAN_POINT('Ctrl Pts',(-0.106657843645223,2.53440443709273,
22.3713506498822));
#27850=CARTESIAN_POINT('Ctrl Pts',(-2.18856541693521,1.28248320151244,22.4985066472991));
#27851=CARTESIAN_POINT('Ctrl Pts',(-2.26317264328954,-1.1457012407396,22.6256626447157));
#27852=CARTESIAN_POINT('Ctrl Pts',(-0.262051542358103,-2.52307564997844,
22.7528186421325));
#27853=CARTESIAN_POINT('Ctrl Pts',(1.97941702446132,-1.58634485205427,22.8799746395492));
#27854=CARTESIAN_POINT('Ctrl Pts',(2.40541119458867,0.805343859052706,23.007130636966));
#27855=CARTESIAN_POINT('Ctrl Pts',(0.625219208223486,2.45839026357387,23.1342866343827));
#27856=CARTESIAN_POINT('Ctrl Pts',(-1.72840902266361,1.85665936475742,23.2614426317994));
#27857=CARTESIAN_POINT('Ctrl Pts',(-2.49678144899819,-0.447955513756536,
23.3885986292162));
#27858=CARTESIAN_POINT('Ctrl Pts',(-0.975165086322767,-2.3417162084214,
23.5157546266329));
#27859=CARTESIAN_POINT('Ctrl Pts',(1.440849589032,-2.08771027878695,23.6429106240497));
#27860=CARTESIAN_POINT('Ctrl Pts',(2.53535115924222,0.0810940546250112,
23.7700666214663));
#27861=CARTESIAN_POINT('Ctrl Pts',(1.30448871603519,2.17552084248882,23.8972226188832));
#27862=CARTESIAN_POINT('Ctrl Pts',(-1.12281987038924,2.2746114580353,24.0243786162998));
#27863=CARTESIAN_POINT('Ctrl Pts',(-2.52030467455963,0.287482336429987,
24.1515346137166));
#27864=CARTESIAN_POINT('Ctrl Pts',(-1.60622574456868,-1.9633187728566,24.2786906111333));
#27865=CARTESIAN_POINT('Ctrl Pts',(0.781045382183157,-2.41341042040858,
24.4058466085501));
#27866=CARTESIAN_POINT('Ctrl Pts',(2.45196018963237,-0.649979211070922,
24.5330026059668));
#27867=CARTESIAN_POINT('Ctrl Pts',(1.87399520521599,1.70959753076386,24.6601586033835));
#27868=CARTESIAN_POINT('Ctrl Pts',(-0.42275378103003,2.50117192271767,24.7873146008003));
#27869=CARTESIAN_POINT('Ctrl Pts',(-2.33176301558138,0.998730687189076,
24.914470598217));
#27870=CARTESIAN_POINT('Ctrl Pts',(-2.10213445848623,-1.41972267179587,
25.0416265956337));
#27871=CARTESIAN_POINT('Ctrl Pts',(0.0555220182558873,-2.53604003356715,
25.1687825930505));
#27872=CARTESIAN_POINT('Ctrl Pts',(2.16225501533173,-1.32636156271175,25.2959385904672));
#27873=CARTESIAN_POINT('Ctrl Pts',(2.2858189424527,1.09982430810144,25.4230945878839));
#27874=CARTESIAN_POINT('Ctrl Pts',(0.312883893252119,2.51727738155925,25.5502505853007));
#27875=CARTESIAN_POINT('Ctrl Pts',(-1.94702084971026,1.6259432822703,25.6774065827174));
#27876=CARTESIAN_POINT('Ctrl Pts',(-2.42116419990269,-0.756667472193677,
25.8045625801342));
#27877=CARTESIAN_POINT('Ctrl Pts',(-0.674673110363047,-2.44528074881381,
25.9317185775509));
#27878=CARTESIAN_POINT('Ctrl Pts',(1.69061217103417,-1.89114045843176,26.0588745749677));
#27879=CARTESIAN_POINT('Ctrl Pts',(2.50530802467614,0.397509053808538,26.1860305723843));
#27880=CARTESIAN_POINT('Ctrl Pts',(1.02219471611566,2.32157268004076,26.3131865698011));
#27881=CARTESIAN_POINT('Ctrl Pts',(-1.39845136730157,2.11634484894564,26.4403425672178));
#27882=CARTESIAN_POINT('Ctrl Pts',(-2.53647099000825,-0.0299443352403086,
26.5674985646346));
#27883=CARTESIAN_POINT('Ctrl Pts',(-1.34809951705112,-2.14876928461222,
26.6946545620513));
#27884=CARTESIAN_POINT('Ctrl Pts',(1.07671689254853,-2.29679395672904,26.8218105594681));
#27885=CARTESIAN_POINT('Ctrl Pts',(2.5139940788561,-0.338253629460036,26.9489665568847));
#27886=CARTESIAN_POINT('Ctrl Pts',(1.64549545986523,1.93052491253787,27.0761225543016));
#27887=CARTESIAN_POINT('Ctrl Pts',(-0.732212608342833,2.4286717445036,27.2032785517182));
#27888=CARTESIAN_POINT('Ctrl Pts',(-2.4383526204242,0.699298394704866,27.330434549135));
#27889=CARTESIAN_POINT('Ctrl Pts',(-1.90809338071484,-1.6714548743052,27.4575905465517));
#27890=CARTESIAN_POINT('Ctrl Pts',(0.372223899506801,-2.50918933422776,
27.5847465439684));
#27891=CARTESIAN_POINT('Ctrl Pts',(2.31114623816709,-1.04555478678664,27.7119025413852));
#27892=CARTESIAN_POINT('Ctrl Pts',(2.13034000495386,1.37703783886266,27.8390585388019));
#27893=CARTESIAN_POINT('Ctrl Pts',(-0.00436360685501822,2.53664398473684,
27.9662145362187));
#27894=CARTESIAN_POINT('Ctrl Pts',(-2.13506502184302,1.3697003682809,28.0933705336354));
#27895=CARTESIAN_POINT('Ctrl Pts',(-2.30753538469401,-1.05349997377856,
28.2205265310522));
#27896=CARTESIAN_POINT('Ctrl Pts',(-0.363588964925368,-2.51045510036544,
28.3476825284689));
#27897=CARTESIAN_POINT('Ctrl Pts',(1.91383263899322,-1.66488028887685,28.4748385258856));
#27898=CARTESIAN_POINT('Ctrl Pts',(2.43593229068633,0.707683277715432,28.6019945233023));
#27899=CARTESIAN_POINT('Ctrl Pts',(0.723852559679631,2.43117650906132,28.7291505207191));
#27900=CARTESIAN_POINT('Ctrl Pts',(-1.65212758889371,1.92485224793558,28.8563065181358));
#27901=CARTESIAN_POINT('Ctrl Pts',(-2.51281545663937,-0.34690088965101,
28.9834625155526));
#27902=CARTESIAN_POINT('Ctrl Pts',(-1.06880852345881,-2.30048475034028,
29.1106185129693));
#27903=CARTESIAN_POINT('Ctrl Pts',(1.35548426425704,-2.14411850318913,29.2377745103861));
#27904=CARTESIAN_POINT('Ctrl Pts',(2.53655900015918,-0.0212175653135828,
29.3649305078028));
#27905=CARTESIAN_POINT('Ctrl Pts',(1.39116191957229,2.12114362076176,29.4920865052195));
#27906=CARTESIAN_POINT('Ctrl Pts',(-1.03017591297604,2.31804213393337,29.6192425026363));
#27907=CARTESIAN_POINT('Ctrl Pts',(-2.50666080600506,0.388887323018423,
29.746398500053));
#27908=CARTESIAN_POINT('Ctrl Pts',(-1.68409579784808,-1.89694572669772,
29.8735544974697));
#27909=CARTESIAN_POINT('Ctrl Pts',(0.683081974969736,-2.44294510004585,
30.0007104948864));
#27910=CARTESIAN_POINT('Ctrl Pts',(2.42375314454311,-0.74833310810332,30.1278664923032));
#27911=CARTESIAN_POINT('Ctrl Pts',(1.94141535569991,1.63263228040444,30.2550224897199));
#27912=CARTESIAN_POINT('Ctrl Pts',(-0.321542599617489,2.51618602313084,
30.3821784871367));
#27913=CARTESIAN_POINT('Ctrl Pts',(-2.28958930084453,1.09195356120261,30.5093344845534));
#27914=CARTESIAN_POINT('Ctrl Pts',(-2.15767894236412,-1.33379283550446,
30.6364904819702));
#27915=CARTESIAN_POINT('Ctrl Pts',(-0.0467965796336351,-2.53621604492014,
30.7636464793869));
#27916=CARTESIAN_POINT('Ctrl Pts',(2.1070064971886,-1.4124819882599,30.8908024768036));
#27917=CARTESIAN_POINT('Ctrl Pts',(2.3283131359011,1.00674708221518,31.0179584742203));
#27918=CARTESIAN_POINT('Ctrl Pts',(0.414146130867886,2.50261158167149,31.1451144716371));
#27919=CARTESIAN_POINT('Ctrl Pts',(-1.8798658930634,1.70314003251725,31.2722704690538));
#27920=CARTESIAN_POINT('Ctrl Pts',(-2.44970945938055,-0.658411202036514,
31.3994264664706));
#27921=CARTESIAN_POINT('Ctrl Pts',(-0.772737550263181,-2.416083281923,31.5265824638873));
#27922=CARTESIAN_POINT('Ctrl Pts',(1.61297093150021,-1.95778101935183,31.653738461304));
#27923=CARTESIAN_POINT('Ctrl Pts',(2.51930069096952,0.296151608044552,31.7808944587208));
#27924=CARTESIAN_POINT('Ctrl Pts',(1.11498754603441,2.27846099837959,31.9080504561375));
#27925=CARTESIAN_POINT('Ctrl Pts',(-1.31196575843683,2.17101994218358,32.0352064535542));
#27926=CARTESIAN_POINT('Ctrl Pts',(-2.5356151542967,0.0723708369516123,
32.1623624509709));
#27927=CARTESIAN_POINT('Ctrl Pts',(-1.43365840531175,-2.0926550931901,32.2895184483877));
#27928=CARTESIAN_POINT('Ctrl Pts',(0.983215862785192,-2.33834733781478,
32.4166744458044));
#27929=CARTESIAN_POINT('Ctrl Pts',(2.4983078419341,-0.439362835282259,32.5438304432212));
#27930=CARTESIAN_POINT('Ctrl Pts',(1.72201105080549,1.86259490497632,32.6709864406379));
#27931=CARTESIAN_POINT('Ctrl Pts',(-0.633673457928804,2.45622462383557,
32.7981424380546));
#27932=CARTESIAN_POINT('Ctrl Pts',(-2.40816772035767,0.797063512714892,
32.9252984354714));
#27933=CARTESIAN_POINT('Ctrl Pts',(-1.9739475380241,-1.5931457486565,33.0524544328881));
#27934=CARTESIAN_POINT('Ctrl Pts',(0.270730427700916,-2.52215874891095,
33.1796104303049));
#27935=CARTESIAN_POINT('Ctrl Pts',(2.26710110725835,-1.13790888751085,33.3067664277216));
#27936=CARTESIAN_POINT('Ctrl Pts',(2.18413989312104,1.29000668695582,33.4339224251383));
#27937=CARTESIAN_POINT('Ctrl Pts',(0.0979382182141485,2.53475365513117,
33.5610784225551));
#27938=CARTESIAN_POINT('Ctrl Pts',(-2.07809178708825,1.45469423037344,33.6882344199718));
#27939=CARTESIAN_POINT('Ctrl Pts',(-2.34814196740883,-0.959594587820653,
33.8153904173885));
#27940=CARTESIAN_POINT('Ctrl Pts',(-0.46453821173187,-2.49373107235192,
33.9425464148053));
#27941=CARTESIAN_POINT('Ctrl Pts',(1.84514088720937,-1.74074306877094,34.069702412222));
#27942=CARTESIAN_POINT('Ctrl Pts',(2.46247778867336,0.608940156566012,34.1968584096388));
#27943=CARTESIAN_POINT('Ctrl Pts',(0.821331672293306,2.39987589499884,34.3240144070555));
#27944=CARTESIAN_POINT('Ctrl Pts',(-1.5732028881622,1.99016378826106,34.4511704044722));
#27945=CARTESIAN_POINT('Ctrl Pts',(-2.52467575143432,-0.245759681649779,
34.5783264018889));
#27946=CARTESIAN_POINT('Ctrl Pts',(-1.16087566506667,-2.25459600021353,
34.7054823993057));
#27947=CARTESIAN_POINT('Ctrl Pts',(1.26822332534423,-2.19881071935727,34.8326383967224));
#27948=CARTESIAN_POINT('Ctrl Pts',(2.5332257643645,-0.119576086335227,34.9598118895592));
#27949=CARTESIAN_POINT('Ctrl Pts',(1.82857489987461,1.33019694560863,35.0446000499235));
#27950=CARTESIAN_POINT('Ctrl Pts',(1.24723521034521,1.7455490827215,35.0870028778158));
#27951=CARTESIAN_POINT('Ctrl Pts',(-1.00847443860881,2.06659004214475,4.91281124221424));
#27952=CARTESIAN_POINT('Ctrl Pts',(-1.69656210016283,1.73082269218899,4.955204336794));
#27953=CARTESIAN_POINT('Ctrl Pts',(-2.6988437297629,0.323810131804284,5.03998276384599));
#27954=CARTESIAN_POINT('Ctrl Pts',(-1.73146397008341,-2.09869526980756,
5.16714652337023));
#27955=CARTESIAN_POINT('Ctrl Pts',(0.826212239389695,-2.58953745539779,
5.29430252078697));
#27956=CARTESIAN_POINT('Ctrl Pts',(2.62492621405411,-0.708640864559765,
5.4214585182037));
#27957=CARTESIAN_POINT('Ctrl Pts',(2.01673606698341,1.82392913404815,5.54861451562044));
#27958=CARTESIAN_POINT('Ctrl Pts',(-0.441479376849763,2.68273202950749,
5.67577051303717));
#27959=CARTESIAN_POINT('Ctrl Pts',(-2.49461115350241,1.08146977860786,5.80292651045392));
#27960=CARTESIAN_POINT('Ctrl Pts',(-2.25983344464387,-1.51193903825939,
5.93008250787064));
#27961=CARTESIAN_POINT('Ctrl Pts',(0.0476565097918634,-2.71850306718649,
6.05723850528739));
#27962=CARTESIAN_POINT('Ctrl Pts',(2.3114126270054,-1.43178873916808,6.18439450270412));
#27963=CARTESIAN_POINT('Ctrl Pts',(2.45520865224759,1.16816409124554,6.31155050012086));
#27964=CARTESIAN_POINT('Ctrl Pts',(0.347138756504326,2.69668572115485,6.4387064975376));
#27965=CARTESIAN_POINT('Ctrl Pts',(-2.07931505948866,1.7518809460953,6.56586249495433));
#27966=CARTESIAN_POINT('Ctrl Pts',(-2.59867221540777,-0.799712689664839,
6.69301849237107));
#27967=CARTESIAN_POINT('Ctrl Pts',(-0.734587816495842,-2.61782608552589,
6.8201744897878));
#27968=CARTESIAN_POINT('Ctrl Pts',(1.80324261498706,-2.0349328401808,6.94733048720455));
#27969=CARTESIAN_POINT('Ctrl Pts',(2.68718191060275,0.414353337739565,7.07448648462127));
#27970=CARTESIAN_POINT('Ctrl Pts',(1.10650148517122,2.48360406076476,7.20164248203802));
#27971=CARTESIAN_POINT('Ctrl Pts',(-1.4890358129034,2.27495218799998,7.32879847945475));
#27972=CARTESIAN_POINT('Ctrl Pts',(-2.71886478142456,-0.0202320388555172,
7.45595447687148));
#27973=CARTESIAN_POINT('Ctrl Pts',(-1.45501537006563,-2.2968598626533,7.58311047428822));
#27974=CARTESIAN_POINT('Ctrl Pts',(1.14333965459547,-2.46686226928065,7.71026647170495));
#27975=CARTESIAN_POINT('Ctrl Pts',(2.69305064264981,-0.374317034155005,
7.8374224691217));
#27976=CARTESIAN_POINT('Ctrl Pts',(1.77275938455494,2.06154290790546,7.96457846653843));
#27977=CARTESIAN_POINT('Ctrl Pts',(-0.773464777704037,2.60660454304561,
8.09173446395516));
#27978=CARTESIAN_POINT('Ctrl Pts',(-2.61028537228249,0.760950247106553,
8.21889046137189));
#27979=CARTESIAN_POINT('Ctrl Pts',(-2.0530140682327,-1.78262958518165,8.34604645878863));
#27980=CARTESIAN_POINT('Ctrl Pts',(0.387233097108164,-2.69122379823399,
8.47320245620537));
#27981=CARTESIAN_POINT('Ctrl Pts',(2.47231924057473,-1.13149130613901,8.60035845362211));
#27982=CARTESIAN_POINT('Ctrl Pts',(2.2898527529559,1.46601820345888,8.72751445103884));
#27983=CARTESIAN_POINT('Ctrl Pts',(0.00718757362643308,2.7189305511663,
8.85467044845559));
#27984=CARTESIAN_POINT('Ctrl Pts',(-2.28206987795533,1.47810421666663,8.98182644587231));
#27985=CARTESIAN_POINT('Ctrl Pts',(-2.47826690633756,-1.11840428474922,
9.10898244328906));
#27986=CARTESIAN_POINT('Ctrl Pts',(-0.401456245579368,-2.68913887445482,
9.23613844070579));
#27987=CARTESIAN_POINT('Ctrl Pts',(2.04356057196105,-1.79345900202152,9.36329443812252));
#27988=CARTESIAN_POINT('Ctrl Pts',(2.61427205078852,0.747138974804695,9.49045043553926));
#27989=CARTESIAN_POINT('Ctrl Pts',(0.787235144338485,2.60247878583629,9.61760643295599));
#27990=CARTESIAN_POINT('Ctrl Pts',(-1.76183518460994,2.07088671478621,9.74476243037273));
#27991=CARTESIAN_POINT('Ctrl Pts',(-2.69499202523146,-0.360073585738528,
9.87191842778947));
#27992=CARTESIAN_POINT('Ctrl Pts',(-1.15636603250672,-2.4607829246142,9.9990744252062));
#27993=CARTESIAN_POINT('Ctrl Pts',(1.44285148756014,-2.30452046813505,10.126230422623));
#27994=CARTESIAN_POINT('Ctrl Pts',(2.71871980858321,-0.0346064390720735,
10.2533864200397));
#27995=CARTESIAN_POINT('Ctrl Pts',(1.50104273554987,2.2670477959807,10.3805424174564));
#27996=CARTESIAN_POINT('Ctrl Pts',(-1.0933551704636,2.48941950551298,10.5076984148732));
#27997=CARTESIAN_POINT('Ctrl Pts',(-2.68495361889042,0.428554626174045,
10.6348544122899));
#27998=CARTESIAN_POINT('Ctrl Pts',(-1.81397622242785,-2.02537040258673,
10.7620104097067));
#27999=CARTESIAN_POINT('Ctrl Pts',(0.720737186875261,-2.62167368500793,
10.8891664071234));
#28000=CARTESIAN_POINT('Ctrl Pts',(2.59440752473566,-0.813439978611172,
11.0163224045401));
#28001=CARTESIAN_POINT('Ctrl Pts',(2.08854874996522,1.74086160340985,11.1434784019569));
#28002=CARTESIAN_POINT('Ctrl Pts',(-0.332877454481621,2.69848616885575,
11.2706343993736));
#28003=CARTESIAN_POINT('Ctrl Pts',(-2.44899634451255,1.18112315520953,11.3977903967903));
#28004=CARTESIAN_POINT('Ctrl Pts',(-2.31895381119968,-1.41953803215357,
11.5249463942071));
#28005=CARTESIAN_POINT('Ctrl Pts',(-0.0620217850118915,-2.71823256940827,
11.6521023916238));
#28006=CARTESIAN_POINT('Ctrl Pts',(2.2517951529124,-1.5238285968337,11.7792583890405));
#28007=CARTESIAN_POINT('Ctrl Pts',(2.50031892815902,1.06819486082722,11.9064143864573));
#28008=CARTESIAN_POINT('Ctrl Pts',(0.455609422322499,2.68049530077911,12.033570383874));
#28009=CARTESIAN_POINT('Ctrl Pts',(-2.00697425095645,1.8343089595828,12.1607263812908));
#28010=CARTESIAN_POINT('Ctrl Pts',(-2.62880869231283,-0.694262099230915,
12.2878823787075));
#28011=CARTESIAN_POINT('Ctrl Pts',(-0.83956208520023,-2.58607240971753,
12.4150383761242));
#28012=CARTESIAN_POINT('Ctrl Pts',(1.71971097479146,-2.1059983775848,12.542194373541));
#28013=CARTESIAN_POINT('Ctrl Pts',(2.70170587365692,0.305647469244615,12.6693503709577));
#28014=CARTESIAN_POINT('Ctrl Pts',(1.20576015647079,2.43696069895998,12.7965063683744));
#28015=CARTESIAN_POINT('Ctrl Pts',(-1.39608020826688,2.33315131427293,12.9236623657912));
#28016=CARTESIAN_POINT('Ctrl Pts',(-2.71746888318096,0.0894308232722988,
13.0508183632079));
#28017=CARTESIAN_POINT('Ctrl Pts',(-1.54645948317952,-2.23631349995748,
13.1779743606246));
#28018=CARTESIAN_POINT('Ctrl Pts',(1.04292591467317,-2.51096406579447,13.3051303580414));
#28019=CARTESIAN_POINT('Ctrl Pts',(2.67576437353453,-0.482617882523345,
13.4322863554581));
#28020=CARTESIAN_POINT('Ctrl Pts',(1.854455145627,1.98837398797749,13.5594423528749));
#28021=CARTESIAN_POINT('Ctrl Pts',(-0.667716404415957,2.63567634706574,
13.6865983502916));
#28022=CARTESIAN_POINT('Ctrl Pts',(-2.5774742884714,0.865598807460369,13.8137543477083));
#28023=CARTESIAN_POINT('Ctrl Pts',(-2.12323382299999,-1.69838544979544,
13.9409103451251));
#28024=CARTESIAN_POINT('Ctrl Pts',(0.278386399345113,-2.70465081218771,
14.0680663425418));
#28025=CARTESIAN_POINT('Ctrl Pts',(2.424677211994,-1.23027453068208,14.1952223399585));
#28026=CARTESIAN_POINT('Ctrl Pts',(2.34711153345411,1.37248040158489,14.3223783373753));
#28027=CARTESIAN_POINT('Ctrl Pts',(0.116830766325856,2.71642882756896,14.449534334792));
#28028=CARTESIAN_POINT('Ctrl Pts',(-2.22060441161598,1.56893309300289,14.5766903322087));
#28029=CARTESIAN_POINT('Ctrl Pts',(-2.52135383579787,-1.01755090187926,
14.7038463296255));
#28030=CARTESIAN_POINT('Ctrl Pts',(-0.509577259988391,-2.67076131829684,
14.8310023270422));
#28031=CARTESIAN_POINT('Ctrl Pts',(1.96957150531571,-1.8744127316726,14.9581583244589));
#28032=CARTESIAN_POINT('Ctrl Pts',(2.64227595081914,0.641102802154851,15.0853143218757));
#28033=CARTESIAN_POINT('Ctrl Pts',(0.891547497430122,2.56861403543508,15.2124703192924));
#28034=CARTESIAN_POINT('Ctrl Pts',(-1.67688719724968,2.1402533333482,15.3396263167092));
#28035=CARTESIAN_POINT('Ctrl Pts',(-2.70732068494482,-0.251097017262045,
15.4667823141259));
#28036=CARTESIAN_POINT('Ctrl Pts',(-1.2546637847063,-2.41214713285786,15.5939383115426));
#28037=CARTESIAN_POINT('Ctrl Pts',(1.34874101223222,-2.36083304897461,15.7210943089594));
#28038=CARTESIAN_POINT('Ctrl Pts',(2.71511250834698,-0.144218827570166,
15.8482503063761));
#28039=CARTESIAN_POINT('Ctrl Pts',(1.59124714071456,2.20466948551834,15.9754063037928));
#28040=CARTESIAN_POINT('Ctrl Pts',(-0.992072403110452,2.53148718151893,
16.1025623012096));
#28041=CARTESIAN_POINT('Ctrl Pts',(-2.66548664388192,0.536484812921177,
16.2297182986263));
#28042=CARTESIAN_POINT('Ctrl Pts',(-1.89417968801256,-1.95056871520298,
16.356874296043));
#28043=CARTESIAN_POINT('Ctrl Pts',(0.614423999078366,-2.64860683238651,
16.4840302934598));
#28044=CARTESIAN_POINT('Ctrl Pts',(2.55949255170539,-0.917405516101003,
16.6111862908765));
#28045=CARTESIAN_POINT('Ctrl Pts',(2.15705517772773,1.6552184035486,16.7383422882933));
#28046=CARTESIAN_POINT('Ctrl Pts',(-0.223782098353677,2.70971522039944,
16.86549828571));
#28047=CARTESIAN_POINT('Ctrl Pts',(-2.39937173587358,1.27892543813116,16.9926542831267));
#28048=CARTESIAN_POINT('Ctrl Pts',(-2.3743144653421,-1.3248644545293,17.1198102805434));
#28049=CARTESIAN_POINT('Ctrl Pts',(-0.171592221611115,-2.71352005938606,
17.2469662779602));
#28050=CARTESIAN_POINT('Ctrl Pts',(2.18851034226299,-1.61339935695285,17.3741222753769));
#28051=CARTESIAN_POINT('Ctrl Pts',(2.54136307238592,0.966493009556284,17.5012782727937));
#28052=CARTESIAN_POINT('Ctrl Pts',(0.563337804795892,2.65994088672957,17.6284342702104));
#28053=CARTESIAN_POINT('Ctrl Pts',(-1.9313675502426,1.91375400432706,17.7555902676271));
#28054=CARTESIAN_POINT('Ctrl Pts',(-2.6546683479107,-0.587682708448213,
17.8827462650439));
#28055=CARTESIAN_POINT('Ctrl Pts',(-0.943170233685906,-2.55011076494666,
18.0099022624606));
#28056=CARTESIAN_POINT('Ctrl Pts',(1.6333812724308,-2.17363764737371,18.1370582598774));
#28057=CARTESIAN_POINT('Ctrl Pts',(2.71183417502487,0.196444420575375,18.2642142572941));
#28058=CARTESIAN_POINT('Ctrl Pts',(1.30305702352152,2.38635232031215,18.3913702547108));
#28059=CARTESIAN_POINT('Ctrl Pts',(-1.30085315674662,2.38755441148266,18.5185262521275));
#28060=CARTESIAN_POINT('Ctrl Pts',(-2.71165164263989,0.198948164546367,
18.6456822495443));
#28061=CARTESIAN_POINT('Ctrl Pts',(-1.63538748881455,-2.17212862525145,
18.772838246961));
#28062=CARTESIAN_POINT('Ctrl Pts',(0.940815322667484,-2.55098050401057,
18.8999942443778));
#28063=CARTESIAN_POINT('Ctrl Pts',(2.65412461084903,-0.590133504635526,
19.0271502417945));
#28064=CARTESIAN_POINT('Ctrl Pts',(1.93313368988793,1.91196996321286,19.1543062392113));
#28065=CARTESIAN_POINT('Ctrl Pts',(-0.560881649881273,2.66045988092931,
19.2814622366279));
#28066=CARTESIAN_POINT('Ctrl Pts',(-2.54046962929626,0.968839029886441,
19.4086182340448));
#28067=CARTESIAN_POINT('Ctrl Pts',(-2.18999905583186,-1.61137802475505,
19.5357742314614));
#28068=CARTESIAN_POINT('Ctrl Pts',(0.169086764197127,-2.71367733332121,
19.6629302288782));
#28069=CARTESIAN_POINT('Ctrl Pts',(2.37309021026153,-1.32705608667036,19.7900862262949));
#28070=CARTESIAN_POINT('Ctrl Pts',(2.40055154088017,1.27670956085784,19.9172422237117));
#28071=CARTESIAN_POINT('Ctrl Pts',(0.226283874248388,2.70950744812837,20.0443982211284));
#28072=CARTESIAN_POINT('Ctrl Pts',(-2.15552600052119,1.65720930008406,20.1715542185451));
#28073=CARTESIAN_POINT('Ctrl Pts',(-2.5603384982902,-0.91504195389121,20.2987102159619));
#28074=CARTESIAN_POINT('Ctrl Pts',(-0.616869187289855,-2.64803840776155,
20.4258662133786));
#28075=CARTESIAN_POINT('Ctrl Pts',(1.89237792686834,-1.95231677376124,20.5530222107954));
#28076=CARTESIAN_POINT('Ctrl Pts',(2.66598084243749,0.53402354907276,20.6801782082121));
#28077=CARTESIAN_POINT('Ctrl Pts',(0.994409294159658,2.5305701252676,20.8073342056288));
#28078=CARTESIAN_POINT('Ctrl Pts',(-1.5892108982743,2.20613773913011,20.9344902030455));
#28079=CARTESIAN_POINT('Ctrl Pts',(-2.71524450783739,-0.141711911520788,
21.0616462004623));
#28080=CARTESIAN_POINT('Ctrl Pts',(-1.35092018684815,-2.359586754492,21.188802197879));
#28081=CARTESIAN_POINT('Ctrl Pts',(1.25243612229158,-2.41330453171314,21.3159581952958));
#28082=CARTESIAN_POINT('Ctrl Pts',(2.7070876939183,-0.253596570647274,21.4431141927125));
#28083=CARTESIAN_POINT('Ctrl Pts',(1.67886257146065,2.13870415657625,21.5702701901293));
#28084=CARTESIAN_POINT('Ctrl Pts',(-0.889175524405625,2.56943610350714,
21.697426187546));
#28085=CARTESIAN_POINT('Ctrl Pts',(-2.64168289644022,0.643542133712422,
21.8245821849627));
#28086=CARTESIAN_POINT('Ctrl Pts',(-1.97130130500755,-1.87259343373928,
21.9517381823794));
#28087=CARTESIAN_POINT('Ctrl Pts',(0.507111137519175,-2.67123067094775,
22.0788941797962));
#28088=CARTESIAN_POINT('Ctrl Pts',(2.52041325965044,-1.01987842598331,22.2060501772129));
#28089=CARTESIAN_POINT('Ctrl Pts',(2.22205205594777,1.56688214740811,22.3332061746296));
#28090=CARTESIAN_POINT('Ctrl Pts',(-0.114322646597065,2.71653553919013,
22.4603621720464));
#28091=CARTESIAN_POINT('Ctrl Pts',(-2.34584332631891,1.37464689705138,22.5875181694631));
#28092=CARTESIAN_POINT('Ctrl Pts',(-2.42581208698928,-1.22803530968155,
22.7146741668798));
#28093=CARTESIAN_POINT('Ctrl Pts',(-0.28088347601373,-2.70439262610117,
22.8418301642966));
#28094=CARTESIAN_POINT('Ctrl Pts',(2.12166480421549,-1.7003451007843,22.9689861617133));
#28095=CARTESIAN_POINT('Ctrl Pts',(2.57827239442557,0.863218664853252,23.0961421591301));
#28096=CARTESIAN_POINT('Ctrl Pts',(0.670149631237062,2.63505872324713,23.2232981565468));
#28097=CARTESIAN_POINT('Ctrl Pts',(-1.85261849592907,1.99008535288051,23.3504541539635));
#28098=CARTESIAN_POINT('Ctrl Pts',(-2.67620883254712,-0.480147152240573,
23.4776101513803));
#28099=CARTESIAN_POINT('Ctrl Pts',(-1.04524383512044,-2.5100000654085,23.604766148797));
#28100=CARTESIAN_POINT('Ctrl Pts',(1.54439404301351,-2.23774038778235,23.7319221462137));
#28101=CARTESIAN_POINT('Ctrl Pts',(2.71755029608022,0.0869217549424415,
23.8590781436305));
#28102=CARTESIAN_POINT('Ctrl Pts',(1.3982338042491,2.33186132346309,23.9862341410472));
#28103=CARTESIAN_POINT('Ctrl Pts',(-1.20350960461554,2.43807293467732,24.113390138464));
#28104=CARTESIAN_POINT('Ctrl Pts',(-2.70142251876817,0.30814181524129,24.2405461358807));
#28105=CARTESIAN_POINT('Ctrl Pts',(-1.72165470325966,-2.10440967635864,
24.3677021332974));
#28106=CARTESIAN_POINT('Ctrl Pts',(0.837174015073502,-2.58684647238557,
24.4948581307141));
#28107=CARTESIAN_POINT('Ctrl Pts',(2.62816656186749,-0.696688973853852,
24.6220141281309));
#28108=CARTESIAN_POINT('Ctrl Pts',(2.00866700702307,1.83245514490942,24.7491701255476));
#28109=CARTESIAN_POINT('Ctrl Pts',(-0.453134335501955,2.68091482095145,
24.8763261229644));
#28110=CARTESIAN_POINT('Ctrl Pts',(-2.49933160157433,1.07050294188287,25.0034821203811));
#28111=CARTESIAN_POINT('Ctrl Pts',(-2.25320113911441,-1.52174887215384,
25.1306381177978));
#28112=CARTESIAN_POINT('Ctrl Pts',(0.0595120232557837,-2.71828867530585,
25.2577941152146));
#28113=CARTESIAN_POINT('Ctrl Pts',(2.31764216790862,-1.42167850962861,25.3849501126313));
#28114=CARTESIAN_POINT('Ctrl Pts',(2.45008582783643,1.17886150138301,25.512106110048));
#28115=CARTESIAN_POINT('Ctrl Pts',(0.335368816128816,2.69817767398226,25.6392621074648));
#28116=CARTESIAN_POINT('Ctrl Pts',(-2.08694052786993,1.7427892116782,25.7664181048815));
#28117=CARTESIAN_POINT('Ctrl Pts',(-2.59515746539462,-0.81104422383404,
25.8935741022983));
#28118=CARTESIAN_POINT('Ctrl Pts',(-0.723157462484335,-2.62100711324124,
26.020730099715));
#28119=CARTESIAN_POINT('Ctrl Pts',(1.81210543131392,-2.02704437766185,26.1478860971317));
#28120=CARTESIAN_POINT('Ctrl Pts',(2.68534815755687,0.426075434534669,26.2750420945485));
#28121=CARTESIAN_POINT('Ctrl Pts',(1.09565317739333,2.48840895314172,26.4021980919652));
#28122=CARTESIAN_POINT('Ctrl Pts',(-1.49894893786632,2.26843273756957,26.5293540893819));
#28123=CARTESIAN_POINT('Ctrl Pts',(-2.71875060177305,-0.0320962391350563,
26.6565100867987));
#28124=CARTESIAN_POINT('Ctrl Pts',(-1.44497862883923,-2.30318730575823,
26.7836660842154));
#28125=CARTESIAN_POINT('Ctrl Pts',(1.15409350672138,-2.46184954474304,26.9108220816321));
#28126=CARTESIAN_POINT('Ctrl Pts',(2.6946584217475,-0.36256170966231,27.0379780790489));
#28127=CARTESIAN_POINT('Ctrl Pts',(1.76374647663869,2.06925913537976,27.1651340764656));
#28128=CARTESIAN_POINT('Ctrl Pts',(-0.784831948561556,2.60320452821615,
27.2922900738823));
#28129=CARTESIAN_POINT('Ctrl Pts',(-2.61358110549165,0.749552405255957,
27.4194460712991));
#28130=CARTESIAN_POINT('Ctrl Pts',(-2.04521559579937,-1.79157142472941,
27.5466020687158));
#28131=CARTESIAN_POINT('Ctrl Pts',(0.398973201256793,-2.68950839148846,
27.6737580661326));
#28132=CARTESIAN_POINT('Ctrl Pts',(2.47723323095525,-1.12069198384702,27.8009140635493));
#28133=CARTESIAN_POINT('Ctrl Pts',(2.28343363407859,1.47599655892775,27.928070060966));
#28134=CARTESIAN_POINT('Ctrl Pts',(-0.00467719079377135,2.71893602850347,
28.0552260583828));
#28135=CARTESIAN_POINT('Ctrl Pts',(-2.28849820708635,1.46813179223479,28.1823820557995));
#28136=CARTESIAN_POINT('Ctrl Pts',(-2.47336288901496,-1.12920813956133,
28.3095380532162));
#28137=CARTESIAN_POINT('Ctrl Pts',(-0.389717730296424,-2.69086511997546,
28.436694050633));
#28138=CARTESIAN_POINT('Ctrl Pts',(2.05136729710396,-1.78452436676565,28.5638500480497));
#28139=CARTESIAN_POINT('Ctrl Pts',(2.61098684245559,0.758539855071413,28.6910060454665));
#28140=CARTESIAN_POINT('Ctrl Pts',(0.775871117775893,2.60588929385136,28.8181620428832));
#28141=CARTESIAN_POINT('Ctrl Pts',(-1.77085521348547,2.06317881340403,28.9453180403));
#28142=CARTESIAN_POINT('Ctrl Pts',(-2.69339509964618,-0.371830391993313,
29.0724740377166));
#28143=CARTESIAN_POINT('Ctrl Pts',(-1.14561681477155,-2.46580557159737,
29.1996300351334));
#28144=CARTESIAN_POINT('Ctrl Pts',(1.4528940696187,-2.29820230303488,29.3267860325501));
#28145=CARTESIAN_POINT('Ctrl Pts',(2.718844936639,-0.0227423332226366,29.4539420299669));
#28146=CARTESIAN_POINT('Ctrl Pts',(1.49113564511475,2.2735763657894,29.5810980273836));
#28147=CARTESIAN_POINT('Ctrl Pts',(-1.10420793077029,2.48462468973324,29.7082540248003));
#28148=CARTESIAN_POINT('Ctrl Pts',(-2.68679815444885,0.416834116235907,
29.8354100222171));
#28149=CARTESIAN_POINT('Ctrl Pts',(-1.80512076892626,-2.03326683266092,
29.9625660196338));
#28150=CARTESIAN_POINT('Ctrl Pts',(0.732170617296673,-2.6185036166436,30.0897220170505));
#28151=CARTESIAN_POINT('Ctrl Pts',(2.59793246058555,-0.802110923403799,
30.2168780144673));
#28152=CARTESIAN_POINT('Ctrl Pts',(2.08093220359809,1.74995890444202,30.344034011884));
#28153=CARTESIAN_POINT('Ctrl Pts',(-0.344649767196044,2.69700788674807,
30.4711900093008));
#28154=CARTESIAN_POINT('Ctrl Pts',(-2.45412713727274,1.17042513528533,30.5983460067174));
#28155=CARTESIAN_POINT('Ctrl Pts',(-2.31273724244973,-1.42964381948506,
30.7255020041343));
#28156=CARTESIAN_POINT('Ctrl Pts',(-0.0501595443200041,-2.71847733544578,
30.8526580015509));
#28157=CARTESIAN_POINT('Ctrl Pts',(2.25842329943333,-1.51398784795982,30.9798139989677));
#28158=CARTESIAN_POINT('Ctrl Pts',(2.49563380156246,1.07909542288794,31.1069699963845));
#28159=CARTESIAN_POINT('Ctrl Pts',(0.443908109713979,2.68245793879611,31.2341259938011));
#28160=CARTESIAN_POINT('Ctrl Pts',(-2.01495958288181,1.8255335884188,31.361281991218));
#28161=CARTESIAN_POINT('Ctrl Pts',(-2.6257540863254,-0.705726916965534,
31.4884379886346));
#28162=CARTESIAN_POINT('Ctrl Pts',(-0.828269153507524,-2.58971141500841,
31.6155939860514));
#28163=CARTESIAN_POINT('Ctrl Pts',(1.72888462274292,-2.09847396066029,31.7427499834681));
#28164=CARTESIAN_POINT('Ctrl Pts',(2.70034638543151,0.317434090813201,31.8699059808848));
#28165=CARTESIAN_POINT('Ctrl Pts',(1.19511442223928,2.4421991163561,31.9970619783016));
#28166=CARTESIAN_POINT('Ctrl Pts',(-1.40624817287752,2.3270369728351,32.1242179757183));
#28167=CARTESIAN_POINT('Ctrl Pts',(-2.71783326273588,0.0775716565606125,
32.251373973135));
#28168=CARTESIAN_POINT('Ctrl Pts',(-1.53668607586383,-2.24304055371657,
32.3785299705518));
#28169=CARTESIAN_POINT('Ctrl Pts',(1.05387316833121,-2.50638909606359,32.5056859679685));
#28170=CARTESIAN_POINT('Ctrl Pts',(2.67784491737894,-0.470936974057936,
32.6328419653853));
#28171=CARTESIAN_POINT('Ctrl Pts',(1.84576074359989,1.99644744162733,32.7599979628019));
#28172=CARTESIAN_POINT('Ctrl Pts',(-0.679211432678792,2.63273745311828,
32.8871539602188));
#28173=CARTESIAN_POINT('Ctrl Pts',(-2.5812270137068,0.854343264078797,33.0143099576354));
#28174=CARTESIAN_POINT('Ctrl Pts',(-2.11580226149321,-1.70763473342862,
33.1414659550522));
#28175=CARTESIAN_POINT('Ctrl Pts',(0.290186056189786,-2.70340983333955,
33.2686219524689));
#28176=CARTESIAN_POINT('Ctrl Pts',(2.43002286401826,-1.21968297089525,33.3957779498857));
#28177=CARTESIAN_POINT('Ctrl Pts',(2.34109976899834,1.38271104627974,33.5229339473025));
#28178=CARTESIAN_POINT('Ctrl Pts',(0.10497639860856,2.71690985324928,33.6500899447191));
#28179=CARTESIAN_POINT('Ctrl Pts',(-2.22743067787563,1.55923360834914,33.777245942136));
#28180=CARTESIAN_POINT('Ctrl Pts',(-2.51688760174644,-1.02855438653656,
33.9044019395525));
#28181=CARTESIAN_POINT('Ctrl Pts',(-0.497921540466094,-2.67293924524441,
34.0315579369694));
#28182=CARTESIAN_POINT('Ctrl Pts',(1.97773911754471,-1.86583890941239,34.158713934386));
#28183=CARTESIAN_POINT('Ctrl Pts',(2.6394399920918,0.652700710408037,34.2858699318029));
#28184=CARTESIAN_POINT('Ctrl Pts',(0.88035541786161,2.57233930898914,34.4130259292195));
#28185=CARTESIAN_POINT('Ctrl Pts',(-1.6862587097392,2.13318386777371,34.5401819266363));
#28186=CARTESIAN_POINT('Ctrl Pts',(-2.70610771640309,-0.263420825630993,
34.667337924053));
#28187=CARTESIAN_POINT('Ctrl Pts',(-1.24430022082504,-2.41661909656449,
34.7944939214698));
#28188=CARTESIAN_POINT('Ctrl Pts',(1.35936225667267,-2.35682489174383,34.9216499188865));
#28189=CARTESIAN_POINT('Ctrl Pts',(2.71527216294739,-0.128169239057751,
35.0488234117232));
#28190=CARTESIAN_POINT('Ctrl Pts',(1.95998264084422,1.42578951645669,35.1336115720876));
#28191=CARTESIAN_POINT('Ctrl Pts',(1.3368658628607,1.87099030021161,35.1760143999799));
#28192=CARTESIAN_POINT('Ctrl Pts',(-1.07608796999509,2.20514531467084,5.00182276437832));
#28193=CARTESIAN_POINT('Ctrl Pts',(-1.81030871625589,1.84686632199456,5.04421585895808));
#28194=CARTESIAN_POINT('Ctrl Pts',(-2.87978867813524,0.345520098533912,
5.12899428601007));
#28195=CARTESIAN_POINT('Ctrl Pts',(-1.84755059459602,-2.23940304886746,
5.25615804553432));
#28196=CARTESIAN_POINT('Ctrl Pts',(0.881605936087441,-2.76315392529851,
5.38331404295105));
#28197=CARTESIAN_POINT('Ctrl Pts',(2.80091533600486,-0.756151946153,5.51047004036779));
#28198=CARTESIAN_POINT('Ctrl Pts',(2.15194886181718,1.94621511872954,5.63762603778452));
#28199=CARTESIAN_POINT('Ctrl Pts',(-0.471078520427701,2.86259676314238,
5.76478203520127));
#28200=CARTESIAN_POINT('Ctrl Pts',(-2.66186325535688,1.15397730881358,5.89193803261799));
#28201=CARTESIAN_POINT('Ctrl Pts',(-2.41134479058127,-1.61330753477629,
6.01909403003473));
#28202=CARTESIAN_POINT('Ctrl Pts',(0.0508516576283012,-2.90076608290592,
6.14625002745147));
#28203=CARTESIAN_POINT('Ctrl Pts',(2.46638211777227,-1.52778353006007,6.2734060248682));
#28204=CARTESIAN_POINT('Ctrl Pts',(2.61981899923616,1.24648407281762,6.40056202228494));
#28205=CARTESIAN_POINT('Ctrl Pts',(0.370412799265996,2.87748598506404,6.52771801970167));
#28206=CARTESIAN_POINT('Ctrl Pts',(-2.21872348537856,1.86933643410663,6.65487401711841));
#28207=CARTESIAN_POINT('Ctrl Pts',(-2.77290112857825,-0.853329714521984,
6.78203001453515));
#28208=CARTESIAN_POINT('Ctrl Pts',(-0.783838520812214,-2.79333917680625,
6.90918601195188));
#28209=CARTESIAN_POINT('Ctrl Pts',(1.92414166455907,-2.17136564421719,7.03634200936862));
#28210=CARTESIAN_POINT('Ctrl Pts',(2.86734498811586,0.442133806270777,7.16349800678535));
#28211=CARTESIAN_POINT('Ctrl Pts',(1.18068727514493,2.65011818812846,7.29065400420209));
#28212=CARTESIAN_POINT('Ctrl Pts',(-1.58886875444023,2.42747717552242,7.41781000161883));
#28213=CARTESIAN_POINT('Ctrl Pts',(-2.90115204840517,-0.0215885031761271,
7.54496599903556));
#28214=CARTESIAN_POINT('Ctrl Pts',(-1.55256739877849,-2.45085365810098,
7.6721219964523));
#28215=CARTESIAN_POINT('Ctrl Pts',(1.21999527288542,-2.63225393721386,7.79927799386903));
#28216=CARTESIAN_POINT('Ctrl Pts',(2.87360719141344,-0.399413254315134,
7.92643399128578));
#28217=CARTESIAN_POINT('Ctrl Pts',(1.89161467498072,2.19975979350155,8.0535899887025));
#28218=CARTESIAN_POINT('Ctrl Pts',(-0.825322001864961,2.78136528197505,
8.18074598611925));
#28219=CARTESIAN_POINT('Ctrl Pts',(-2.78529289373178,0.811968430063206,
8.30790198353598));
#28220=CARTESIAN_POINT('Ctrl Pts',(-2.19065913470589,-1.90214662675786,
8.43505798095271));
#28221=CARTESIAN_POINT('Ctrl Pts',(0.413195279353741,-2.87165786555681,
8.56221397836945));
#28222=CARTESIAN_POINT('Ctrl Pts',(2.63807677311075,-1.20735254764592,8.6893699757862));
#28223=CARTESIAN_POINT('Ctrl Pts',(2.44337675421409,1.56430792109332,8.81652597320291));
#28224=CARTESIAN_POINT('Ctrl Pts',(0.0076694670848323,2.90122222770289,
8.94368197061967));
#28225=CARTESIAN_POINT('Ctrl Pts',(-2.43507207356043,1.57720424540266,9.07083796803638));
#28226=CARTESIAN_POINT('Ctrl Pts',(-2.64442320226339,-1.19338810220102,
9.19799396545314));
#28227=CARTESIAN_POINT('Ctrl Pts',(-0.428372023928768,-2.86943315731314,
9.32514996286987));
#28228=CARTESIAN_POINT('Ctrl Pts',(2.18057182537728,-1.91370210574398,9.4523059602866));
#28229=CARTESIAN_POINT('Ctrl Pts',(2.78954686053182,0.797231176043415,9.57946195770334));
#28230=CARTESIAN_POINT('Ctrl Pts',(0.840015607682165,2.77696291189002,9.70661795512008));
#28231=CARTESIAN_POINT('Ctrl Pts',(-1.87995805812211,2.20973005927462,9.83377395253681));
#28232=CARTESIAN_POINT('Ctrl Pts',(-2.87567873468839,-0.384214848777708,
9.96092994995354));
#28233=CARTESIAN_POINT('Ctrl Pts',(-1.23389500898796,-2.62576700069816,
10.0880859473702));
#28234=CARTESIAN_POINT('Ctrl Pts',(1.53958798439635,-2.45902787163197,10.2152419447871));
#28235=CARTESIAN_POINT('Ctrl Pts',(2.90099735580753,-0.0369266402241637,
10.3423979422037));
#28236=CARTESIAN_POINT('Ctrl Pts',(1.60168068553317,2.41904283069784,10.4695539396205));
#28237=CARTESIAN_POINT('Ctrl Pts',(-1.1666595610404,2.65632353146103,10.5967099370373));
#28238=CARTESIAN_POINT('Ctrl Pts',(-2.8649672997844,0.457287225195054,10.723865934454));
#28239=CARTESIAN_POINT('Ctrl Pts',(-1.93559491057049,-2.16116208955603,
10.8510219318708));
#28240=CARTESIAN_POINT('Ctrl Pts',(0.769059270748106,-2.79744473997913,
10.9781779292875));
#28241=CARTESIAN_POINT('Ctrl Pts',(2.76835051018645,-0.867977354491986,
11.1053339267041));
#28242=CARTESIAN_POINT('Ctrl Pts',(2.22857625195351,1.85757829562831,11.2324899241209));
#28243=CARTESIAN_POINT('Ctrl Pts',(-0.355195343120889,2.87940714442847,
11.3596459215376));
#28244=CARTESIAN_POINT('Ctrl Pts',(-2.61319018509511,1.26031198188509,11.4868019189544));
#28245=CARTESIAN_POINT('Ctrl Pts',(-2.47442890337263,-1.51471146998848,
11.6139579163712));
#28246=CARTESIAN_POINT('Ctrl Pts',(-0.0661800578911379,-2.9004774495069,
11.7411139137879));
#28247=CARTESIAN_POINT('Ctrl Pts',(2.40276756869014,-1.62599423308062,11.8682699112045));
#28248=CARTESIAN_POINT('Ctrl Pts',(2.66795370981783,1.13981236939675,11.9954259086213));
#28249=CARTESIAN_POINT('Ctrl Pts',(0.486155919880249,2.8602100721321,12.1225819060381));
#28250=CARTESIAN_POINT('Ctrl Pts',(-2.1415325613244,1.95729086339969,12.2497379034547));
#28251=CARTESIAN_POINT('Ctrl Pts',(-2.80505811641455,-0.740809151332146,
12.3768939008716));
#28252=CARTESIAN_POINT('Ctrl Pts',(-0.895850827110875,-2.75945656438461,
12.5040498982883));
#28253=CARTESIAN_POINT('Ctrl Pts',(1.83500961550839,-2.24719579613177,12.6312058957051));
#28254=CARTESIAN_POINT('Ctrl Pts',(2.88284271549586,0.326139713731703,12.7583618931217));
#28255=CARTESIAN_POINT('Ctrl Pts',(1.28660077975543,2.60034760535842,12.8855178905385));
#28256=CARTESIAN_POINT('Ctrl Pts',(-1.48968090786382,2.48957828314488,13.0126738879553));
#28257=CARTESIAN_POINT('Ctrl Pts',(-2.89966256166186,0.095426744978067,
13.139829885372));
#28258=CARTESIAN_POINT('Ctrl Pts',(-1.65014241533962,-2.38624794274561,
13.2669858827887));
#28259=CARTESIAN_POINT('Ctrl Pts',(1.11284925766102,-2.67931255453407,13.3941418802055));
#28260=CARTESIAN_POINT('Ctrl Pts',(2.85516195816916,-0.514975172007566,
13.5212978776221));
#28261=CARTESIAN_POINT('Ctrl Pts',(1.97878775773184,2.12168523702531,13.6484538750389));
#28262=CARTESIAN_POINT('Ctrl Pts',(-0.712483690862428,2.81238621554999,
13.7756098724557));
#28263=CARTESIAN_POINT('Ctrl Pts',(-2.75028197900763,0.923633190777811,
13.9027658698724));
#28264=CARTESIAN_POINT('Ctrl Pts',(-2.26558679818273,-1.81225431302031,
14.0299218672892));
#28265=CARTESIAN_POINT('Ctrl Pts',(0.297050915597647,-2.88598509848946,
14.1570778647059));
#28266=CARTESIAN_POINT('Ctrl Pts',(2.58724056759163,-1.31275872900115,14.2842338621225));
#28267=CARTESIAN_POINT('Ctrl Pts',(2.50447447024121,1.46449884365629,14.4113898595393));
#28268=CARTESIAN_POINT('Ctrl Pts',(0.124663727066729,2.89855277514735,14.538545856956));
#28269=CARTESIAN_POINT('Ctrl Pts',(-2.36948563292723,1.67412277641516,14.6657018543728));
#28270=CARTESIAN_POINT('Ctrl Pts',(-2.69039891040353,-1.08577296800945,
14.7928578517896));
#28271=CARTESIAN_POINT('Ctrl Pts',(-0.54374205062941,-2.84982347129394,
14.9200138492063));
#28272=CARTESIAN_POINT('Ctrl Pts',(2.10162213515206,-2.00008340731066,15.0471698466229));
#28273=CARTESIAN_POINT('Ctrl Pts',(2.81942829211027,0.684085770067413,15.1743258440397));
#28274=CARTESIAN_POINT('Ctrl Pts',(0.951321619997796,2.74082768712031,15.3014818414565));
#28275=CARTESIAN_POINT('Ctrl Pts',(-1.7893147024018,2.28374738772249,15.4286378388731));
#28276=CARTESIAN_POINT('Ctrl Pts',(-2.88883397382565,-0.267931907079493,
15.55579383629));
#28277=CARTESIAN_POINT('Ctrl Pts',(-1.33878316933185,-2.57387040479398,
15.6829498337066));
#28278=CARTESIAN_POINT('Ctrl Pts',(1.43916783840774,-2.51911594970405,15.8101058311235));
#28279=CARTESIAN_POINT('Ctrl Pts',(2.89714820282978,-0.153888030725978,
15.9372618285401));
#28280=CARTESIAN_POINT('Ctrl Pts',(1.69793287747983,2.35248234397915,16.0644178259569));
#28281=CARTESIAN_POINT('Ctrl Pts',(-1.05858625412856,2.70121164993243,16.1915738233737));
#28282=CARTESIAN_POINT('Ctrl Pts',(-2.84419515443609,0.572453630124593,
16.3187298207904));
#28283=CARTESIAN_POINT('Ctrl Pts',(-2.02117564634667,-2.08134529614278,
16.4458858182071));
#28284=CARTESIAN_POINT('Ctrl Pts',(0.655618277044906,-2.82618362990893,
16.5730418156239));
#28285=CARTESIAN_POINT('Ctrl Pts',(2.73109465023388,-0.978913298829069,
16.7001978130405));
#28286=CARTESIAN_POINT('Ctrl Pts',(2.30167571780043,1.76619311663488,16.8273538104573));
#28287=CARTESIAN_POINT('Ctrl Pts',(-0.23878564961041,2.89138905177091,16.9545098078741));
#28288=CARTESIAN_POINT('Ctrl Pts',(-2.56023847672482,1.36467145403512,17.0816658052908));
#28289=CARTESIAN_POINT('Ctrl Pts',(-2.53350123247984,-1.41369046830757,
17.2088218027076));
#28290=CARTESIAN_POINT('Ctrl Pts',(-0.183096683813934,-2.89544898755562,
17.3359778001242));
#28291=CARTESIAN_POINT('Ctrl Pts',(2.33523980515338,-1.72157029702181,17.4631337975409));
#28292=CARTESIAN_POINT('Ctrl Pts',(2.71174967345399,1.03129188093514,17.5902897949577));
#28293=CARTESIAN_POINT('Ctrl Pts',(0.601106990495946,2.8382775800012,17.7174457923745));
#28294=CARTESIAN_POINT('Ctrl Pts',(-2.06085678217284,2.04206232973746,17.8446017897912));
#28295=CARTESIAN_POINT('Ctrl Pts',(-2.83265154192117,-0.627084106968225,
17.971757787208));
#28296=CARTESIAN_POINT('Ctrl Pts',(-1.0064054211695,-2.72108385820819,18.0989137846246));
#28297=CARTESIAN_POINT('Ctrl Pts',(1.74289190720861,-2.31936996508692,18.2260697820413));
#28298=CARTESIAN_POINT('Ctrl Pts',(2.89365007247118,0.209615107394771,18.3532257794581));
#28299=CARTESIAN_POINT('Ctrl Pts',(1.39042095024577,2.54634616976526,18.4803817768749));
#28300=CARTESIAN_POINT('Ctrl Pts',(-1.38806932443051,2.54762885557052,18.6075377742917));
#28301=CARTESIAN_POINT('Ctrl Pts',(-2.89345530213681,0.212286715780541,
18.7346937717084));
#28302=CARTESIAN_POINT('Ctrl Pts',(-1.74503263109116,-2.31775977003389,
18.861849769125));
#28303=CARTESIAN_POINT('Ctrl Pts',(1.00389262429512,-2.72201190924037,18.9890057665418));
#28304=CARTESIAN_POINT('Ctrl Pts',(2.8320713498127,-0.629699217667123,19.1161617639586));
#28305=CARTESIAN_POINT('Ctrl Pts',(2.06274133328574,2.04015867694529,19.2433177613753));
#28306=CARTESIAN_POINT('Ctrl Pts',(-0.598486161791943,2.83883137035367,
19.370473758792));
#28307=CARTESIAN_POINT('Ctrl Pts',(-2.71079632915113,1.03379519104186,19.4976297562087));
#28308=CARTESIAN_POINT('Ctrl Pts',(-2.33682833005875,-1.71941344388002,
19.6247857536255));
#28309=CARTESIAN_POINT('Ctrl Pts',(0.180423247106767,-2.89561680597831,
19.7519417510422));
#28310=CARTESIAN_POINT('Ctrl Pts',(2.53219489677721,-1.41602903921353,19.8790977484589));
#28311=CARTESIAN_POINT('Ctrl Pts',(2.56149738218228,1.36230701247328,20.0062537458757));
#28312=CARTESIAN_POINT('Ctrl Pts',(0.241455157969516,2.89116734933321,20.1334097432925));
#28313=CARTESIAN_POINT('Ctrl Pts',(-2.30004401635826,1.76831749354441,20.2605657407091));
#28314=CARTESIAN_POINT('Ctrl Pts',(-2.73199731361163,-0.976391270741076,
20.387721738126));
#28315=CARTESIAN_POINT('Ctrl Pts',(-0.658227403779219,-2.82557709505061,
20.5148777355426));
#28316=CARTESIAN_POINT('Ctrl Pts',(2.01925308547869,-2.0832105539156,20.6420337329593));
#28317=CARTESIAN_POINT('Ctrl Pts',(2.84472248671151,0.569827349956488,20.769189730376));
#28318=CARTESIAN_POINT('Ctrl Pts',(1.06107982287839,2.70023310931498,20.8963457277929));
#28319=CARTESIAN_POINT('Ctrl Pts',(-1.69576011443302,2.35404903718225,21.0235017252096));
#28320=CARTESIAN_POINT('Ctrl Pts',(-2.89728905227348,-0.151213037588684,
21.1506577226264));
#28321=CARTESIAN_POINT('Ctrl Pts',(-1.44149311656933,-2.51778609695974,
21.2778137200429));
#28322=CARTESIAN_POINT('Ctrl Pts',(1.33640615248957,-2.57510540187165,21.4049697174598));
#28323=CARTESIAN_POINT('Ctrl Pts',(2.88858536183199,-0.270599043920174,
21.5321257148764));
#28324=CARTESIAN_POINT('Ctrl Pts',(1.791422516287,2.28209434583684,21.6592817122933));
#28325=CARTESIAN_POINT('Ctrl Pts',(-0.948790617189007,2.74170487104185,
21.7864377097099));
#28326=CARTESIAN_POINT('Ctrl Pts',(-2.81879547618728,0.686688647486343,
21.9135937071268));
#28327=CARTESIAN_POINT('Ctrl Pts',(-2.10346790988621,-1.99814213389326,
22.0407497045435));
#28328=CARTESIAN_POINT('Ctrl Pts',(0.541110586092526,-2.85032429186209,
22.1679057019603));
#28329=CARTESIAN_POINT('Ctrl Pts',(2.6893952729901,-1.08825654180393,22.2950616993769));
#28330=CARTESIAN_POINT('Ctrl Pts',(2.37103033509376,1.67193432443554,22.4222176967938));
#28331=CARTESIAN_POINT('Ctrl Pts',(-0.121987449548903,2.89866664128752,
22.5493736942105));
#28332=CARTESIAN_POINT('Ctrl Pts',(-2.50312123570262,1.46681059259031,22.6765296916271));
#28333=CARTESIAN_POINT('Ctrl Pts',(-2.58845153068903,-1.31036937862351,
22.8036856890438));
#28334=CARTESIAN_POINT('Ctrl Pts',(-0.299715409669359,-2.88570960222391,
22.9308416864606));
#28335=CARTESIAN_POINT('Ctrl Pts',(2.26391258396967,-1.81434534951434,23.0579976838774));
#28336=CARTESIAN_POINT('Ctrl Pts',(2.75113359426246,0.921093470653797,23.1851536812941));
#28337=CARTESIAN_POINT('Ctrl Pts',(0.715080054250639,2.81172718292039,23.3123096787109));
#28338=CARTESIAN_POINT('Ctrl Pts',(-1.97682796919452,2.12351134100359,23.4394656761275));
#28339=CARTESIAN_POINT('Ctrl Pts',(-2.85563621609605,-0.512338790724611,
23.5666216735442));
#28340=CARTESIAN_POINT('Ctrl Pts',(-1.11532258391811,-2.6782839223956,23.693777670961));
#28341=CARTESIAN_POINT('Ctrl Pts',(1.64793849699504,-2.38777049677775,23.8209336683777));
#28342=CARTESIAN_POINT('Ctrl Pts',(2.89974943291822,0.0927494552598746,
23.9480896657945));
#28343=CARTESIAN_POINT('Ctrl Pts',(1.49197889246301,2.48820180443737,24.0752456632113));
#28344=CARTESIAN_POINT('Ctrl Pts',(-1.28419933884185,2.60153441131934,24.202401660628));
#28345=CARTESIAN_POINT('Ctrl Pts',(-2.8825403629767,0.32880129405259,24.3295576580448));
#28346=CARTESIAN_POINT('Ctrl Pts',(-1.83708366195063,-2.24550057986067,
24.4567136554614));
#28347=CARTESIAN_POINT('Ctrl Pts',(0.893302647963849,-2.76028252436256,
24.5838696528783));
#28348=CARTESIAN_POINT('Ctrl Pts',(2.80437293410263,-0.74339873663678,24.7110256502948));
#28349=CARTESIAN_POINT('Ctrl Pts',(2.14333880883014,1.95531275905497,24.8381816477117));
#28350=CARTESIAN_POINT('Ctrl Pts',(-0.483514889973881,2.86065771918524,
24.9653376451283));
#28351=CARTESIAN_POINT('Ctrl Pts',(-2.66690018756726,1.14227519657666,25.0924936425451));
#28352=CARTESIAN_POINT('Ctrl Pts',(-2.40426781974259,-1.62377507251181,
25.2196496399619));
#28353=CARTESIAN_POINT('Ctrl Pts',(0.063502028255683,-2.90053731704456,
25.3468056373787));
#28354=CARTESIAN_POINT('Ctrl Pts',(2.47302932048551,-1.51699545654545,25.4739616347953));
#28355=CARTESIAN_POINT('Ctrl Pts',(2.61435271322018,1.25789869466457,25.6011176322122));
#28356=CARTESIAN_POINT('Ctrl Pts',(0.357853739005512,2.87907796640528,25.7282736296288));
#28357=CARTESIAN_POINT('Ctrl Pts',(-2.22686020602959,1.85963514108612,25.8554296270455));
#28358=CARTESIAN_POINT('Ctrl Pts',(-2.76915073088654,-0.865420975474404,
25.9825856244623));
#28359=CARTESIAN_POINT('Ctrl Pts',(-0.771641814605623,-2.79673347766867,
26.109741621879));
#28360=CARTESIAN_POINT('Ctrl Pts',(1.93359869159367,-2.16294829689196,26.2368976192958));
#28361=CARTESIAN_POINT('Ctrl Pts',(2.8653882904376,0.4546418152608,26.3640536167125));
#28362=CARTESIAN_POINT('Ctrl Pts',(1.169111638671,2.65524522624268,26.4912096141293));
#28363=CARTESIAN_POINT('Ctrl Pts',(-1.59944650843108,2.42052062619349,26.6183656115459));
#28364=CARTESIAN_POINT('Ctrl Pts',(-2.90103021353787,-0.0342481430297994,
26.7455216089627));
#28365=CARTESIAN_POINT('Ctrl Pts',(-1.54185774062733,-2.45760532690425,
26.8726776063794));
#28366=CARTESIAN_POINT('Ctrl Pts',(1.23147012089423,-2.62690513275704,26.9998336037961));
#28367=CARTESIAN_POINT('Ctrl Pts',(2.8753227646389,-0.386869789864589,27.1269896012129));
#28368=CARTESIAN_POINT('Ctrl Pts',(1.88199749341217,2.20799335822166,27.2541455986297));
#28369=CARTESIAN_POINT('Ctrl Pts',(-0.837451288780281,2.77773731192868,
27.3813015960464));
#28370=CARTESIAN_POINT('Ctrl Pts',(-2.7888095905591,0.799806415807056,27.5084575934632));
#28371=CARTESIAN_POINT('Ctrl Pts',(-2.18233781088392,-1.91168797515362,
27.6356135908798));
#28372=CARTESIAN_POINT('Ctrl Pts',(0.425722503006781,-2.86982744874917,
27.7627695882965));
#28373=CARTESIAN_POINT('Ctrl Pts',(2.64332022374341,-1.1958291809074,27.8899255857133));
#28374=CARTESIAN_POINT('Ctrl Pts',(2.43652726320332,1.57495527899285,28.0170815831301));
#28375=CARTESIAN_POINT('Ctrl Pts',(-0.00499077473252099,2.90122807227011,
28.1442375805469));
#28376=CARTESIAN_POINT('Ctrl Pts',(-2.44193139232967,1.56656321618868,28.2713935779634));
#28377=CARTESIAN_POINT('Ctrl Pts',(-2.63919039333589,-1.2049163053441,28.3985495753804));
#28378=CARTESIAN_POINT('Ctrl Pts',(-0.415846495667482,-2.87127513958548,
28.525705572797));
#28379=CARTESIAN_POINT('Ctrl Pts',(2.1889019552147,-1.90416844465447,28.6528615702139));
#28380=CARTESIAN_POINT('Ctrl Pts',(2.78604139422485,0.809396432427394,28.7800175676304));
#28381=CARTESIAN_POINT('Ctrl Pts',(0.827889675872156,2.7806020786414,28.9071735650473));
#28382=CARTESIAN_POINT('Ctrl Pts',(-1.88958283807723,2.2015053788725,29.0343295624639));
#28383=CARTESIAN_POINT('Ctrl Pts',(-2.87397474265299,-0.396759894335619,
29.1614855598808));
#28384=CARTESIAN_POINT('Ctrl Pts',(-1.22242510608428,-2.63112639285447,
29.2886415572974));
#28385=CARTESIAN_POINT('Ctrl Pts',(1.55030387498037,-2.45228610288064,29.4157975547142));
#28386=CARTESIAN_POINT('Ctrl Pts',(2.90113087311882,-0.0242671011316893,
29.5429535521309));
#28387=CARTESIAN_POINT('Ctrl Pts',(1.59110937065723,2.42600911081705,29.6701095495477));
#28388=CARTESIAN_POINT('Ctrl Pts',(-1.17823994856453,2.6512072455331,29.7972655469643));
#28389=CARTESIAN_POINT('Ctrl Pts',(-2.86693550289264,0.444780909453394,
29.924421544381));
#28390=CARTESIAN_POINT('Ctrl Pts',(-1.92614574000444,-2.16958793862411,
30.0515775417978));
#28391=CARTESIAN_POINT('Ctrl Pts',(0.781259259623611,-2.79406213324135,
30.1787335392145));
#28392=CARTESIAN_POINT('Ctrl Pts',(2.77211177662798,-0.855888738704282,
30.3058895366313));
#28393=CARTESIAN_POINT('Ctrl Pts',(2.22044905149627,1.86728552847961,30.433045534048));
#28394=CARTESIAN_POINT('Ctrl Pts',(-0.367756934774604,2.87782975036528,
30.5602015314649));
#28395=CARTESIAN_POINT('Ctrl Pts',(-2.61866497370095,1.24889670936804,30.6873575288816));
#28396=CARTESIAN_POINT('Ctrl Pts',(-2.46779554253535,-1.52549480346568,
30.8145135262982));
#28397=CARTESIAN_POINT('Ctrl Pts',(-0.0535225090063733,-2.90073862597142,
30.9416695237149));
#28398=CARTESIAN_POINT('Ctrl Pts',(2.40984010167806,-1.61549370765973,31.0688255211317));
#28399=CARTESIAN_POINT('Ctrl Pts',(2.66295446722381,1.15144376356069,31.1959815185485));
#28400=CARTESIAN_POINT('Ctrl Pts',(0.473670088560071,2.86230429592071,31.3231375159653));
#28401=CARTESIAN_POINT('Ctrl Pts',(-2.15005327270024,1.94792714432035,31.4502935133819));
#28402=CARTESIAN_POINT('Ctrl Pts',(-2.80179871327025,-0.753042631894556,
31.5774495107988));
#28403=CARTESIAN_POINT('Ctrl Pts',(-0.883800756751865,-2.76333954809381,
31.7046055082154));
#28404=CARTESIAN_POINT('Ctrl Pts',(1.84479831398562,-2.23916690196877,31.8317615056321));
#28405=CARTESIAN_POINT('Ctrl Pts',(2.8813920798935,0.338716573581852,31.9589175030488));
#28406=CARTESIAN_POINT('Ctrl Pts',(1.27524129844414,2.6059372343326,32.0860735004657));
#28407=CARTESIAN_POINT('Ctrl Pts',(-1.5005305873182,2.48305400348663,32.2132294978823));
#28408=CARTESIAN_POINT('Ctrl Pts',(-2.90005137117508,0.0827724761696081,
32.340385495299));
#28409=CARTESIAN_POINT('Ctrl Pts',(-1.6397137464159,-2.39342601424305,32.4675414927158));
#28410=CARTESIAN_POINT('Ctrl Pts',(1.12453047387723,-2.67443085431241,32.5946974901326));
#28411=CARTESIAN_POINT('Ctrl Pts',(2.85738199282378,-0.502511112833611,
32.7218534875494));
#28412=CARTESIAN_POINT('Ctrl Pts',(1.9695104363943,2.13029997827834,32.8490094849659));
#28413=CARTESIAN_POINT('Ctrl Pts',(-0.72474940742878,2.80925028240099,32.9761654823829));
#28414=CARTESIAN_POINT('Ctrl Pts',(-2.75428630705593,0.911623015442704,
33.1033214797994));
#28415=CARTESIAN_POINT('Ctrl Pts',(-2.25765698496233,-1.82212371820075,
33.2304774772162));
#28416=CARTESIAN_POINT('Ctrl Pts',(0.309641684678655,-2.88466091776816,
33.3576334746329));
#28417=CARTESIAN_POINT('Ctrl Pts',(2.59294462077817,-1.30145705427967,33.4847894720497));
#28418=CARTESIAN_POINT('Ctrl Pts',(2.49805964487565,1.47541540560368,33.6119454694664));
#28419=CARTESIAN_POINT('Ctrl Pts',(0.112014579002967,2.89906605136737,33.7391014668832));
#28420=CARTESIAN_POINT('Ctrl Pts',(-2.376769568663,1.66377298632484,33.8662574642999));
#28421=CARTESIAN_POINT('Ctrl Pts',(-2.68563323608405,-1.09751418525246,
33.9934134617166));
#28422=CARTESIAN_POINT('Ctrl Pts',(-0.531304869200315,-2.8521474181369,
34.1205694591334));
#28423=CARTESIAN_POINT('Ctrl Pts',(2.11033734788005,-1.99093475005384,34.2477254565501));
#28424=CARTESIAN_POINT('Ctrl Pts',(2.81640219551024,0.696461264250067,34.3748814539669));
#28425=CARTESIAN_POINT('Ctrl Pts',(0.939379163429915,2.74480272297943,34.5020374513837));
#28426=CARTESIAN_POINT('Ctrl Pts',(-1.79931453131619,2.27620394728637,34.6291934488004));
#28427=CARTESIAN_POINT('Ctrl Pts',(-2.88753968137186,-0.281081969612209,
34.7563494462171));
#28428=CARTESIAN_POINT('Ctrl Pts',(-1.32772477658342,-2.57864219291544,
34.8835054436339));
#28429=CARTESIAN_POINT('Ctrl Pts',(1.45050118800113,-2.5148390641304,35.0106614410506));
#28430=CARTESIAN_POINT('Ctrl Pts',(2.89731856153029,-0.136762391780276,
35.1378349338873));
#28431=CARTESIAN_POINT('Ctrl Pts',(2.09139038181383,1.52138208730474,35.2226230942517));
#28432=CARTESIAN_POINT('Ctrl Pts',(1.42649651537617,1.99643151770172,35.265025922144));
#28433=CARTESIAN_POINT('Ctrl Pts',(1.07765335145023,-2.20537355632018,35.));
#28434=CARTESIAN_POINT('Ctrl Pts',(1.12608568679243,-2.17636639516506,35.));
#28435=CARTESIAN_POINT('Ctrl Pts',(1.17334200114935,-2.14562777706368,35.));
#28436=CARTESIAN_POINT('Ctrl Pts',(1.21932057562345,-2.11315743459273,35.));
#28437=CARTESIAN_POINT('Ctrl Pts',(1.28817512261598,-2.06453194441387,35.));
#28438=CARTESIAN_POINT('Ctrl Pts',(1.35416618230553,-2.01202443036934,35.));
#28439=CARTESIAN_POINT('Ctrl Pts',(1.41715084111308,-1.95600074797492,35.));
#28440=CARTESIAN_POINT('Ctrl Pts',(1.48097822413899,-1.89922747806429,35.));
#28441=CARTESIAN_POINT('Ctrl Pts',(1.54171870905508,-1.8388423677737,35.));
#28442=CARTESIAN_POINT('Ctrl Pts',(1.59918018254526,-1.77519516634181,35.));
#28443=CARTESIAN_POINT('Ctrl Pts',(1.65050079776131,-1.71834988661151,35.));
#28444=CARTESIAN_POINT('Ctrl Pts',(1.69920540977255,-1.65890158684205,35.));
#28445=CARTESIAN_POINT('Ctrl Pts',(1.74512376077102,-1.5970884092347,35.));
#28446=CARTESIAN_POINT('Ctrl Pts',(1.75529127963222,-1.58340136177924,35.));
#28447=CARTESIAN_POINT('Ctrl Pts',(1.76532422531884,-1.56959511326082,35.));
#28448=CARTESIAN_POINT('Ctrl Pts',(1.77520514651304,-1.5556944105563,35.));
#28449=CARTESIAN_POINT('Ctrl Pts',(1.82386234832705,-1.48724236205229,35.));
#28450=CARTESIAN_POINT('Ctrl Pts',(1.86891170266444,-1.41640445602353,35.));
#28451=CARTESIAN_POINT('Ctrl Pts',(1.91020321093418,-1.34352891022868,35.));
#28452=CARTESIAN_POINT('Ctrl Pts',(1.95133765088607,-1.27093057492749,35.));
#28453=CARTESIAN_POINT('Ctrl Pts',(1.98874309755711,-1.19630906999412,35.));
#28454=CARTESIAN_POINT('Ctrl Pts',(2.02222286790158,-1.11999139492036,35.));
#28455=CARTESIAN_POINT('Ctrl Pts',(2.05486283066187,-1.04558807474436,35.));
#28456=CARTESIAN_POINT('Ctrl Pts',(2.08377169731716,-0.969571724964817,
35.0000000000001));
#28457=CARTESIAN_POINT('Ctrl Pts',(2.10871830317936,-0.892242812277137,
35.));
#28458=CARTESIAN_POINT('Ctrl Pts',(2.12038288024076,-0.856085225705955,
35.));
#28459=CARTESIAN_POINT('Ctrl Pts',(2.13118046130615,-0.819640713985427,
35.0000000000001));
#28460=CARTESIAN_POINT('Ctrl Pts',(2.14108350125101,-0.782940603525681,
35.0000000000001));
#28461=CARTESIAN_POINT('Ctrl Pts',(2.14499434205243,-0.768447246919899,
35.0000000000001));
#28462=CARTESIAN_POINT('Ctrl Pts',(2.14876589141593,-0.753912606988428,
35.));
#28463=CARTESIAN_POINT('Ctrl Pts',(2.15239164739826,-0.739358800620033,
35.));
#28464=CARTESIAN_POINT('Ctrl Pts',(2.1717999226392,-0.661453866813646,35.));
#28465=CARTESIAN_POINT('Ctrl Pts',(2.18707152189339,-0.582868815048147,
35.0000000000001));
#28466=CARTESIAN_POINT('Ctrl Pts',(2.19803328046829,-0.503902432658308,
35.));
#28467=CARTESIAN_POINT('Ctrl Pts',(2.20867776994429,-0.427221595312448,
35.));
#28468=CARTESIAN_POINT('Ctrl Pts',(2.21525829954634,-0.350180402115567,
35.));
#28469=CARTESIAN_POINT('Ctrl Pts',(2.21756806762709,-0.273055178946711,
35.));
#28470=CARTESIAN_POINT('Ctrl Pts',(2.21922188933148,-0.217832592273324,
35.));
#28471=CARTESIAN_POINT('Ctrl Pts',(2.21868522452938,-0.16256695838533,35.));
#28472=CARTESIAN_POINT('Ctrl Pts',(2.21586615289966,-0.107363829501902,
35.));
#28473=CARTESIAN_POINT('Ctrl Pts',(2.21363495647111,-0.0636724870361094,
35.));
#28474=CARTESIAN_POINT('Ctrl Pts',(2.20997361758447,-0.0200203449622079,
35.));
#28475=CARTESIAN_POINT('Ctrl Pts',(2.20490714034605,0.02353692277755,35.));
#28476=CARTESIAN_POINT('Ctrl Pts',(2.20288214372725,0.0409461236377381,
35.));
#28477=CARTESIAN_POINT('Ctrl Pts',(2.20063263637465,0.0583401394397984,
35.));
#28478=CARTESIAN_POINT('Ctrl Pts',(2.19816005299519,0.0757152900358326,
35.));
#28479=CARTESIAN_POINT('Ctrl Pts',(2.19629318131952,0.0888340292369028,
35.));
#28480=CARTESIAN_POINT('Ctrl Pts',(2.19429889864556,0.101942946564588,35.));
#28481=CARTESIAN_POINT('Ctrl Pts',(2.19218072060339,0.115023983495219,35.));
#28482=CARTESIAN_POINT('Ctrl Pts',(2.17977000031993,0.191667725018257,35.));
#28483=CARTESIAN_POINT('Ctrl Pts',(2.16309238897283,0.267488609930578,35.));
#28484=CARTESIAN_POINT('Ctrl Pts',(2.1423663045745,0.342201061127123,35.));
#28485=CARTESIAN_POINT('Ctrl Pts',(2.12141046041582,0.417741739911314,35.));
#28486=CARTESIAN_POINT('Ctrl Pts',(2.09631530446764,0.492150169822511,35.));
#28487=CARTESIAN_POINT('Ctrl Pts',(2.06725864745812,0.565108591848321,35.));
#28488=CARTESIAN_POINT('Ctrl Pts',(2.04123920834817,0.630440856975602,35.));
#28489=CARTESIAN_POINT('Ctrl Pts',(2.01204219851591,0.69461051592541,35.));
#28490=CARTESIAN_POINT('Ctrl Pts',(1.9797690575023,0.757365501062226,35.));
#28491=CARTESIAN_POINT('Ctrl Pts',(1.9659229546567,0.78428918902653,35.));
#28492=CARTESIAN_POINT('Ctrl Pts',(1.95151036732749,0.81095215532431,35.));
#28493=CARTESIAN_POINT('Ctrl Pts',(1.93653818053308,0.837332865669673,35.));
#28494=CARTESIAN_POINT('Ctrl Pts',(1.92952503385073,0.84968989766354,35.));
#28495=CARTESIAN_POINT('Ctrl Pts',(1.92238807723357,0.861986698760252,35.));
#28496=CARTESIAN_POINT('Ctrl Pts',(1.91513122016409,0.874215517168203,35.));
#28497=CARTESIAN_POINT('Ctrl Pts',(1.87607319733047,0.940033744540321,35.));
#28498=CARTESIAN_POINT('Ctrl Pts',(1.83365076636555,1.0037092427996,35.));
#28499=CARTESIAN_POINT('Ctrl Pts',(1.78802404629311,1.06493571288568,35.));
#28500=CARTESIAN_POINT('Ctrl Pts',(1.74567631435256,1.12176211063583,35.));
#28501=CARTESIAN_POINT('Ctrl Pts',(1.70056750903953,1.17647899830786,35.));
#28502=CARTESIAN_POINT('Ctrl Pts',(1.65280195923282,1.22880897718462,35.));
#28503=CARTESIAN_POINT('Ctrl Pts',(1.63720809247316,1.24589297855049,35.));
#28504=CARTESIAN_POINT('Ctrl Pts',(1.62133091608016,1.26272229886012,35.));
#28505=CARTESIAN_POINT('Ctrl Pts',(1.60517365571296,1.27928641683785,35.));
#28506=CARTESIAN_POINT('Ctrl Pts',(1.59049326620989,1.29433647471657,35.));
#28507=CARTESIAN_POINT('Ctrl Pts',(1.57557759509512,1.30917128746184,35.));
#28508=CARTESIAN_POINT('Ctrl Pts',(1.56045218899025,1.32376086026856,35.));
#28509=CARTESIAN_POINT('Ctrl Pts',(1.50795809437859,1.37439529678875,35.));
#28510=CARTESIAN_POINT('Ctrl Pts',(1.45289725142259,1.42212540384556,35.));
#28511=CARTESIAN_POINT('Ctrl Pts',(1.39539290098519,1.46665275041003,35.));
#28512=CARTESIAN_POINT('Ctrl Pts',(1.33835522673797,1.5108187355767,35.));
#28513=CARTESIAN_POINT('Ctrl Pts',(1.27891299211275,1.55183426341562,35.));
#28514=CARTESIAN_POINT('Ctrl Pts',(1.2171680440423,1.58936089781169,35.));
#28515=CARTESIAN_POINT('Ctrl Pts',(1.19843944143164,1.60074355250463,35.));
#28516=CARTESIAN_POINT('Ctrl Pts',(1.17949888147004,1.61180485329072,35.));
#28517=CARTESIAN_POINT('Ctrl Pts',(1.16034898466929,1.62253437445157,35.));
#28518=CARTESIAN_POINT('',(-1.16151515828124,-1.62372562119785,4.99906051802604));
#28519=CARTESIAN_POINT('Ctrl Pts',(-1.16285328700336,-1.62483580526419,
5.));
#28520=CARTESIAN_POINT('Ctrl Pts',(-1.20343768958331,-1.60238320695503,
5.));
#28521=CARTESIAN_POINT('Ctrl Pts',(-1.24311218157518,-1.57845987066057,
5.));
#28522=CARTESIAN_POINT('Ctrl Pts',(-1.28178686802123,-1.55308297299673,
5.));
#28523=CARTESIAN_POINT('Ctrl Pts',(-1.34195170533604,-1.51360503381216,
5.));
#28524=CARTESIAN_POINT('Ctrl Pts',(-1.39969830932625,-1.470612093931,5.));
#28525=CARTESIAN_POINT('Ctrl Pts',(-1.45494355975133,-1.42445336940955,
5.));
#28526=CARTESIAN_POINT('Ctrl Pts',(-1.48514962863777,-1.39921547833516,
5.));
#28527=CARTESIAN_POINT('Ctrl Pts',(-1.51460761679082,-1.3730302650096,5.));
#28528=CARTESIAN_POINT('Ctrl Pts',(-1.54330127771845,-1.34594885488638,
5.));
#28529=CARTESIAN_POINT('Ctrl Pts',(-1.5566354423299,-1.33336391560645,5.));
#28530=CARTESIAN_POINT('Ctrl Pts',(-1.56980451805764,-1.32058538486767,
5.));
#28531=CARTESIAN_POINT('Ctrl Pts',(-1.58280670788321,-1.30761812162911,
5.));
#28532=CARTESIAN_POINT('Ctrl Pts',(-1.59329282042784,-1.29716017696445,
5.));
#28533=CARTESIAN_POINT('Ctrl Pts',(-1.60366420748321,-1.28658560363462,
5.));
#28534=CARTESIAN_POINT('Ctrl Pts',(-1.61391823577837,-1.27589950014936,
5.));
#28535=CARTESIAN_POINT('Ctrl Pts',(-1.66537461857496,-1.22227489372994,
5.));
#28536=CARTESIAN_POINT('Ctrl Pts',(-1.71389395975769,-1.16582913622441,
5.));
#28537=CARTESIAN_POINT('Ctrl Pts',(-1.75938584450093,-1.10692270980611,
5.));
#28538=CARTESIAN_POINT('Ctrl Pts',(-1.80604256162394,-1.04650796793208,
5.));
#28539=CARTESIAN_POINT('Ctrl Pts',(-1.8495154674723,-0.983504341078151,
5.));
#28540=CARTESIAN_POINT('Ctrl Pts',(-1.88967804425422,-0.918255072861017,
5.));
#28541=CARTESIAN_POINT('Ctrl Pts',(-1.89492548324527,-0.909729933748583,
5.));
#28542=CARTESIAN_POINT('Ctrl Pts',(-1.90011636451144,-0.901166405302841,
5.));
#28543=CARTESIAN_POINT('Ctrl Pts',(-1.90525036092304,-0.89256520611988,
5.));
#28544=CARTESIAN_POINT('Ctrl Pts',(-1.91542554647779,-0.875518291657261,
5.));
#28545=CARTESIAN_POINT('Ctrl Pts',(-1.92537820160518,-0.858321342061171,
5.));
#28546=CARTESIAN_POINT('Ctrl Pts',(-1.93509056212758,-0.841008120409997,
5.));
#28547=CARTESIAN_POINT('Ctrl Pts',(-1.97336409133439,-0.772781854199896,
5.));
#28548=CARTESIAN_POINT('Ctrl Pts',(-2.00796690665968,-0.702658135348163,
5.));
#28549=CARTESIAN_POINT('Ctrl Pts',(-2.03880011439901,-0.631020466449058,
5.));
#28550=CARTESIAN_POINT('Ctrl Pts',(-2.07000444132555,-0.558520541709422,
5.));
#28551=CARTESIAN_POINT('Ctrl Pts',(-2.09734851848856,-0.484469191405541,
5.));
#28552=CARTESIAN_POINT('Ctrl Pts',(-2.12069441174469,-0.409223850782309,
5.));
#28553=CARTESIAN_POINT('Ctrl Pts',(-2.14389726846613,-0.334439526263928,
5.));
#28554=CARTESIAN_POINT('Ctrl Pts',(-2.16315133497366,-0.258474862586811,
5.));
#28555=CARTESIAN_POINT('Ctrl Pts',(-2.17827758432059,-0.181654682439834,
5.));
#28556=CARTESIAN_POINT('Ctrl Pts',(-2.1821185547538,-0.162147927404194,
5.));
#28557=CARTESIAN_POINT('Ctrl Pts',(-2.18569312293337,-0.142585917374366,
5.));
#28558=CARTESIAN_POINT('Ctrl Pts',(-2.18899783935687,-0.122973812778064,
5.));
#28559=CARTESIAN_POINT('Ctrl Pts',(-2.19117568691587,-0.110049201813536,
5.));
#28560=CARTESIAN_POINT('Ctrl Pts',(-2.19323666341748,-0.0971006168957883,
5.));
#28561=CARTESIAN_POINT('Ctrl Pts',(-2.19517866938162,-0.0841366491538629,
5.));
#28562=CARTESIAN_POINT('Ctrl Pts',(-2.20719266907519,-0.00393653269949183,
5.));
#28563=CARTESIAN_POINT('Ctrl Pts',(-2.21462073981273,0.07659741124565,5.));
#28564=CARTESIAN_POINT('Ctrl Pts',(-2.21733626437033,0.157086393268394,
5.));
#28565=CARTESIAN_POINT('Ctrl Pts',(-2.21853337584323,0.192569145045132,
5.));
#28566=CARTESIAN_POINT('Ctrl Pts',(-2.21881410288858,0.228043565217086,
5.));
#28567=CARTESIAN_POINT('Ctrl Pts',(-2.21816479719429,0.26347878735506,5.));
#28568=CARTESIAN_POINT('Ctrl Pts',(-2.21672815511135,0.341882121545975,
5.));
#28569=CARTESIAN_POINT('Ctrl Pts',(-2.21074233778476,0.42009311079211,5.));
#28570=CARTESIAN_POINT('Ctrl Pts',(-2.20044788110181,0.497853177799087,
5.));
#28571=CARTESIAN_POINT('Ctrl Pts',(-2.19015342441887,0.575613244806064,
5.));
#28572=CARTESIAN_POINT('Ctrl Pts',(-2.17555003407646,0.652923153155624,
5.));
#28573=CARTESIAN_POINT('Ctrl Pts',(-2.15682597556414,0.729526478768245,
5.));
#28574=CARTESIAN_POINT('Ctrl Pts',(-2.15351333591367,0.743079054114864,
5.));
#28575=CARTESIAN_POINT('Ctrl Pts',(-2.15007106234521,0.756611497694574,
5.));
#28576=CARTESIAN_POINT('Ctrl Pts',(-2.14650173555311,0.770115975691647,
5.));
#28577=CARTESIAN_POINT('Ctrl Pts',(-2.14362734645692,0.780991170529645,
5.));
#28578=CARTESIAN_POINT('Ctrl Pts',(-2.14067167855265,0.791844072988402,
5.));
#28579=CARTESIAN_POINT('Ctrl Pts',(-2.13763596071444,0.802672401844663,
5.));
#28580=CARTESIAN_POINT('Ctrl Pts',(-2.11580129108532,0.880556116936863,
5.));
#28581=CARTESIAN_POINT('Ctrl Pts',(-2.089821911864,0.957197613250287,5.));
#28582=CARTESIAN_POINT('Ctrl Pts',(-2.05997091461799,1.03232750463359,5.));
#28583=CARTESIAN_POINT('Ctrl Pts',(-2.02958681930464,1.10879911333258,5.));
#28584=CARTESIAN_POINT('Ctrl Pts',(-1.99519138342501,1.18370546487653,5.));
#28585=CARTESIAN_POINT('Ctrl Pts',(-1.95701797710563,1.25676376200865,5.));
#28586=CARTESIAN_POINT('Ctrl Pts',(-1.91845318815751,1.33057110805044,5.));
#28587=CARTESIAN_POINT('Ctrl Pts',(-1.87603226072822,1.40249322828441,5.));
#28588=CARTESIAN_POINT('Ctrl Pts',(-1.82994451627638,1.47222660890071,5.));
#28589=CARTESIAN_POINT('Ctrl Pts',(-1.81136251787481,1.50034223014795,5.));
#28590=CARTESIAN_POINT('Ctrl Pts',(-1.79218388918198,1.52810183780879,5.));
#28591=CARTESIAN_POINT('Ctrl Pts',(-1.77241889109871,1.55548446600544,5.));
#28592=CARTESIAN_POINT('Ctrl Pts',(-1.7626765455579,1.56898161002658,5.));
#28593=CARTESIAN_POINT('Ctrl Pts',(-1.75278959954955,1.58238978774029,5.));
#28594=CARTESIAN_POINT('Ctrl Pts',(-1.74277497729945,1.59568597132499,5.));
#28595=CARTESIAN_POINT('Ctrl Pts',(-1.69111299121085,1.66427640182051,5.));
#28596=CARTESIAN_POINT('Ctrl Pts',(-1.63598077918668,1.72999683047024,5.));
#28597=CARTESIAN_POINT('Ctrl Pts',(-1.57763490532952,1.79255088797377,5.));
#28598=CARTESIAN_POINT('Ctrl Pts',(-1.51919867470482,1.85520181920732,5.));
#28599=CARTESIAN_POINT('Ctrl Pts',(-1.45753838720462,1.91467750037871,5.));
#28600=CARTESIAN_POINT('Ctrl Pts',(-1.39286260070177,1.97066278379734,5.));
#28601=CARTESIAN_POINT('Ctrl Pts',(-1.32955699149425,2.02546200101775,5.));
#28602=CARTESIAN_POINT('Ctrl Pts',(-1.2633617398569,2.0769179289258,5.));
#28603=CARTESIAN_POINT('Ctrl Pts',(-1.19443292968338,2.12470580679072,5.));
#28604=CARTESIAN_POINT('Ctrl Pts',(-1.15551571854606,2.15168684603965,5.));
#28605=CARTESIAN_POINT('Ctrl Pts',(-1.11572644903728,2.17749801406487,5.));
#28606=CARTESIAN_POINT('Ctrl Pts',(-1.07508846035129,2.20207516956608,5.));
#28607=CARTESIAN_POINT('Ctrl Pts',(-1.16055672420885,-1.62238579024646,
4.99906051802604));
#28608=CARTESIAN_POINT('Ctrl Pts',(-1.15296330661381,-1.6278176621863,4.99937367868403));
#28609=CARTESIAN_POINT('Ctrl Pts',(-1.14533175338124,-1.63319622287715,
4.99968683934202));
#28610=CARTESIAN_POINT('Ctrl Pts',(-1.13766281679009,-1.63852094212837,
5.));
#28611=CARTESIAN_POINT('Ctrl Pts',(1.42649653067546,-1.99643148636002,4.73497408903594));
#28612=CARTESIAN_POINT('Ctrl Pts',(2.09139037751359,-1.52138205586238,4.77737691639768));
#28613=CARTESIAN_POINT('Ctrl Pts',(2.89731909148689,0.136761439869381,4.86216507623168));
#28614=CARTESIAN_POINT('Ctrl Pts',(1.450500801584,2.51483958866074,4.98933856853792));
#28615=CARTESIAN_POINT('Ctrl Pts',(-1.32772456687247,2.57864173676513,5.11649456595466));
#28616=CARTESIAN_POINT('Ctrl Pts',(-2.88753967722034,0.281082199765186,
5.24365056337139));
#28617=CARTESIAN_POINT('Ctrl Pts',(-1.79931443848377,-2.27620402637004,
5.37080656078811));
#28618=CARTESIAN_POINT('Ctrl Pts',(0.939379116963788,-2.74480255219456,
5.49796255820487));
#28619=CARTESIAN_POINT('Ctrl Pts',(2.81640211996325,-0.696461296195236,
5.6251185556216));
#28620=CARTESIAN_POINT('Ctrl Pts',(2.11033728095063,1.99093472149687,5.75227455303834));
#28621=CARTESIAN_POINT('Ctrl Pts',(-0.5313048515864,2.85214731506389,5.87943055045507));
#28622=CARTESIAN_POINT('Ctrl Pts',(-2.68563315664284,1.09751416275767,6.00658654787181));
#28623=CARTESIAN_POINT('Ctrl Pts',(-2.37676949737353,-1.66377294249894,
6.13374254528854));
#28624=CARTESIAN_POINT('Ctrl Pts',(0.112014575536817,-2.89906596147756,
6.26089854270528));
#28625=CARTESIAN_POINT('Ctrl Pts',(2.49805957031855,-1.47541536341306,6.38805454012201));
#28626=CARTESIAN_POINT('Ctrl Pts',(2.59294454333804,1.30145701646242,6.51521053753876));
#28627=CARTESIAN_POINT('Ctrl Pts',(0.309641675430814,2.88466083104124,6.64236653495548));
#28628=CARTESIAN_POINT('Ctrl Pts',(-2.25765691753952,1.82212366411349,6.76952253237223));
#28629=CARTESIAN_POINT('Ctrl Pts',(-2.75428622481087,-0.911622988399715,
6.89667852978896));
#28630=CARTESIAN_POINT('Ctrl Pts',(-0.724749385783444,-2.80925019841095,
7.0238345272057));
#28631=CARTESIAN_POINT('Ctrl Pts',(1.96951037757824,-2.13029991471801,7.15099052462243));
#28632=CARTESIAN_POINT('Ctrl Pts',(2.85738190749746,0.502511097857537,7.27814652203917));
#28633=CARTESIAN_POINT('Ctrl Pts',(1.12453044029566,2.6744307744314,7.4053025194559));
#28634=CARTESIAN_POINT('Ctrl Pts',(-1.6397136974498,2.39342594277931,7.53245851687264));
#28635=CARTESIAN_POINT('Ctrl Pts',(-2.90005128457351,-0.082772473702611,
7.65961451428937));
#28636=CARTESIAN_POINT('Ctrl Pts',(-1.50053054250907,-2.48305392933439,
7.78677051170611));
#28637=CARTESIAN_POINT('Ctrl Pts',(1.27524126036236,-2.60593715651519,7.91392650912285));
#28638=CARTESIAN_POINT('Ctrl Pts',(2.88139199384887,-0.338716563466436,
8.04108250653958));
#28639=CARTESIAN_POINT('Ctrl Pts',(1.84479825889604,2.2391668351018,8.16823850395633));
#28640=CARTESIAN_POINT('Ctrl Pts',(-0.88380073035943,2.76333946557476,8.29539450137305));
#28641=CARTESIAN_POINT('Ctrl Pts',(-2.80179862960237,0.75304260940714,8.42255049878981));
#28642=CARTESIAN_POINT('Ctrl Pts',(-2.15005320849511,-1.94792708615075,
8.54970649620651));
#28643=CARTESIAN_POINT('Ctrl Pts',(0.473670074415001,-2.86230421044614,
8.67686249362328));
#28644=CARTESIAN_POINT('Ctrl Pts',(2.66295438770209,-1.15144372917626,8.80401849103999));
#28645=CARTESIAN_POINT('Ctrl Pts',(2.4098400297151,1.61549365941736,8.93117448845674));
#28646=CARTESIAN_POINT('Ctrl Pts',(-0.0535225074078562,2.90073853934904,
9.05833048587348));
#28647=CARTESIAN_POINT('Ctrl Pts',(-2.46779546884147,1.52549475791126,9.1854864832902));
#28648=CARTESIAN_POINT('Ctrl Pts',(-2.61866489550199,-1.24889667207306,
9.31264248070695));
#28649=CARTESIAN_POINT('Ctrl Pts',(-0.367756923792801,-2.87782966442698,
9.43979847812368));
#28650=CARTESIAN_POINT('Ctrl Pts',(2.22044898518867,-1.86728547271856,9.56695447554042));
#28651=CARTESIAN_POINT('Ctrl Pts',(2.77211169384673,0.85588871314536,9.69411047295715));
#28652=CARTESIAN_POINT('Ctrl Pts',(0.781259236293708,2.79406204980448,9.82126647037389));
#28653=CARTESIAN_POINT('Ctrl Pts',(-1.92614568248534,2.16958787383562,9.94842246779061));
#28654=CARTESIAN_POINT('Ctrl Pts',(-2.86693541727973,-0.444780896171051,
10.0755784652073));
#28655=CARTESIAN_POINT('Ctrl Pts',(-1.17823991337992,-2.65120716636218,
10.2027344626241));
#28656=CARTESIAN_POINT('Ctrl Pts',(1.59110932314304,-2.42600903837123,10.3298904600408));
#28657=CARTESIAN_POINT('Ctrl Pts',(2.90113078648473,0.0242671004068106,
10.4570464574575));
#28658=CARTESIAN_POINT('Ctrl Pts',(1.55030382868508,2.45228602964989,10.5842024548743));
#28659=CARTESIAN_POINT('Ctrl Pts',(-1.22242506957978,2.63112631428339,10.711358452291));
#28660=CARTESIAN_POINT('Ctrl Pts',(-2.8739746568298,0.396759882487747,10.8385144497078));
#28661=CARTESIAN_POINT('Ctrl Pts',(-1.88958278165034,-2.20150531313058,
10.9656704471245));
#28662=CARTESIAN_POINT('Ctrl Pts',(0.827889651149327,-2.78060199560661,
11.0928264445412));
#28663=CARTESIAN_POINT('Ctrl Pts',(2.78604131102751,-0.809396408257279,
11.219982441958));
#28664=CARTESIAN_POINT('Ctrl Pts',(2.18890188984948,1.90416838779164,11.3471384393747));
#28665=CARTESIAN_POINT('Ctrl Pts',(-0.415846483249164,2.87127505384296,
11.4742944367915));
#28666=CARTESIAN_POINT('Ctrl Pts',(-2.6391903145238,1.2049162693629,11.6014504342082));
#28667=CARTESIAN_POINT('Ctrl Pts',(-2.44193131940839,-1.56656316940748,
11.7286064316249));
#28668=CARTESIAN_POINT('Ctrl Pts',(-0.00499077458373336,-2.9012279856331,
11.8557624290416));
#28669=CARTESIAN_POINT('Ctrl Pts',(2.43652719044317,-1.57495523196144,11.9829184264584));
#28670=CARTESIAN_POINT('Ctrl Pts',(2.64332014480819,1.19582914519711,12.1100744238751));
#28671=CARTESIAN_POINT('Ctrl Pts',(0.425722490293999,2.86982736304983,12.2372304212918));
#28672=CARTESIAN_POINT('Ctrl Pts',(-2.1823377457144,1.9116879180666,12.3643864187086));
#28673=CARTESIAN_POINT('Ctrl Pts',(-2.78880950727922,-0.799806391922873,
12.4915424161253));
#28674=CARTESIAN_POINT('Ctrl Pts',(-0.837451263772367,-2.77773722897932,
12.6186984135421));
#28675=CARTESIAN_POINT('Ctrl Pts',(1.88199743721141,-2.2079932922863,12.7458544109588));
#28676=CARTESIAN_POINT('Ctrl Pts',(2.87532267877552,0.386869778311558,12.8730104083755));
#28677=CARTESIAN_POINT('Ctrl Pts',(1.23147008412008,2.62690505431182,13.0001664057923));
#28678=CARTESIAN_POINT('Ctrl Pts',(-1.54185769458389,2.45760525351491,13.127322403209));
#28679=CARTESIAN_POINT('Ctrl Pts',(-2.90103012690677,0.034248142007324,
13.2544784006258));
#28680=CARTESIAN_POINT('Ctrl Pts',(-1.59944646066832,-2.42052055391133,
13.3816343980425));
#28681=CARTESIAN_POINT('Ctrl Pts',(1.16911160375855,-2.65524514695135,13.5087903954592));
#28682=CARTESIAN_POINT('Ctrl Pts',(2.86538820487081,-0.454641801684438,
13.6359463928759));
#28683=CARTESIAN_POINT('Ctrl Pts',(1.93359863385237,2.16294823230143,13.7631023902927));
#28684=CARTESIAN_POINT('Ctrl Pts',(-0.771641791562487,2.79673339415216,
13.8902583877094));
#28685=CARTESIAN_POINT('Ctrl Pts',(-2.76915064819359,0.865420949631279,
14.0174143851262));
#28686=CARTESIAN_POINT('Ctrl Pts',(-2.22686013953083,-1.85963508555317,
14.1445703825429));
#28687=CARTESIAN_POINT('Ctrl Pts',(0.357853728318975,-2.87907788042974,
14.2717263799596));
#28688=CARTESIAN_POINT('Ctrl Pts',(2.6143526351498,-1.25789865710119,14.3988823773764));
#28689=CARTESIAN_POINT('Ctrl Pts',(2.47302924663558,1.51699541124444,14.5260383747931));
#28690=CARTESIAN_POINT('Ctrl Pts',(0.0635020263596358,2.90053723042815,
14.6531943722098));
#28691=CARTESIAN_POINT('Ctrl Pts',(-2.40426774794574,1.62377502402257,14.7803503696266));
#28692=CARTESIAN_POINT('Ctrl Pts',(-2.66690010792791,-1.14227516246556,
14.9075063670433));
#28693=CARTESIAN_POINT('Ctrl Pts',(-0.483514875535344,-2.86065763375971,
15.0346623644601));
#28694=CARTESIAN_POINT('Ctrl Pts',(2.14333874482516,-1.95531270066527,15.1618183618768));
#28695=CARTESIAN_POINT('Ctrl Pts',(2.80437285035799,0.743398714437,15.2889743592935));
#28696=CARTESIAN_POINT('Ctrl Pts',(0.893302621288155,2.7602824419344,15.4161303567102));
#28697=CARTESIAN_POINT('Ctrl Pts',(-1.83708360709109,2.2455005128053,15.543286354127));
#28698=CARTESIAN_POINT('Ctrl Pts',(-2.88254027689778,-0.328801284233579,
15.6704423515437));
#28699=CARTESIAN_POINT('Ctrl Pts',(-1.2841993004931,-2.60153433363172,15.7975983489605));
#28700=CARTESIAN_POINT('Ctrl Pts',(1.49197884790902,-2.48820173013437,15.9247543463772));
#28701=CARTESIAN_POINT('Ctrl Pts',(2.89974934632536,-0.0927494524904423,
16.0519103437939));
#28702=CARTESIAN_POINT('Ctrl Pts',(1.64793844778422,2.38777042547358,16.1790663412107));
#28703=CARTESIAN_POINT('Ctrl Pts',(-1.11532255061193,2.67828384241628,16.3062223386274));
#28704=CARTESIAN_POINT('Ctrl Pts',(-2.85563613082048,0.512338775425298,
16.4333783360441));
#28705=CARTESIAN_POINT('Ctrl Pts',(-1.97682791016231,-2.12351127759072,
16.5605343334609));
#28706=CARTESIAN_POINT('Ctrl Pts',(0.715080032896517,-2.81172709895614,
16.6876903308776));
#28707=CARTESIAN_POINT('Ctrl Pts',(2.75113351210751,-0.92109344314821,16.8148463282943));
#28708=CARTESIAN_POINT('Ctrl Pts',(2.26391251636448,1.8143452953338,16.9420023257111));
#28709=CARTESIAN_POINT('Ctrl Pts',(-0.299715400718915,2.88570951605034,
17.0691583231278));
#28710=CARTESIAN_POINT('Ctrl Pts',(-2.58845145339209,1.31036933949326,17.1963143205446));
#28711=CARTESIAN_POINT('Ctrl Pts',(-2.5031211609541,-1.46681054878789,17.3234703179612));
#28712=CARTESIAN_POINT('Ctrl Pts',(-0.121987445906368,-2.898666554727,17.4506263153781));
#28713=CARTESIAN_POINT('Ctrl Pts',(2.37103026428945,-1.67193427450816,17.5777823127947));
#28714=CARTESIAN_POINT('Ctrl Pts',(2.68939519267899,1.08825650930596,17.7049383102115));
#28715=CARTESIAN_POINT('Ctrl Pts',(0.541110569934063,2.85032420674513,17.8320943076282));
#28716=CARTESIAN_POINT('Ctrl Pts',(-2.10346784707187,1.99814207422457,17.959250305045));
#28717=CARTESIAN_POINT('Ctrl Pts',(-2.81879539201196,-0.686688626980042,
18.0864063024617));
#28718=CARTESIAN_POINT('Ctrl Pts',(-0.948790588856309,-2.74170478916847,
18.2135622998784));
#28719=CARTESIAN_POINT('Ctrl Pts',(1.79142246279098,-2.2820942776887,18.3407182972952));
#28720=CARTESIAN_POINT('Ctrl Pts',(2.88858527557254,0.270599035839221,18.4678742947119));
#28721=CARTESIAN_POINT('Ctrl Pts',(1.33640611258182,2.57510532497325,18.5950302921287));
#28722=CARTESIAN_POINT('Ctrl Pts',(-1.44149307352296,2.51778602177329,18.7221862895454));
#28723=CARTESIAN_POINT('Ctrl Pts',(-2.89728896575409,0.151213033073416,
18.8493422869621));
#28724=CARTESIAN_POINT('Ctrl Pts',(-1.69576006379414,-2.35404896688503,
18.9764982843789));
#28725=CARTESIAN_POINT('Ctrl Pts',(1.06107979119196,-2.70023302868023,19.1036542817956));
#28726=CARTESIAN_POINT('Ctrl Pts',(2.84472240176183,-0.569827332940471,
19.2308102792123));
#28727=CARTESIAN_POINT('Ctrl Pts',(2.01925302517959,2.08321049170619,19.3579662766291));
#28728=CARTESIAN_POINT('Ctrl Pts',(-0.658227384122869,2.82557701067276,
19.4851222740458));
#28729=CARTESIAN_POINT('Ctrl Pts',(-2.73199723202815,0.976391241584123,
19.6122782714625));
#28730=CARTESIAN_POINT('Ctrl Pts',(-2.30004394767405,-1.7683174407384,19.7394342688793));
#28731=CARTESIAN_POINT('Ctrl Pts',(0.241455150758871,-2.89116726299665,
19.866590266296));
#28732=CARTESIAN_POINT('Ctrl Pts',(2.56149730569025,-1.36230697179206,19.9937462637128));
#28733=CARTESIAN_POINT('Ctrl Pts',(2.53219482116047,1.41602899692759,20.1209022611294));
#28734=CARTESIAN_POINT('Ctrl Pts',(0.180423241719181,2.89561671950885,20.2480582585463));
#28735=CARTESIAN_POINT('Ctrl Pts',(-2.3368282602758,1.71941339253478,20.375214255963));
#28736=CARTESIAN_POINT('Ctrl Pts',(-2.71079624820093,-1.03379516017022,
20.5023702533797));
#28737=CARTESIAN_POINT('Ctrl Pts',(-0.598486143920099,-2.83883128557993,
20.6295262507964));
#28738=CARTESIAN_POINT('Ctrl Pts',(2.0627412716876,-2.04015861602187,20.7566822482131));
#28739=CARTESIAN_POINT('Ctrl Pts',(2.83207126524092,0.629699198862666,20.8838382456299));
#28740=CARTESIAN_POINT('Ctrl Pts',(1.00389259431695,2.72201182795505,21.0109942430466));
#28741=CARTESIAN_POINT('Ctrl Pts',(-1.74503257898048,2.31775970082069,21.1381502404634));
#28742=CARTESIAN_POINT('Ctrl Pts',(-2.89345521573194,-0.212286709440951,
21.2653062378801));
#28743=CARTESIAN_POINT('Ctrl Pts',(-1.38806928297995,-2.54762877949265,
21.3924622352968));
#28744=CARTESIAN_POINT('Ctrl Pts',(1.39042090872455,-2.54634609372591,21.5196182327136));
#28745=CARTESIAN_POINT('Ctrl Pts',(2.89364998606044,-0.209615101135453,
21.6467742301303));
#28746=CARTESIAN_POINT('Ctrl Pts',(1.74289185516227,2.3193698958253,21.773930227547));
#28747=CARTESIAN_POINT('Ctrl Pts',(-1.00640539111578,2.72108377695078,21.9010862249638));
#28748=CARTESIAN_POINT('Ctrl Pts',(-2.83265145733194,0.627084088242402,
22.0282422223805));
#28749=CARTESIAN_POINT('Ctrl Pts',(-2.06085672063136,-2.04206226875681,
22.1553982197973));
#28750=CARTESIAN_POINT('Ctrl Pts',(0.601106972545297,-2.83827749524409,
22.282554217214));
#28751=CARTESIAN_POINT('Ctrl Pts',(2.71174959247513,-1.03129185013877,22.4097102146307));
#28752=CARTESIAN_POINT('Ctrl Pts',(2.33523973541819,1.72157024561173,22.5368662120475));
#28753=CARTESIAN_POINT('Ctrl Pts',(-0.18309667834599,2.89544890109121,22.6640222094642));
#28754=CARTESIAN_POINT('Ctrl Pts',(-2.53350115682382,1.41369042609194,22.7911782068809));
#28755=CARTESIAN_POINT('Ctrl Pts',(-2.56023840027064,-1.36467141328281,
22.9183342042977));
#28756=CARTESIAN_POINT('Ctrl Pts',(-0.238785642480034,-2.8913889654277,
23.0454902017144));
#28757=CARTESIAN_POINT('Ctrl Pts',(2.3016756490672,-1.76619306389272,23.1726461991311));
#28758=CARTESIAN_POINT('Ctrl Pts',(2.73109456867753,0.978913269596307,23.2998021965479));
#28759=CARTESIAN_POINT('Ctrl Pts',(0.655618257466982,2.82618354551285,23.4269581939646));
#28760=CARTESIAN_POINT('Ctrl Pts',(-2.02117558598974,2.08134523398946,23.5541141913814));
#28761=CARTESIAN_POINT('Ctrl Pts',(-2.84419506950227,-0.572453613029604,
23.6812701887981));
#28762=CARTESIAN_POINT('Ctrl Pts',(-1.05858622251712,-2.70121156926823,
23.8084261862149));
#28763=CARTESIAN_POINT('Ctrl Pts',(1.6979328267756,-2.35248227372907,23.9355821836315));
#28764=CARTESIAN_POINT('Ctrl Pts',(2.89714811631462,0.153888026130212,24.0627381810483));
#28765=CARTESIAN_POINT('Ctrl Pts',(1.43916779543132,2.51911587447759,24.189894178465));
#28766=CARTESIAN_POINT('Ctrl Pts',(-1.33878312935259,2.57387032793273,24.3170501758818));
#28767=CARTESIAN_POINT('Ctrl Pts',(-2.88883388755873,0.26793189907875,24.4442061732985));
#28768=CARTESIAN_POINT('Ctrl Pts',(-1.78931464896918,-2.28374731952464,
24.5713621707153));
#28769=CARTESIAN_POINT('Ctrl Pts',(0.951321591588982,-2.74082760527331,
24.698518168132));
#28770=CARTESIAN_POINT('Ctrl Pts',(2.81942820791591,-0.684085749639387,
24.8256741655487));
#28771=CARTESIAN_POINT('Ctrl Pts',(2.10162207239324,2.00008334758359,24.9528301629654));
#28772=CARTESIAN_POINT('Ctrl Pts',(-0.543742034391811,2.84982338619205,
25.0799861603822));
#28773=CARTESIAN_POINT('Ctrl Pts',(-2.69039883006224,1.08577293558616,25.2071421577989));
#28774=CARTESIAN_POINT('Ctrl Pts',(-2.36948556216938,-1.67412272642197,
25.3342981552157));
#28775=CARTESIAN_POINT('Ctrl Pts',(0.12466372334371,-2.89855268859024,25.4614541526324));
#28776=CARTESIAN_POINT('Ctrl Pts',(2.50447439545198,-1.46449879992339,25.5886101500491));
#28777=CARTESIAN_POINT('Ctrl Pts',(2.58724049033111,1.31275868979903,25.7157661474659));
#28778=CARTESIAN_POINT('Ctrl Pts',(0.297050906727364,2.8859850123076,25.8429221448826));
#28779=CARTESIAN_POINT('Ctrl Pts',(-2.26558673052715,1.81225425890269,25.9700781422993));
#28780=CARTESIAN_POINT('Ctrl Pts',(-2.75028189687831,-0.923633163195802,
26.0972341397161));
#28781=CARTESIAN_POINT('Ctrl Pts',(-0.712483669586427,-2.81238613156592,
26.2243901371328));
#28782=CARTESIAN_POINT('Ctrl Pts',(1.97878769864067,-2.12168517366737,26.3515461345495));
#28783=CARTESIAN_POINT('Ctrl Pts',(2.85516187290784,0.514975156628957,26.4787021319663));
#28784=CARTESIAN_POINT('Ctrl Pts',(1.11284922442921,2.67931247452382,26.605858129383));
#28785=CARTESIAN_POINT('Ctrl Pts',(-1.6501423660625,2.38624787148722,26.7330141267998));
#28786=CARTESIAN_POINT('Ctrl Pts',(-2.89966247507162,-0.0954267421280935,
26.8601701242165));
#28787=CARTESIAN_POINT('Ctrl Pts',(-1.48968086337897,-2.48957820880047,
26.9873261216332));
#28788=CARTESIAN_POINT('Ctrl Pts',(1.28660074133443,-2.60034752770651,27.11448211905));
#28789=CARTESIAN_POINT('Ctrl Pts',(2.88284262940784,-0.326139703992787,
27.2416381164667));
#28790=CARTESIAN_POINT('Ctrl Pts',(1.83500956071125,2.24719572902539,27.3687941138834));
#28791=CARTESIAN_POINT('Ctrl Pts',(-0.895850800358501,2.75945648198132,
27.4959501113002));
#28792=CARTESIAN_POINT('Ctrl Pts',(-2.80505803264929,0.740809129210285,
27.6231061087169));
#28793=CARTESIAN_POINT('Ctrl Pts',(-2.14153249737378,-1.95729080495048,
27.7502621061337));
#28794=CARTESIAN_POINT('Ctrl Pts',(0.486155905362252,-2.86020998672004,
27.8774181035504));
#28795=CARTESIAN_POINT('Ctrl Pts',(2.66795363014677,-1.13981233535976,28.0045741009671));
#28796=CARTESIAN_POINT('Ctrl Pts',(2.40276749693843,1.62599418452461,28.1317300983839));
#28797=CARTESIAN_POINT('Ctrl Pts',(-0.0661800559145379,2.90047736289232,
28.2588860958006));
#28798=CARTESIAN_POINT('Ctrl Pts',(-2.4744288294806,1.51471142475617,28.3860420932174));
#28799=CARTESIAN_POINT('Ctrl Pts',(-2.61319010705968,-1.26031194424914,
28.5131980906341));
#28800=CARTESIAN_POINT('Ctrl Pts',(-0.355195332514304,-2.87940705844306,
28.6403540880508));
#28801=CARTESIAN_POINT('Ctrl Pts',(2.22857618540315,-1.85757824015722,28.7675100854675));
#28802=CARTESIAN_POINT('Ctrl Pts',(2.76835042751757,0.867977328571968,28.8946660828843));
#28803=CARTESIAN_POINT('Ctrl Pts',(0.769059247782621,2.79744465644124,29.021822080301));
#28804=CARTESIAN_POINT('Ctrl Pts',(-1.93559485276915,2.16116202501923,29.1489780777177));
#28805=CARTESIAN_POINT('Ctrl Pts',(-2.86496721423027,-0.457287211539142,
29.2761340751345));
#28806=CARTESIAN_POINT('Ctrl Pts',(-1.16665952620171,-2.65632345213726,
29.4032900725512));
#28807=CARTESIAN_POINT('Ctrl Pts',(1.60168063770319,-2.41904275846012,29.5304460699679));
#28808=CARTESIAN_POINT('Ctrl Pts',(2.90099726917742,0.0369266391210829,
29.6576020673847));
#28809=CARTESIAN_POINT('Ctrl Pts',(1.53958793842119,2.45902779819983,29.7847580648014));
#28810=CARTESIAN_POINT('Ctrl Pts',(-1.23389497214082,2.62576692228718,29.9119140622182));
#28811=CARTESIAN_POINT('Ctrl Pts',(-2.8756786488143,0.38421483730457,30.0390700596349));
#28812=CARTESIAN_POINT('Ctrl Pts',(-1.87995800198274,-2.20972999328701,
30.1662260570517));
#28813=CARTESIAN_POINT('Ctrl Pts',(0.840015582597118,-2.77696282896395,
30.2933820544683));
#28814=CARTESIAN_POINT('Ctrl Pts',(2.78954677722976,-0.797231152236704,
30.4205380518851));
#28815=CARTESIAN_POINT('Ctrl Pts',(2.18057176026088,1.91370204859638,30.5476940493018));
#28816=CARTESIAN_POINT('Ctrl Pts',(-0.428372011136305,2.86943307162567,
30.6748500467186));
#28817=CARTESIAN_POINT('Ctrl Pts',(-2.644423123295,1.19338806656412,30.8020060441353));
#28818=CARTESIAN_POINT('Ctrl Pts',(-2.43507200084404,-1.5772041983036,30.929162041552));
#28819=CARTESIAN_POINT('Ctrl Pts',(0.00766946685548332,-2.9012221410661,
31.0563180389688));
#28820=CARTESIAN_POINT('Ctrl Pts',(2.44337668124933,-1.56430787437987,31.1834740363855));
#28821=CARTESIAN_POINT('Ctrl Pts',(2.63807669433218,1.20735251159128,31.3106300338023));
#28822=CARTESIAN_POINT('Ctrl Pts',(0.413195267015108,2.87165777980301,31.437786031219));
#28823=CARTESIAN_POINT('Ctrl Pts',(-2.19065906928768,1.90214656995545,31.5649420286357));
#28824=CARTESIAN_POINT('Ctrl Pts',(-2.78529281055713,-0.81196840581493,
31.6920980260525));
#28825=CARTESIAN_POINT('Ctrl Pts',(-0.825321977219055,-2.78136519891875,
31.8192540234692));
#28826=CARTESIAN_POINT('Ctrl Pts',(1.89161461849208,-2.19975972780952,31.946410020886));
#28827=CARTESIAN_POINT('Ctrl Pts',(2.87360710560243,0.399413242382576,32.0735660183027));
#28828=CARTESIAN_POINT('Ctrl Pts',(1.21999523645203,2.63225385861773,32.2007220157194));
#28829=CARTESIAN_POINT('Ctrl Pts',(-1.55256735241157,2.45085358489712,32.3278780131362));
#28830=CARTESIAN_POINT('Ctrl Pts',(-2.90115196177673,0.0215885025613874,
32.4550340105528));
#28831=CARTESIAN_POINT('Ctrl Pts',(-1.58886870698235,-2.42747710308629,
32.5821900079697));
#28832=CARTESIAN_POINT('Ctrl Pts',(1.18068723986726,-2.65011810889251,32.7093460053863));
#28833=CARTESIAN_POINT('Ctrl Pts',(2.86734490252435,-0.442133793245194,
32.8365020028031));
#28834=CARTESIAN_POINT('Ctrl Pts',(1.92414160704232,2.1713655796952,32.9636580002198));
#28835=CARTESIAN_POINT('Ctrl Pts',(-0.783838497306285,2.79333909281486,
33.0908139976365));
#28836=CARTESIAN_POINT('Ctrl Pts',(-2.77290104593788,0.853329690074369,
33.2179699950533));
#28837=CARTESIAN_POINT('Ctrl Pts',(-2.21872341885293,-1.86933638013305,
33.34512599247));
#28838=CARTESIAN_POINT('Ctrl Pts',(0.370412787773323,-2.87748589584457,
33.4722819898868));
#28839=CARTESIAN_POINT('Ctrl Pts',(2.61981892166448,-1.24648404142433,33.5994379873035));
#28840=CARTESIAN_POINT('Ctrl Pts',(2.46638204316312,1.5277834946993,33.7265939847202));
#28841=CARTESIAN_POINT('Ctrl Pts',(0.0508516573559641,2.90076597833909,
33.853749982137));
#28842=CARTESIAN_POINT('Ctrl Pts',(-2.41134471984188,1.61330751771713,33.9809059795537));
#28843=CARTESIAN_POINT('Ctrl Pts',(-2.66186317555782,-1.15397732778452,
34.1080619769705));
#28844=CARTESIAN_POINT('Ctrl Pts',(-0.471078502934338,-2.86259658701582,
34.2352179743872));
#28845=CARTESIAN_POINT('Ctrl Pts',(2.15194878338818,-1.94621521211644,34.3623739718039));
#28846=CARTESIAN_POINT('Ctrl Pts',(2.80091529373492,0.756152172428542,34.4895299692206));
#28847=CARTESIAN_POINT('Ctrl Pts',(0.881605804944954,2.76315344068171,34.6166859666374));
#28848=CARTESIAN_POINT('Ctrl Pts',(-1.84755030053663,2.23940363022795,34.7438419640541));
#28849=CARTESIAN_POINT('Ctrl Pts',(-2.87978905100241,-0.345521145569797,
34.8710057240579));
#28850=CARTESIAN_POINT('Ctrl Pts',(-1.81030869183372,-1.84686632628722,
34.9557841515895));
#28851=CARTESIAN_POINT('Ctrl Pts',(-1.07608793779701,-2.20514531190313,
34.9981772466487));
#28852=CARTESIAN_POINT('Ctrl Pts',(1.33686590078714,-1.87099030385222,4.82398558717196));
#28853=CARTESIAN_POINT('Ctrl Pts',(1.95998267139732,-1.42578951214757,4.8663884145337));
#28854=CARTESIAN_POINT('Ctrl Pts',(2.71527270751542,0.128168349219389,4.9511765743677));
#28855=CARTESIAN_POINT('Ctrl Pts',(1.35936191852075,2.35682542490182,5.07835006667395));
#28856=CARTESIAN_POINT('Ctrl Pts',(-1.24430004624595,2.41661871171578,5.20550606409067));
#28857=CARTESIAN_POINT('Ctrl Pts',(-2.70610776026073,0.263421045970905,
5.33266206150741));
#28858=CARTESIAN_POINT('Ctrl Pts',(-1.68625865249321,-2.13318397952756,
5.45981805892415));
#28859=CARTESIAN_POINT('Ctrl Pts',(0.880355389848543,-2.5723391943232,5.58697405634089));
#28860=CARTESIAN_POINT('Ctrl Pts',(2.63943996786359,-0.65270075186278,5.71413005375762));
#28861=CARTESIAN_POINT('Ctrl Pts',(1.97773908971723,1.86583891557173,5.84128605117436));
#28862=CARTESIAN_POINT('Ctrl Pts',(-0.497921532744458,2.67293919581084,
5.96844204859109));
#28863=CARTESIAN_POINT('Ctrl Pts',(-2.5168875717063,1.02855438360375,6.09559804600783));
#28864=CARTESIAN_POINT('Ctrl Pts',(-2.22743065036776,-1.55923359478898,
6.22275404342456));
#28865=CARTESIAN_POINT('Ctrl Pts',(0.104976397212366,-2.7169098169464,6.3499100408413));
#28866=CARTESIAN_POINT('Ctrl Pts',(2.3410997404337,-1.38271103113762,6.47706603825804));
#28867=CARTESIAN_POINT('Ctrl Pts',(2.43002283432085,1.21968295697496,6.60422203567477));
#28868=CARTESIAN_POINT('Ctrl Pts',(0.290186052643345,2.70340979976262,6.73137803309151));
#28869=CARTESIAN_POINT('Ctrl Pts',(-2.11580223563929,1.70763471287051,6.85853403050825));
#28870=CARTESIAN_POINT('Ctrl Pts',(-2.58122698217429,-0.854343253809485,
6.98569002792498));
#28871=CARTESIAN_POINT('Ctrl Pts',(-0.679211424378038,-2.63273742085926,
7.11284602534172));
#28872=CARTESIAN_POINT('Ctrl Pts',(1.84576072104714,-1.99644741728735,7.24000202275845));
#28873=CARTESIAN_POINT('Ctrl Pts',(2.67784488466356,0.470936968332268,7.36715802017519));
#28874=CARTESIAN_POINT('Ctrl Pts',(1.05387315545497,2.50638906542604,7.49431401759193));
#28875=CARTESIAN_POINT('Ctrl Pts',(-1.5366860570886,2.24304052632082,7.62147001500866));
#28876=CARTESIAN_POINT('Ctrl Pts',(-2.71783322953095,-0.077571655617246,
7.7486260124254));
#28877=CARTESIAN_POINT('Ctrl Pts',(-1.40624815569671,-2.32703694440175,
7.87578200984213));
#28878=CARTESIAN_POINT('Ctrl Pts',(1.19511440763756,-2.44219908651995,8.00293800725887));
#28879=CARTESIAN_POINT('Ctrl Pts',(2.70034635243996,-0.317434086934477,
8.1300940046756));
#28880=CARTESIAN_POINT('Ctrl Pts',(1.72888460162041,2.09847393502153,8.25725000209234));
#28881=CARTESIAN_POINT('Ctrl Pts',(-0.82826914338782,2.58971138336883,8.38440599950907));
#28882=CARTESIAN_POINT('Ctrl Pts',(-2.62575405424508,0.705726908343466,
8.51156199692582));
#28883=CARTESIAN_POINT('Ctrl Pts',(-2.01495955826419,-1.82553356611497,
8.63871799434254));
#28884=CARTESIAN_POINT('Ctrl Pts',(0.443908104290186,-2.68245790602317,
8.76587399175929));
#28885=CARTESIAN_POINT('Ctrl Pts',(2.49563377107184,-1.07909540970433,8.89302998917602));
#28886=CARTESIAN_POINT('Ctrl Pts',(2.25842327184115,1.51398782946234,9.02018598659275));
#28887=CARTESIAN_POINT('Ctrl Pts',(-0.0501595437068742,2.7184773022327,
9.14734198400951));
#28888=CARTESIAN_POINT('Ctrl Pts',(-2.31273721419361,1.42964380201861,9.27449798142622));
#28889=CARTESIAN_POINT('Ctrl Pts',(-2.45412710728949,-1.17042512098534,
9.40165397884297));
#28890=CARTESIAN_POINT('Ctrl Pts',(-0.344649762985586,-2.69700785379723,
9.5288099762597));
#28891=CARTESIAN_POINT('Ctrl Pts',(2.08093217817404,-1.74995888306207,9.65596597367644));
#28892=CARTESIAN_POINT('Ctrl Pts',(2.5979324288453,0.802110913603682,9.78312197109316));
#28893=CARTESIAN_POINT('Ctrl Pts',(0.732170608351645,2.61850358465186,9.91027796850992));
#28894=CARTESIAN_POINT('Ctrl Pts',(-1.8051207468719,2.03326680781961,10.0374339659267));
#28895=CARTESIAN_POINT('Ctrl Pts',(-2.68679812162284,-0.416834111142922,
10.1645899633433));
#28896=CARTESIAN_POINT('Ctrl Pts',(-1.10420791727987,-2.48462465937712,
10.2917459607601));
#28897=CARTESIAN_POINT('Ctrl Pts',(1.49113562689651,-2.27357633801207,10.4189019581768));
#28898=CARTESIAN_POINT('Ctrl Pts',(2.71884490342142,0.0227423329444836,
10.5460579555935));
#28899=CARTESIAN_POINT('Ctrl Pts',(1.45289405186817,2.29820227495634,10.6732139530104));
#28900=CARTESIAN_POINT('Ctrl Pts',(-1.14561680077464,2.46580554147145,10.800369950427));
#28901=CARTESIAN_POINT('Ctrl Pts',(-2.69339506673948,0.371830387450793,
10.9275259478437));
#28902=CARTESIAN_POINT('Ctrl Pts',(-1.77085519185023,-2.06317878819687,
11.0546819452605));
#28903=CARTESIAN_POINT('Ctrl Pts',(0.775871108296341,-2.60588926201391,
11.1818379426773));
#28904=CARTESIAN_POINT('Ctrl Pts',(2.61098681055567,-0.758539845804237,
11.308993940094));
#28905=CARTESIAN_POINT('Ctrl Pts',(2.05136727204152,1.78452434496292,11.4361499375107));
#28906=CARTESIAN_POINT('Ctrl Pts',(-0.389717725534715,2.69086508709977,
11.5633059349274));
#28907=CARTESIAN_POINT('Ctrl Pts',(-2.47336285879642,1.12920812576549,11.6904619323442));
#28908=CARTESIAN_POINT('Ctrl Pts',(-2.28849817912672,-1.46813177429756,
11.817617929761));
#28909=CARTESIAN_POINT('Ctrl Pts',(-0.00467719073695795,-2.71893599528478,
11.9447739271776));
#28910=CARTESIAN_POINT('Ctrl Pts',(2.28343360618049,-1.47599654089498,12.0719299245944));
#28911=CARTESIAN_POINT('Ctrl Pts',(2.4772332006897,1.12069197015463,12.1990859220111));
#28912=CARTESIAN_POINT('Ctrl Pts',(0.398973196382628,2.68950835862925,12.326241919428));
#28913=CARTESIAN_POINT('Ctrl Pts',(-2.04521557081167,1.79157140284105,12.4533979168447));
#28914=CARTESIAN_POINT('Ctrl Pts',(-2.61358107356021,-0.749552396097977,
12.5805539142613));
#28915=CARTESIAN_POINT('Ctrl Pts',(-0.784831938973139,-2.60320449641131,
12.707709911678));
#28916=CARTESIAN_POINT('Ctrl Pts',(1.7637464550898,-2.06925911009872,12.8348659090948));
#28917=CARTESIAN_POINT('Ctrl Pts',(2.69465838882545,0.362561705232363,12.9620219065116));
#28918=CARTESIAN_POINT('Ctrl Pts',(1.15409349262152,2.46184951466517,13.0891779039284));
#28919=CARTESIAN_POINT('Ctrl Pts',(-1.44497861118487,2.30318727761913,13.216333901345));
#28920=CARTESIAN_POINT('Ctrl Pts',(-2.71875056855662,0.0320962387432519,
13.3434898987617));
#28921=CARTESIAN_POINT('Ctrl Pts',(-1.49894891955313,-2.26843270985474,
13.4706458961785));
#28922=CARTESIAN_POINT('Ctrl Pts',(1.09565316400684,-2.48840892273963,13.5978018935953));
#28923=CARTESIAN_POINT('Ctrl Pts',(2.68534812474848,-0.426075429329398,
13.724957891012));
#28924=CARTESIAN_POINT('Ctrl Pts',(1.81210540917471,2.02704435289614,13.8521138884288));
#28925=CARTESIAN_POINT('Ctrl Pts',(-0.723157453648822,2.62100708121908,
13.9792698858454));
#28926=CARTESIAN_POINT('Ctrl Pts',(-2.59515743368809,0.811044213925397,
14.1064258832623));
#28927=CARTESIAN_POINT('Ctrl Pts',(-2.08694050237286,-1.74278919038536,
14.233581880679));
#28928=CARTESIAN_POINT('Ctrl Pts',(0.335368812031106,-2.69817764101722,
14.3607378780956));
#28929=CARTESIAN_POINT('Ctrl Pts',(2.45008579790229,-1.17886148698052,14.4878938755124));
#28930=CARTESIAN_POINT('Ctrl Pts',(2.31764213959291,1.42167849225891,14.6150498729291));
#28931=CARTESIAN_POINT('Ctrl Pts',(0.0595120225290418,2.71828864209504,
14.7422058703459));
#28932=CARTESIAN_POINT('Ctrl Pts',(-2.25320111158564,1.52174885356211,14.8693618677626));
#28933=CARTESIAN_POINT('Ctrl Pts',(-2.49933157103879,-1.07050292880361,
14.9965178651794));
#28934=CARTESIAN_POINT('Ctrl Pts',(-0.453134329966127,-2.68091478819722,
15.1236738625962));
#28935=CARTESIAN_POINT('Ctrl Pts',(2.00866698248185,-1.8324551225216,15.2508298600128));
#28936=CARTESIAN_POINT('Ctrl Pts',(2.62816652975788,0.696688965341679,15.3779858574296));
#28937=CARTESIAN_POINT('Ctrl Pts',(0.837174004845652,2.58684644078056,15.5051418548462));
#28938=CARTESIAN_POINT('Ctrl Pts',(-1.721654682225,2.10440965064816,15.632297852263));
#28939=CARTESIAN_POINT('Ctrl Pts',(-2.70142248576348,-0.308141811476186,
15.7594538496798));
#28940=CARTESIAN_POINT('Ctrl Pts',(-1.20350958991195,-2.43807290488992,
15.8866098470964));
#28941=CARTESIAN_POINT('Ctrl Pts',(1.39823378716581,-2.33186129497368,16.0137658445133));
#28942=CARTESIAN_POINT('Ctrl Pts',(2.71755026287845,-0.0869217538808249,
16.14092184193));
#28943=CARTESIAN_POINT('Ctrl Pts',(1.54439402414511,2.23774036044249,16.2680778393468));
#28944=CARTESIAN_POINT('Ctrl Pts',(-1.04524382234984,2.51000003474261,16.3952338367634));
#28945=CARTESIAN_POINT('Ctrl Pts',(-2.67620879985039,0.480147146374683,
16.5223898341802));
#28946=CARTESIAN_POINT('Ctrl Pts',(-1.85261847329488,-1.99008532856633,
16.6495458315969));
#28947=CARTESIAN_POINT('Ctrl Pts',(0.670149623049134,-2.63505869105329,
16.7767018290136));
#28948=CARTESIAN_POINT('Ctrl Pts',(2.57827236292531,-0.863218654307199,
16.9038578264304));
#28949=CARTESIAN_POINT('Ctrl Pts',(2.12166477829421,1.70034508000999,17.0310138238472));
#28950=CARTESIAN_POINT('Ctrl Pts',(-0.280883472581658,2.70439259306019,
17.1581698212639));
#28951=CARTESIAN_POINT('Ctrl Pts',(-2.42581205735167,1.22803529467831,17.2853258186807));
#28952=CARTESIAN_POINT('Ctrl Pts',(-2.34584329765868,-1.37464688025626,
17.4124818160974));
#28953=CARTESIAN_POINT('Ctrl Pts',(-0.114322645200683,-2.71653550600074,
17.5396378135142));
#28954=CARTESIAN_POINT('Ctrl Pts',(2.22205202879955,-1.56688212826498,17.6667938109308));
#28955=CARTESIAN_POINT('Ctrl Pts',(2.52041322885733,1.01987841352257,17.7939498083476));
#28956=CARTESIAN_POINT('Ctrl Pts',(0.507111131323891,2.67123063831182,17.9211058057642));
#28957=CARTESIAN_POINT('Ctrl Pts',(-1.97130128092286,1.87259341086107,18.048261803181));
#28958=CARTESIAN_POINT('Ctrl Pts',(-2.64168286416546,-0.643542125849563,
18.1754178005977));
#28959=CARTESIAN_POINT('Ctrl Pts',(-0.889175513542436,-2.56943607211484,
18.3025737980144));
#28960=CARTESIAN_POINT('Ctrl Pts',(1.67886255094878,-2.13870413044678,18.4297297954312));
#28961=CARTESIAN_POINT('Ctrl Pts',(2.7070876608444,0.25359656754859,18.5568857928479));
#28962=CARTESIAN_POINT('Ctrl Pts',(1.25243610699023,2.41330450222833,18.6840417902647));
#28963=CARTESIAN_POINT('Ctrl Pts',(-1.35092017034292,2.35958672566386,18.8111977876814));
#28964=CARTESIAN_POINT('Ctrl Pts',(-2.71524447466377,0.141711909789787,
18.9383537850982));
#28965=CARTESIAN_POINT('Ctrl Pts',(-1.58921087885835,-2.20613771217634,
19.0655097825149));
#28966=CARTESIAN_POINT('Ctrl Pts',(0.994409282010079,-2.5305700943504,19.1926657799316));
#28967=CARTESIAN_POINT('Ctrl Pts',(2.66598080986571,-0.534023542548665,
19.3198217773484));
#28968=CARTESIAN_POINT('Ctrl Pts',(1.8923779037484,1.95231674990849,19.446977774765));
#28969=CARTESIAN_POINT('Ctrl Pts',(-0.616869179752904,2.64803837540913,
19.5741337721818));
#28970=CARTESIAN_POINT('Ctrl Pts',(-2.56033846700907,0.915041942711955,
19.7012897695985));
#28971=CARTESIAN_POINT('Ctrl Pts',(-2.15552597418617,-1.65720927983679,
19.8284457670153));
#28972=CARTESIAN_POINT('Ctrl Pts',(0.226283871483405,-2.70950741502488,
19.955601764432));
#28973=CARTESIAN_POINT('Ctrl Pts',(2.40055151155118,-1.27670954525991,20.0827577618488));
#28974=CARTESIAN_POINT('Ctrl Pts',(2.3730901812684,1.32705607045671,20.2099137592656));
#28975=CARTESIAN_POINT('Ctrl Pts',(0.169086762131636,2.71367730016675,20.3370697566822));
#28976=CARTESIAN_POINT('Ctrl Pts',(-2.18999902907526,1.61137800506825,20.4642257540991));
#28977=CARTESIAN_POINT('Ctrl Pts',(-2.54046959825811,-0.968839018049278,
20.5913817515157));
#28978=CARTESIAN_POINT('Ctrl Pts',(-0.560881643029023,-2.660459848425,20.7185377489324));
#28979=CARTESIAN_POINT('Ctrl Pts',(1.93313366626957,-1.91196993985354,20.8456937463493));
#28980=CARTESIAN_POINT('Ctrl Pts',(2.65412457842224,0.590133497425207,20.9728497437659));
#28981=CARTESIAN_POINT('Ctrl Pts',(0.940815311173381,2.55098047284375,21.1000057411826));
#28982=CARTESIAN_POINT('Ctrl Pts',(-1.63538746883388,2.17212859871361,21.2271617385995));
#28983=CARTESIAN_POINT('Ctrl Pts',(-2.71165160951022,-0.19894816211538,
21.3543177360161));
#28984=CARTESIAN_POINT('Ctrl Pts',(-1.30085314085368,-2.38755438231248,
21.4814737334328));
#28985=CARTESIAN_POINT('Ctrl Pts',(1.3030570076011,-2.38635229115696,21.6086297308496));
#28986=CARTESIAN_POINT('Ctrl Pts',(2.71183414189291,-0.196444418175644,
21.7357857282663));
#28987=CARTESIAN_POINT('Ctrl Pts',(1.63338125247519,2.17363762081699,21.8629417256831));
#28988=CARTESIAN_POINT('Ctrl Pts',(-0.94317022216235,2.55011073379072,21.9900977230998));
#28989=CARTESIAN_POINT('Ctrl Pts',(-2.65466831547712,0.58768270126854,22.1172537205165));
#28990=CARTESIAN_POINT('Ctrl Pts',(-1.9313675266463,-1.91375398094545,22.2444097179333));
#28991=CARTESIAN_POINT('Ctrl Pts',(0.56333779791293,-2.65994085423172,22.3715657153501));
#28992=CARTESIAN_POINT('Ctrl Pts',(2.5413630413366,-0.966492997748461,22.4987217127668));
#28993=CARTESIAN_POINT('Ctrl Pts',(2.18851031552501,1.61339933724078,22.6258777101835));
#28994=CARTESIAN_POINT('Ctrl Pts',(-0.171592219514319,2.71352002623355,
22.7530337076002));
#28995=CARTESIAN_POINT('Ctrl Pts',(-2.37431443633364,1.32486443834305,22.8801897050169));
#28996=CARTESIAN_POINT('Ctrl Pts',(-2.39937170655933,-1.27892542250552,
23.0073457024337));
#28997=CARTESIAN_POINT('Ctrl Pts',(-0.223782095619982,-2.70971518729337,
23.1345016998504));
#28998=CARTESIAN_POINT('Ctrl Pts',(2.15705515137361,-1.6552183833262,23.2616576972671));
#28999=CARTESIAN_POINT('Ctrl Pts',(2.55949252043483,0.91740550489222,23.3888136946838));
#29000=CARTESIAN_POINT('Ctrl Pts',(0.614423991571972,2.64860680002698,23.5159696921006));
#29001=CARTESIAN_POINT('Ctrl Pts',(-1.89417966487008,1.95056869137211,23.6431256895173));
#29002=CARTESIAN_POINT('Ctrl Pts',(-2.66548661131631,-0.536484806366303,
23.7702816869341));
#29003=CARTESIAN_POINT('Ctrl Pts',(-0.992072390990129,-2.53148715059024,
23.8974376843508));
#29004=CARTESIAN_POINT('Ctrl Pts',(1.59124712127312,-2.20466945858295,24.0245936817677));
#29005=CARTESIAN_POINT('Ctrl Pts',(2.71511247517501,0.14421882580776,24.1517496791844));
#29006=CARTESIAN_POINT('Ctrl Pts',(1.34874099575428,2.36083302013085,24.278905676601));
#29007=CARTESIAN_POINT('Ctrl Pts',(-1.25466376937707,2.41214710338757,24.4060616740178));
#29008=CARTESIAN_POINT('Ctrl Pts',(-2.70732065186799,0.251097014194625,
24.5332176714345));
#29009=CARTESIAN_POINT('Ctrl Pts',(-1.67688717676254,-2.14025330719935,
24.6603736688514));
#29010=CARTESIAN_POINT('Ctrl Pts',(0.89154748653726,-2.56861400405307,24.787529666268));
#29011=CARTESIAN_POINT('Ctrl Pts',(2.64227591853694,-0.641102794322506,
24.9146856636847));
#29012=CARTESIAN_POINT('Ctrl Pts',(1.96957148125265,1.87441270877163,25.0418416611014));
#29013=CARTESIAN_POINT('Ctrl Pts',(-0.509577253762257,2.67076128566679,
25.1689976585183));
#29014=CARTESIAN_POINT('Ctrl Pts',(-2.52135380499301,1.01755088944764,25.2961536559349));
#29015=CARTESIAN_POINT('Ctrl Pts',(-2.22060438448587,-1.5689330738341,25.4233096533516));
#29016=CARTESIAN_POINT('Ctrl Pts',(0.1168307648981,-2.71642879438091,25.5504656507684));
#29017=CARTESIAN_POINT('Ctrl Pts',(2.34711150477801,-1.37248038481687,25.6776216481851));
#29018=CARTESIAN_POINT('Ctrl Pts',(2.42467718237059,1.23027451565081,25.8047776456018));
#29019=CARTESIAN_POINT('Ctrl Pts',(0.278386395944303,2.7046507791435,25.9319336430186));
#29020=CARTESIAN_POINT('Ctrl Pts',(-2.12323379705904,1.69838542904567,26.0590896404354));
#29021=CARTESIAN_POINT('Ctrl Pts',(-2.57747425698115,-0.865598796884507,
26.1862456378521));
#29022=CARTESIAN_POINT('Ctrl Pts',(-0.667716396258505,-2.63567631486417,
26.3134016352688));
#29023=CARTESIAN_POINT('Ctrl Pts',(1.85445512296983,-1.98837396368473,26.4405576326856));
#29024=CARTESIAN_POINT('Ctrl Pts',(2.67576434084336,0.482617876626542,26.5677136301024));
#29025=CARTESIAN_POINT('Ctrl Pts',(1.04292590193155,2.51096403511652,26.694869627519));
#29026=CARTESIAN_POINT('Ctrl Pts',(-1.54645946428526,2.23631347263548,26.8220256249357));
#29027=CARTESIAN_POINT('Ctrl Pts',(-2.71746884998021,-0.0894308221792745,
26.9491816223525));
#29028=CARTESIAN_POINT('Ctrl Pts',(-1.39608019121057,-2.33315128576736,
27.0763376197693));
#29029=CARTESIAN_POINT('Ctrl Pts',(1.20576014173901,-2.4369606691865,27.2034936171861));
#29030=CARTESIAN_POINT('Ctrl Pts',(2.70170584064869,-0.305647465510764,
27.3306496146028));
#29031=CARTESIAN_POINT('Ctrl Pts',(1.71971095378114,2.10599835185442,27.4578056120194));
#29032=CARTESIAN_POINT('Ctrl Pts',(-0.839562074942459,2.58607237812223,
27.5849616094363));
#29033=CARTESIAN_POINT('Ctrl Pts',(-2.62880866019516,0.694262090749141,
27.7121176068529));
#29034=CARTESIAN_POINT('Ctrl Pts',(-2.00697422643644,-1.83430893717177,
27.8392736042696));
#29035=CARTESIAN_POINT('Ctrl Pts',(0.455609416755672,-2.68049526803014,
27.9664296016865));
#29036=CARTESIAN_POINT('Ctrl Pts',(2.50031889761113,-1.06819484777688,28.0935855991032));
#29037=CARTESIAN_POINT('Ctrl Pts',(2.25179512540124,1.52382857821593,28.22074159652));
#29038=CARTESIAN_POINT('Ctrl Pts',(-0.0620217842537382,2.71823253619818,
28.3478975939367));
#29039=CARTESIAN_POINT('Ctrl Pts',(-2.31895378286757,1.41953801481067,28.4750535913533));
#29040=CARTESIAN_POINT('Ctrl Pts',(-2.44899631459202,-1.18112314077876,
28.60220958877));
#29041=CARTESIAN_POINT('Ctrl Pts',(-0.332877450415083,-2.69848613588685,
28.7293655861868));
#29042=CARTESIAN_POINT('Ctrl Pts',(2.08854872444804,-1.74086158214111,28.8565215836035));
#29043=CARTESIAN_POINT('Ctrl Pts',(2.59440749303851,0.813439968672548,28.9836775810204));
#29044=CARTESIAN_POINT('Ctrl Pts',(0.720737178070014,2.62167365297744,29.110833578437));
#29045=CARTESIAN_POINT('Ctrl Pts',(-1.81397620026522,2.02537037784197,29.2379895758538));
#29046=CARTESIAN_POINT('Ctrl Pts',(-2.68495358608697,-0.428554620937766,
29.3651455732704));
#29047=CARTESIAN_POINT('Ctrl Pts',(-1.09335515710588,-2.48941947509823,
29.4923015706873));
#29048=CARTESIAN_POINT('Ctrl Pts',(1.50104271721046,-2.2670477682832,29.6194575681039));
#29049=CARTESIAN_POINT('Ctrl Pts',(2.71871977536715,0.0346064386488195,
29.7466135655207));
#29050=CARTESIAN_POINT('Ctrl Pts',(1.44285146993242,2.30452043997926,29.8737695629374));
#29051=CARTESIAN_POINT('Ctrl Pts',(-1.15636601837838,2.46078289454969,30.0009255603543));
#29052=CARTESIAN_POINT('Ctrl Pts',(-2.69499199230524,0.360073581339755,
30.1280815577708));
#29053=CARTESIAN_POINT('Ctrl Pts',(-1.76183516308499,-2.07088668948479,
30.2552375551877));
#29054=CARTESIAN_POINT('Ctrl Pts',(0.78723513471999,-2.60247875404054,30.3823935526044));
#29055=CARTESIAN_POINT('Ctrl Pts',(2.61427201884843,-0.747138965676931,
30.5095495500212));
#29056=CARTESIAN_POINT('Ctrl Pts',(2.04356054699407,1.79345898010954,30.6367055474379));
#29057=CARTESIAN_POINT('Ctrl Pts',(-0.401456240674143,2.68913884160025,
30.7638615448547));
#29058=CARTESIAN_POINT('Ctrl Pts',(-2.47826687605908,1.11840427108543,30.8910175422714));
#29059=CARTESIAN_POINT('Ctrl Pts',(-2.28206985007429,-1.47810419860748,
31.018173539688));
#29060=CARTESIAN_POINT('Ctrl Pts',(0.00718757353821803,-2.7189305179477,
31.1453295371049));
#29061=CARTESIAN_POINT('Ctrl Pts',(2.2898527249793,-1.46601818554802,31.2724855345215));
#29062=CARTESIAN_POINT('Ctrl Pts',(2.47231921036929,1.13149129231446,31.3996415319384));
#29063=CARTESIAN_POINT('Ctrl Pts',(0.38723309237749,2.69122376535401,31.5267975293551));
#29064=CARTESIAN_POINT('Ctrl Pts',(-2.05301404314954,1.78262956340224,31.6539535267717));
#29065=CARTESIAN_POINT('Ctrl Pts',(-2.61028534039153,-0.760950237808461,
31.7811095241884));
#29066=CARTESIAN_POINT('Ctrl Pts',(-0.77346476825431,-2.60660451120056,
31.9082655216052));
#29067=CARTESIAN_POINT('Ctrl Pts',(1.77275936289528,-2.06154288271629,32.035421519022));
#29068=CARTESIAN_POINT('Ctrl Pts',(2.69305060974847,0.374317029576794,32.1625775164387));
#29069=CARTESIAN_POINT('Ctrl Pts',(1.14333964062519,2.4668622391498,32.2897335138555));
#29070=CARTESIAN_POINT('Ctrl Pts',(-1.45501535228521,2.29685983457637,32.4168895112722));
#29071=CARTESIAN_POINT('Ctrl Pts',(-2.71886474821264,0.0202320386364921,
32.544045508689));
#29072=CARTESIAN_POINT('Ctrl Pts',(-1.48903579470102,-2.27495216025588,
32.6712015061057));
#29073=CARTESIAN_POINT('Ctrl Pts',(1.10650147163388,-2.48360403032979,32.7983575035225));
#29074=CARTESIAN_POINT('Ctrl Pts',(2.68718187780354,-0.414353332843636,
32.925513500939));
#29075=CARTESIAN_POINT('Ctrl Pts',(1.80324259290189,2.0349328156185,33.0526694983558));
#29076=CARTESIAN_POINT('Ctrl Pts',(-0.734587807428301,2.61782605300257,
33.1798254957725));
#29077=CARTESIAN_POINT('Ctrl Pts',(-2.59867218381255,0.799712680864083,
33.3069814931893));
#29078=CARTESIAN_POINT('Ctrl Pts',(-2.07931503383186,-1.75188092642428,
33.434137490606));
#29079=CARTESIAN_POINT('Ctrl Pts',(0.347138751858806,-2.69668568512338,
33.5612934880228));
#29080=CARTESIAN_POINT('Ctrl Pts',(2.4552086228712,-1.16816408243671,33.6884494854395));
#29081=CARTESIAN_POINT('Ctrl Pts',(2.31141259786826,1.43178873129245,33.8156054828562));
#29082=CARTESIAN_POINT('Ctrl Pts',(0.0476565103776217,2.71850301715689,
33.9427614802729));
#29083=CARTESIAN_POINT('Ctrl Pts',(-2.25983341822314,1.51193904894985,34.0699174776897));
#29084=CARTESIAN_POINT('Ctrl Pts',(-2.49461112273393,-1.08146981546886,
34.1970734751064));
#29085=CARTESIAN_POINT('Ctrl Pts',(-0.441479368245401,-2.68273191178327,
34.3242294725231));
#29086=CARTESIAN_POINT('Ctrl Pts',(2.01673602906685,-1.82392925374997,34.4513854699399));
#29087=CARTESIAN_POINT('Ctrl Pts',(2.62492622075604,0.708641089121424,34.5785414673567));
#29088=CARTESIAN_POINT('Ctrl Pts',(0.826212131065567,2.58953704692221,34.7056974647735));
#29089=CARTESIAN_POINT('Ctrl Pts',(-1.73146372505156,2.09869585167041,34.8328534621901));
#29090=CARTESIAN_POINT('Ctrl Pts',(-2.69884412682198,-0.323811118765491,
34.9600172221939));
#29091=CARTESIAN_POINT('Ctrl Pts',(-1.69656210721047,-1.73082272675162,
35.0447956497254));
#29092=CARTESIAN_POINT('Ctrl Pts',(-1.00847442622808,-2.06659007601517,
35.0871887447847));
#29093=CARTESIAN_POINT('Ctrl Pts',(1.24723527089883,-1.74554912134441,4.91299708530798));
#29094=CARTESIAN_POINT('Ctrl Pts',(1.82857496528105,-1.33019696843275,4.95539991266972));
#29095=CARTESIAN_POINT('Ctrl Pts',(2.53322632354395,0.119575258569398,5.04018807250373));
#29096=CARTESIAN_POINT('Ctrl Pts',(1.26822303545749,2.19881126114289,5.16736156480996));
#29097=CARTESIAN_POINT('Ctrl Pts',(-1.16087552561943,2.25459568666643,5.2945175622267));
#29098=CARTESIAN_POINT('Ctrl Pts',(-2.52467584330113,0.245759892176623,
5.42167355964344));
#29099=CARTESIAN_POINT('Ctrl Pts',(-1.57320286650264,-1.99016393268508,
5.54882955706016));
#29100=CARTESIAN_POINT('Ctrl Pts',(0.821331662733299,-2.39987583645184,
5.67598555447692));
#29101=CARTESIAN_POINT('Ctrl Pts',(2.46247781576393,-0.608940207530322,
5.80314155189363));
#29102=CARTESIAN_POINT('Ctrl Pts',(1.84514089848384,1.74074310964657,5.93029754931038));
#29103=CARTESIAN_POINT('Ctrl Pts',(-0.46453821390252,2.49373107655781,6.05745354672711));
#29104=CARTESIAN_POINT('Ctrl Pts',(-2.34814198676975,0.95959460444983,6.18460954414384));
#29105=CARTESIAN_POINT('Ctrl Pts',(-2.07809180336199,-1.45469424707903,
6.31176554156058));
#29106=CARTESIAN_POINT('Ctrl Pts',(0.0979382188879125,-2.53475367241525,
6.43892153897732));
#29107=CARTESIAN_POINT('Ctrl Pts',(2.18413991054886,-1.29000669886218,6.56607753639405));
#29108=CARTESIAN_POINT('Ctrl Pts',(2.26710112530366,1.13790889748749,6.69323353381079));
#29109=CARTESIAN_POINT('Ctrl Pts',(0.270730429855875,2.522158768484,6.82038953122753));
#29110=CARTESIAN_POINT('Ctrl Pts',(-1.97394755373906,1.59314576162754,6.94754552864427));
#29111=CARTESIAN_POINT('Ctrl Pts',(-2.40816773953772,-0.797063519219258,
7.074701526061));
#29112=CARTESIAN_POINT('Ctrl Pts',(-0.633673462972628,-2.45622464330757,
7.20185752347775));
#29113=CARTESIAN_POINT('Ctrl Pts',(1.72201106451603,-1.86259491985669,7.32901352089446));
#29114=CARTESIAN_POINT('Ctrl Pts',(2.49830786182965,0.439362838806997,7.45616951831122));
#29115=CARTESIAN_POINT('Ctrl Pts',(0.983215870614292,2.33834735642068,7.58332551572794));
#29116=CARTESIAN_POINT('Ctrl Pts',(-1.43365841672741,2.09265510986232,7.71048151314468));
#29117=CARTESIAN_POINT('Ctrl Pts',(-2.53561517448838,-0.0723708375318783,
7.83763751056142));
#29118=CARTESIAN_POINT('Ctrl Pts',(-1.31196576888435,-2.17101995946912,
7.96479350797814));
#29119=CARTESIAN_POINT('Ctrl Pts',(1.11498755491276,-2.27846101652471,8.09194950539489));
#29120=CARTESIAN_POINT('Ctrl Pts',(2.51930071103104,-0.296151610402521,
8.21910550281162));
#29121=CARTESIAN_POINT('Ctrl Pts',(1.61297094434476,1.95778103494126,8.34626150022837));
#29122=CARTESIAN_POINT('Ctrl Pts',(-0.772737556416206,2.41608330116289,
8.47341749764509));
#29123=CARTESIAN_POINT('Ctrl Pts',(-2.44970947888779,0.658411207279792,
8.60057349506184));
#29124=CARTESIAN_POINT('Ctrl Pts',(-1.87986590803327,-1.70314004607919,
8.72772949247856));
#29125=CARTESIAN_POINT('Ctrl Pts',(0.414146134165366,-2.50261160160021,
8.85488548989531));
#29126=CARTESIAN_POINT('Ctrl Pts',(2.32831315444159,-1.00674709023239,8.98204148731205));
#29127=CARTESIAN_POINT('Ctrl Pts',(2.1070065139672,1.41248199950732,9.10919748472876));
#29128=CARTESIAN_POINT('Ctrl Pts',(-0.0467965800058906,2.53621606511637,
9.23635348214553));
#29129=CARTESIAN_POINT('Ctrl Pts',(-2.15767895954577,1.33379284612595,9.36350947956224));
#29130=CARTESIAN_POINT('Ctrl Pts',(-2.28958931907699,-1.09195356989761,
9.49066547697899));
#29131=CARTESIAN_POINT('Ctrl Pts',(-0.321542602178368,-2.51618604316749,
9.61782147439571));
#29132=CARTESIAN_POINT('Ctrl Pts',(1.94141537115939,-1.6326322934056,9.74497747181245));
#29133=CARTESIAN_POINT('Ctrl Pts',(2.42375316384388,0.748333114062007,9.8721334692292));
#29134=CARTESIAN_POINT('Ctrl Pts',(0.68308198040958,2.44294511949922,9.99928946664592));
#29135=CARTESIAN_POINT('Ctrl Pts',(-1.68409581125844,1.8969457418036,10.1264454640627));
#29136=CARTESIAN_POINT('Ctrl Pts',(-2.50666082596597,-0.388887326114794,
10.2536014614794));
#29137=CARTESIAN_POINT('Ctrl Pts',(-1.03017592117983,-2.31804215239206,
10.3807574588962));
#29138=CARTESIAN_POINT('Ctrl Pts',(1.39116193064996,-2.1211436376529,10.5079134563129));
#29139=CARTESIAN_POINT('Ctrl Pts',(2.53655902035812,0.021217565482156,10.6350694537296));
#29140=CARTESIAN_POINT('Ctrl Pts',(1.35548427505125,2.14411852026279,10.7622254511464));
#29141=CARTESIAN_POINT('Ctrl Pts',(-1.06880853196949,2.3004847686595,10.8893814485631));
#29142=CARTESIAN_POINT('Ctrl Pts',(-2.51281547664917,0.346900892413839,
11.0165374459798));
#29143=CARTESIAN_POINT('Ctrl Pts',(-1.65212760205011,-1.92485226326314,
11.1436934433966));
#29144=CARTESIAN_POINT('Ctrl Pts',(0.723852565443357,-2.4311765284212,11.2708494408133));
#29145=CARTESIAN_POINT('Ctrl Pts',(2.43593231008385,-0.707683283351195,
11.39800543823));
#29146=CARTESIAN_POINT('Ctrl Pts',(1.91383265423357,1.66488030213418,11.5251614356468));
#29147=CARTESIAN_POINT('Ctrl Pts',(-0.363588967820266,2.51045512035657,
11.6523174330635));
#29148=CARTESIAN_POINT('Ctrl Pts',(-2.30753540306903,1.05349998216809,11.7794734304802));
#29149=CARTESIAN_POINT('Ctrl Pts',(-2.13506503884503,-1.36970037918765,
11.906629427897));
#29150=CARTESIAN_POINT('Ctrl Pts',(-0.00436360689018303,-2.53664400493645,
12.0337854253137));
#29151=CARTESIAN_POINT('Ctrl Pts',(2.1303400219178,-1.37703784982852,12.1609414227305));
#29152=CARTESIAN_POINT('Ctrl Pts',(2.31114625657121,1.04555479511216,12.2880974201472));
#29153=CARTESIAN_POINT('Ctrl Pts',(0.372223902471257,2.50918935420869,12.4152534175639));
#29154=CARTESIAN_POINT('Ctrl Pts',(-1.90809339590896,1.6714548876155,12.5424094149807));
#29155=CARTESIAN_POINT('Ctrl Pts',(-2.43835263984122,-0.699298400273082,
12.6695654123974));
#29156=CARTESIAN_POINT('Ctrl Pts',(-0.732212614173908,-2.42867176384331,
12.7967214098141));
#29157=CARTESIAN_POINT('Ctrl Pts',(1.64549547296818,-1.93052492791114,12.9238774072309));
#29158=CARTESIAN_POINT('Ctrl Pts',(2.51399409887539,0.338253632153168,13.0510334046476));
#29159=CARTESIAN_POINT('Ctrl Pts',(1.07671690112295,2.29679397501851,13.1781894020643));
#29160=CARTESIAN_POINT('Ctrl Pts',(-1.34809952778586,2.14876930172335,13.3053453994811));
#29161=CARTESIAN_POINT('Ctrl Pts',(-2.53647101020647,0.02994433547918,13.4325013968978));
#29162=CARTESIAN_POINT('Ctrl Pts',(-1.39845137843795,-2.11634486579813,
13.5596573943146));
#29163=CARTESIAN_POINT('Ctrl Pts',(1.02219472425514,-2.3215726985279,13.6868133917313));
#29164=CARTESIAN_POINT('Ctrl Pts',(2.50530804462615,-0.397509056974356,
13.813969389148));
#29165=CARTESIAN_POINT('Ctrl Pts',(1.69061218449704,1.89114047349086,13.9411253865648));
#29166=CARTESIAN_POINT('Ctrl Pts',(-0.674673115735156,2.44528076828599,
14.0682813839815));
#29167=CARTESIAN_POINT('Ctrl Pts',(-2.4211642191826,0.756667478219514,14.1954373813982));
#29168=CARTESIAN_POINT('Ctrl Pts',(-1.9470208652149,-1.62594329521757,14.322593378815));
#29169=CARTESIAN_POINT('Ctrl Pts',(0.312883895743237,-2.51727740160469,
14.4497493762317));
#29170=CARTESIAN_POINT('Ctrl Pts',(2.28581896065478,-1.09982431685984,14.5769053736484));
#29171=CARTESIAN_POINT('Ctrl Pts',(2.16225503255025,1.32636157327338,14.7040613710652));
#29172=CARTESIAN_POINT('Ctrl Pts',(0.0555220186984494,2.53604005376192,
14.8312173684819));
#29173=CARTESIAN_POINT('Ctrl Pts',(-2.10213447522553,1.41972268310166,14.9583733658987));
#29174=CARTESIAN_POINT('Ctrl Pts',(-2.33176303414969,-0.998730695141672,
15.0855293633154));
#29175=CARTESIAN_POINT('Ctrl Pts',(-0.42275378439691,-2.50117194263474,
15.2126853607321));
#29176=CARTESIAN_POINT('Ctrl Pts',(1.87399522013853,-1.70959754437793,15.3398413581488));
#29177=CARTESIAN_POINT('Ctrl Pts',(2.45196020915775,0.649979216246355,15.4669973555656));
#29178=CARTESIAN_POINT('Ctrl Pts',(0.781045388403149,2.41341043962673,15.5941533529823));
#29179=CARTESIAN_POINT('Ctrl Pts',(-1.60622575735892,1.96331878849104,15.7213093503991));
#29180=CARTESIAN_POINT('Ctrl Pts',(-2.52030469462918,-0.287482338718793,
15.8484653478158));
#29181=CARTESIAN_POINT('Ctrl Pts',(-1.12281987933079,-2.27461147614811,
15.9756213452325));
#29182=CARTESIAN_POINT('Ctrl Pts',(1.30448872642261,-2.17552085981299,16.1027773426493));
#29183=CARTESIAN_POINT('Ctrl Pts',(2.53535117943153,-0.0810940552712092,
16.229933340066));
#29184=CARTESIAN_POINT('Ctrl Pts',(1.44084960050602,2.08771029541141,16.3570893374828));
#29185=CARTESIAN_POINT('Ctrl Pts',(-0.975165094087748,2.34171622706894,
16.4842453348995));
#29186=CARTESIAN_POINT('Ctrl Pts',(-2.4967814688803,0.447955517324072,16.6114013323162));
#29187=CARTESIAN_POINT('Ctrl Pts',(-1.72840903642746,-1.85665937954192,
16.738557329733));
#29188=CARTESIAN_POINT('Ctrl Pts',(0.625219213201751,-2.45839028315044,
16.8657133271497));
#29189=CARTESIAN_POINT('Ctrl Pts',(2.4054112137431,-0.805343865466191,16.9928693245664));
#29190=CARTESIAN_POINT('Ctrl Pts',(1.97941704022394,1.58634486468619,17.1200253219832));
#29191=CARTESIAN_POINT('Ctrl Pts',(-0.2620515444444,2.52307567007005,17.2471813193999));
#29192=CARTESIAN_POINT('Ctrl Pts',(-2.26317266131126,1.14570124986335,17.3743373168166));
#29193=CARTESIAN_POINT('Ctrl Pts',(-2.18856543436326,-1.28248321172463,
17.5014933142334));
#29194=CARTESIAN_POINT('Ctrl Pts',(-0.106657844494999,-2.53440445727449,
17.6286493116501));
#29195=CARTESIAN_POINT('Ctrl Pts',(2.07307379330966,-1.46182998202179,17.7558053090668));
#29196=CARTESIAN_POINT('Ctrl Pts',(2.35143126503568,0.9515003177392,17.8829613064836));
#29197=CARTESIAN_POINT('Ctrl Pts',(0.473111692713715,2.49213706987852,18.0101173039003));
#29198=CARTESIAN_POINT('Ctrl Pts',(-1.83913471477385,1.74704474749757,18.137273301317));
#29199=CARTESIAN_POINT('Ctrl Pts',(-2.46457033631895,-0.600395624719085,
18.2644292987338));
#29200=CARTESIAN_POINT('Ctrl Pts',(-0.829560438228563,-2.39716735506121,
18.3915852961505));
#29201=CARTESIAN_POINT('Ctrl Pts',(1.56630263910659,-1.99531398320486,18.5187412935673));
#29202=CARTESIAN_POINT('Ctrl Pts',(2.52559004611624,0.236594099257959,18.645897290984));
#29203=CARTESIAN_POINT('Ctrl Pts',(1.16846610139864,2.25150367948342,18.7730532884007));
#29204=CARTESIAN_POINT('Ctrl Pts',(-1.26034726716289,2.20138742955441,18.9002092858175));
#29205=CARTESIAN_POINT('Ctrl Pts',(-2.53319998357345,0.132210786506162,
19.0273652832342));
#29206=CARTESIAN_POINT('Ctrl Pts',(-1.48266169392256,-2.05822645746765,
19.1545212806509));
#29207=CARTESIAN_POINT('Ctrl Pts',(0.927738772828189,-2.36090716002057,
19.2816772780677));
#29208=CARTESIAN_POINT('Ctrl Pts',(2.48723921796958,-0.498219752156858,
19.4088332754844));
#29209=CARTESIAN_POINT('Ctrl Pts',(1.76550278231721,1.82142300811078,19.5359892729011));
#29210=CARTESIAN_POINT('Ctrl Pts',(-0.57551097538294,2.47049974014549,19.6631452703179));
#29211=CARTESIAN_POINT('Ctrl Pts',(-2.38867970198999,0.853692643839789,
19.7903012677346));
#29212=CARTESIAN_POINT('Ctrl Pts',(-2.01100800069828,-1.54610111893518,
19.9174572651514));
#29213=CARTESIAN_POINT('Ctrl Pts',(0.211112592207941,-2.52784756705311,
20.0446132625681));
#29214=CARTESIAN_POINT('Ctrl Pts',(2.2396057174121,-1.19111211872777,20.1717692599848));
#29215=CARTESIAN_POINT('Ctrl Pts',(2.21398554137631,1.23808314398582,20.2989252574016));
#29216=CARTESIAN_POINT('Ctrl Pts',(0.157750282544093,2.53173788082463,20.4260812548183));
#29217=CARTESIAN_POINT('Ctrl Pts',(-2.04316979787472,1.50334261760173,20.553237252235));
#29218=CARTESIAN_POINT('Ctrl Pts',(-2.37014294831528,-0.903882875928337,
20.6803932496518));
#29219=CARTESIAN_POINT('Ctrl Pts',(-0.523277142137953,-2.48208841127005,
20.8075492470685));
#29220=CARTESIAN_POINT('Ctrl Pts',(1.80352606085155,-1.78378126368521,20.9347052444853));
#29221=CARTESIAN_POINT('Ctrl Pts',(2.47617789160356,0.550567795987747,21.061861241902));
#29222=CARTESIAN_POINT('Ctrl Pts',(0.877738028029808,2.37994911773245,21.1890172393187));
#29223=CARTESIAN_POINT('Ctrl Pts',(-1.52574235868728,2.02649749660654,21.3161732367354));
#29224=CARTESIAN_POINT('Ctrl Pts',(-2.52984800328848,-0.185609614789812,
21.4433292341522));
#29225=CARTESIAN_POINT('Ctrl Pts',(-1.21363699872742,-2.2274799851323,21.5704852315689));
#29226=CARTESIAN_POINT('Ctrl Pts',(1.21569310647764,-2.22635848858801,21.6976412289857));
#29227=CARTESIAN_POINT('Ctrl Pts',(2.53001829772536,-0.183273735215835,
21.8247972264024));
#29228=CARTESIAN_POINT('Ctrl Pts',(1.52387064978812,2.0279053458087,21.9519532238192));
#29229=CARTESIAN_POINT('Ctrl Pts',(-0.879935053208925,2.37913769063065,
22.0791092212358));
#29230=CARTESIAN_POINT('Ctrl Pts',(-2.47668517362228,0.548281314294679,
22.2062652186526));
#29231=CARTESIAN_POINT('Ctrl Pts',(-1.80187833266125,-1.78544569313408,
22.3334212160693));
#29232=CARTESIAN_POINT('Ctrl Pts',(0.525568623280569,-2.48160421321936,
22.4605772134861));
#29233=CARTESIAN_POINT('Ctrl Pts',(2.37097649019807,-0.901694145358155,
22.5877332109028));
#29234=CARTESIAN_POINT('Ctrl Pts',(2.04178089563184,1.50522842886984,22.7148892083196));
#29235=CARTESIAN_POINT('Ctrl Pts',(-0.16008776068265,2.5315911513759,22.8420452057363));
#29236=CARTESIAN_POINT('Ctrl Pts',(-2.21512771584346,1.23603845059418,22.969201203153));
#29237=CARTESIAN_POINT('Ctrl Pts',(-2.23850501284805,-1.19317943172823,
23.0963572005698));
#29238=CARTESIAN_POINT('Ctrl Pts',(-0.208778548759929,-2.52804140915904,
23.2235131979865));
#29239=CARTESIAN_POINT('Ctrl Pts',(2.01243465368002,-1.54424370275967,23.3506691954032));
#29240=CARTESIAN_POINT('Ctrl Pts',(2.38789047219213,0.855897740188131,23.47782519282));
#29241=CARTESIAN_POINT('Ctrl Pts',(0.57322972567696,2.47103005454111,23.6049811902367));
#29242=CARTESIAN_POINT('Ctrl Pts',(-1.76718374375042,1.81979214875473,23.7321371876534));
#29243=CARTESIAN_POINT('Ctrl Pts',(-2.48677815313036,-0.500515999702998,
23.8592931850702));
#29244=CARTESIAN_POINT('Ctrl Pts',(-0.925558559463123,-2.36176273191226,
23.9864491824869));
#29245=CARTESIAN_POINT('Ctrl Pts',(1.48456141577064,-2.05685664343682,24.1136051799036));
#29246=CARTESIAN_POINT('Ctrl Pts',(2.53307683403542,0.134549625485303,24.2407611773204));
#29247=CARTESIAN_POINT('Ctrl Pts',(1.25831419607725,2.20255016578411,24.3679171747371));
#29248=CARTESIAN_POINT('Ctrl Pts',(-1.17054440940153,2.25042387884239,24.4950731721539));
#29249=CARTESIAN_POINT('Ctrl Pts',(-2.52580741617726,0.234262129310505,
24.6222291695706));
#29250=CARTESIAN_POINT('Ctrl Pts',(-1.5644597045559,-1.99675929487407,24.7493851669873));
#29251=CARTESIAN_POINT('Ctrl Pts',(0.83177338148554,-2.39640040283281,24.8765411644041));
#29252=CARTESIAN_POINT('Ctrl Pts',(2.46512362915797,-0.598119839005628,
25.0036971618208));
#29253=CARTESIAN_POINT('Ctrl Pts',(1.83752089011209,1.74874206995966,25.1308531592375));
#29254=CARTESIAN_POINT('Ctrl Pts',(-0.475412473132706,2.49169918514153,
25.2580091566543));
#29255=CARTESIAN_POINT('Ctrl Pts',(-2.35230877992377,0.949328843309133,
25.385165154071));
#29256=CARTESIAN_POINT('Ctrl Pts',(-2.07172320680237,-1.46374342124623,
25.5123211514877));
#29257=CARTESIAN_POINT('Ctrl Pts',(0.108997806452491,-2.53430490017158,
25.6394771489045));
#29258=CARTESIAN_POINT('Ctrl Pts',(2.18974861410406,-1.28046196971035,25.7666331463212));
#29259=CARTESIAN_POINT('Ctrl Pts',(2.26211387441007,1.14779034150259,25.893789143738));
#29260=CARTESIAN_POINT('Ctrl Pts',(0.259721885161245,2.5233165459794,26.0209451411547));
#29261=CARTESIAN_POINT('Ctrl Pts',(-1.98088086359093,1.58451659918865,26.1481011385715));
#29262=CARTESIAN_POINT('Ctrl Pts',(-2.40466661708398,-0.807564430573208,
26.2752571359881));
#29263=CARTESIAN_POINT('Ctrl Pts',(-0.622949122930586,-2.45896649816241,
26.4024131334049));
#29264=CARTESIAN_POINT('Ctrl Pts',(1.73012254729899,-1.85506275370209,26.5295691308216));
#29265=CARTESIAN_POINT('Ctrl Pts',(2.49636680877887,0.450260596624125,26.6567251282384));
#29266=CARTESIAN_POINT('Ctrl Pts',(0.973002579433895,2.34261559570924,26.7838811256551));
#29267=CARTESIAN_POINT('Ctrl Pts',(-1.44277656250804,2.08637907378373,26.9110371230718));
#29268=CARTESIAN_POINT('Ctrl Pts',(-2.53527522488879,-0.0834349022304562,
27.0381931204886));
#29269=CARTESIAN_POINT('Ctrl Pts',(-1.30247951904217,-2.17672436273424,
27.1653491179053));
#29270=CARTESIAN_POINT('Ctrl Pts',(1.12491954214358,-2.27357381066651,27.2925051153221));
#29271=CARTESIAN_POINT('Ctrl Pts',(2.52056905188954,-0.285155227028738,
27.4196611127388));
#29272=CARTESIAN_POINT('Ctrl Pts',(1.60441234685104,1.96480097468346,27.5468171101555));
#29273=CARTESIAN_POINT('Ctrl Pts',(-0.783273349526421,2.41268827426315,
27.6739731075723));
#29274=CARTESIAN_POINT('Ctrl Pts',(-2.45255928774101,0.647715052287995,
27.801129104989));
#29275=CARTESIAN_POINT('Ctrl Pts',(-1.87241595549912,-1.71132706939307,
27.9282851024057));
#29276=CARTESIAN_POINT('Ctrl Pts',(0.425062928149098,-2.50078054934024,
28.0554410998225));
#29277=CARTESIAN_POINT('Ctrl Pts',(2.33268416507548,-0.996577360194006,
28.1825970972391));
#29278=CARTESIAN_POINT('Ctrl Pts',(2.10082275386406,1.42166297190725,28.309753094656));
#29279=CARTESIAN_POINT('Ctrl Pts',(-0.0578635125929414,2.53598770950404,
28.4369090920726));
#29280=CARTESIAN_POINT('Ctrl Pts',(-2.16347873625452,1.32436460486516,28.5640650894894));
#29281=CARTESIAN_POINT('Ctrl Pts',(-2.28480252212436,-1.10193433730837,
28.6912210869062));
#29282=CARTESIAN_POINT('Ctrl Pts',(-0.310559568315866,-2.51756521333065,
28.8183770843229));
#29283=CARTESIAN_POINT('Ctrl Pts',(1.94852126349294,-1.62414492412501,28.9455330817396));
#29284=CARTESIAN_POINT('Ctrl Pts',(2.42046455855946,0.758902608773127,29.0726890791563));
#29285=CARTESIAN_POINT('Ctrl Pts',(0.672415108357407,2.44590264951363,29.1998450765731));
#29286=CARTESIAN_POINT('Ctrl Pts',(-1.6923575477613,1.88957873066472,29.3270010739898));
#29287=CARTESIAN_POINT('Ctrl Pts',(-2.50493995794367,-0.39982203033639,
29.4541570714066));
#29288=CARTESIAN_POINT('Ctrl Pts',(-1.02005078801005,-2.32251549805921,
29.5813130688233));
#29289=CARTESIAN_POINT('Ctrl Pts',(1.40040479671775,-2.11505277810627,29.70846906624));
#29290=CARTESIAN_POINT('Ctrl Pts',(2.53644228155689,0.0322862381765574,
29.8356250636568));
#29291=CARTESIAN_POINT('Ctrl Pts',(1.34611500144365,2.15001308175867,29.9627810610735));
#29292=CARTESIAN_POINT('Ctrl Pts',(-1.07883706461593,2.29579886681221,30.0899370584902));
#29293=CARTESIAN_POINT('Ctrl Pts',(-2.51430533579618,0.335932325374936,
30.217093055907));
#29294=CARTESIAN_POINT('Ctrl Pts',(-1.64371232418725,-1.93204338568256,
30.3442490533237));
#29295=CARTESIAN_POINT('Ctrl Pts',(0.734454686842863,-2.42799467911713,
30.4714050507405));
#29296=CARTESIAN_POINT('Ctrl Pts',(2.43899726046709,-0.697046779117154,
30.5985610481571));
#29297=CARTESIAN_POINT('Ctrl Pts',(1.90654933372726,1.6732159116227,30.725717045574));
#29298=CARTESIAN_POINT('Ctrl Pts',(-0.374540470211985,2.50884461157482,
30.8528730429906));
#29299=CARTESIAN_POINT('Ctrl Pts',(-2.31211062882314,1.04342047560674,30.9800290404074));
#29300=CARTESIAN_POINT('Ctrl Pts',(-2.12906769930454,-1.37900419891136,
31.1071850378241));
#29301=CARTESIAN_POINT('Ctrl Pts',(0.0067056802209494,-2.53663889482931,
31.2343410352408));
#29302=CARTESIAN_POINT('Ctrl Pts',(2.13632876870929,-1.36772849671617,31.3614970326576));
#29303=CARTESIAN_POINT('Ctrl Pts',(2.30656172640638,1.05563007303765,31.4886530300743));
#29304=CARTESIAN_POINT('Ctrl Pts',(0.361270917739877,2.51078975090502,31.6158090274911));
#29305=CARTESIAN_POINT('Ctrl Pts',(-1.91536901701141,1.66311255684901,31.7429650249078));
#29306=CARTESIAN_POINT('Ctrl Pts',(-2.43527787022593,-0.709932069801992,
31.8701210223245));
#29307=CARTESIAN_POINT('Ctrl Pts',(-0.721607559289571,-2.43184382348237,
31.9972770197413));
#29308=CARTESIAN_POINT('Ctrl Pts',(1.65390410729847,-1.92332603762306,32.124433017158));
#29309=CARTESIAN_POINT('Ctrl Pts',(2.51249411389452,0.349220816771008,32.2515890145748));
#29310=CARTESIAN_POINT('Ctrl Pts',(1.06668404479837,2.30147061968187,32.3787450119915));
#29311=CARTESIAN_POINT('Ctrl Pts',(-1.35746335215886,2.14286608425562,32.5059010094083));
#29312=CARTESIAN_POINT('Ctrl Pts',(-2.53657753464855,0.0188755747115968,
32.6330570068249));
#29313=CARTESIAN_POINT('Ctrl Pts',(-1.38920288241969,-2.12242721742547,
32.7602130042417));
#29314=CARTESIAN_POINT('Ctrl Pts',(1.03231570340048,-2.31708995176706,32.8873690016584));
#29315=CARTESIAN_POINT('Ctrl Pts',(2.50701885308274,-0.386572872442074,
33.0145249990751));
#29316=CARTESIAN_POINT('Ctrl Pts',(1.68234357876146,1.89850005154182,33.1416809964919));
#29317=CARTESIAN_POINT('Ctrl Pts',(-0.685337117550317,2.44231301319027,
33.2688369939086));
#29318=CARTESIAN_POINT('Ctrl Pts',(-2.42444332168722,0.746095671653793,
33.3959929913254));
#29319=CARTESIAN_POINT('Ctrl Pts',(-1.93990664881079,-1.63442547271552,
33.5231489887421));
#29320=CARTESIAN_POINT('Ctrl Pts',(0.323864715944294,-2.51588547440217,
33.6503049861589));
#29321=CARTESIAN_POINT('Ctrl Pts',(2.29059832407793,-1.08984412344908,33.7774609835755));
#29322=CARTESIAN_POINT('Ctrl Pts',(2.1564431525734,1.3357939678856,33.9046169809924));
#29323=CARTESIAN_POINT('Ctrl Pts',(0.0444613633992766,2.5362400559747,34.031772978409));
#29324=CARTESIAN_POINT('Ctrl Pts',(-2.1083221166044,1.41057058018255,34.1589289758258));
#29325=CARTESIAN_POINT('Ctrl Pts',(-2.32735906991002,-1.00896230315321,
34.2860849732425));
#29326=CARTESIAN_POINT('Ctrl Pts',(-0.411880233556468,-2.50286723655074,
34.4132409706593));
#29327=CARTESIAN_POINT('Ctrl Pts',(1.88152327474552,-1.70164329538349,34.540396968076));
#29328=CARTESIAN_POINT('Ctrl Pts',(2.44893714777715,0.661130005814309,34.6675529654928));
#29329=CARTESIAN_POINT('Ctrl Pts',(0.77081845718618,2.41592065316272,34.7947089629094));
#29330=CARTESIAN_POINT('Ctrl Pts',(-1.6153771495665,1.95798807311286,34.9218649603262));
#29331=CARTESIAN_POINT('Ctrl Pts',(-2.51789920264154,-0.302101091961186,
35.0490287203299));
#29332=CARTESIAN_POINT('Ctrl Pts',(-1.58281552258723,-1.61477912721602,
35.1338071478614));
#29333=CARTESIAN_POINT('Ctrl Pts',(-0.940860914659138,-1.9280348401272,
35.1762002429208));
#29334=CARTESIAN_POINT('Ctrl Pts',(1.1576046410105,-1.62010793883659,5.002008583444));
#29335=CARTESIAN_POINT('Ctrl Pts',(1.69716725916479,-1.23460442471794,5.04441141080575));
#29336=CARTESIAN_POINT('Ctrl Pts',(2.35117993957248,0.110982167919405,5.12919957063975));
#29337=CARTESIAN_POINT('Ctrl Pts',(1.17708415239424,2.04079709738398,5.25637306294598));
#29338=CARTESIAN_POINT('Ctrl Pts',(-1.07745100499292,2.09257266161708,5.38352906036272));
#29339=CARTESIAN_POINT('Ctrl Pts',(-2.34324392634153,0.228098738382345,
5.51068505777945));
#29340=CARTESIAN_POINT('Ctrl Pts',(-1.46014708051209,-1.8471438858426,5.63784105519619));
#29341=CARTESIAN_POINT('Ctrl Pts',(0.762307935618055,-2.22741247858047,
5.76499705261293));
#29342=CARTESIAN_POINT('Ctrl Pts',(2.28551566366429,-0.565179663197865,
5.89215305002966));
#29343=CARTESIAN_POINT('Ctrl Pts',(1.71254270725044,1.61564730372143,6.0193090474464));
#29344=CARTESIAN_POINT('Ctrl Pts',(-0.431154895060577,2.31452295730476,
6.14646504486313));
#29345=CARTESIAN_POINT('Ctrl Pts',(-2.1793964018332,0.89063482529591,6.27362104227988));
#29346=CARTESIAN_POINT('Ctrl Pts',(-1.92875295635622,-1.35015489936908,
6.4007770396966));
#29347=CARTESIAN_POINT('Ctrl Pts',(0.0909000405634622,-2.35259752788409,
6.52793303711335));
#29348=CARTESIAN_POINT('Ctrl Pts',(2.02718008066401,-1.19730236658674,6.65508903453007));
#29349=CARTESIAN_POINT('Ctrl Pts',(2.10417941628647,1.05613483800003,6.78224503194682));
#29350=CARTESIAN_POINT('Ctrl Pts',(0.251274807068405,2.3409077372054,6.90940102936354));
#29351=CARTESIAN_POINT('Ctrl Pts',(-1.83209287183882,1.47865681038455,7.0365570267803));
#29352=CARTESIAN_POINT('Ctrl Pts',(-2.23510849690114,-0.739783784629025,
7.16371302419701));
#29353=CARTESIAN_POINT('Ctrl Pts',(-0.58813550156722,-2.27971186575587,
7.29086902161376));
#29354=CARTESIAN_POINT('Ctrl Pts',(1.59826140798492,-1.72874242242604,7.41802501903049));
#29355=CARTESIAN_POINT('Ctrl Pts',(2.31877083899574,0.407788709281728,7.54518101644724));
#29356=CARTESIAN_POINT('Ctrl Pts',(0.912558585773612,2.17030564741532,7.67233701386396));
#29357=CARTESIAN_POINT('Ctrl Pts',(-1.3306307763662,1.94226969340383,7.79949301128071));
#29358=CARTESIAN_POINT('Ctrl Pts',(-2.35339711944582,-0.067170019446514,
7.92664900869743));
#29359=CARTESIAN_POINT('Ctrl Pts',(-1.21768338207199,-2.01500297453647,
8.05380500611418));
#29360=CARTESIAN_POINT('Ctrl Pts',(1.03486070218796,-2.11472294652947,8.1809610035309));
#29361=CARTESIAN_POINT('Ctrl Pts',(2.33825506962212,-0.274869133870564,
8.30811700094765));
#29362=CARTESIAN_POINT('Ctrl Pts',(1.49705728706912,1.81708813486099,8.43527299836438));
#29363=CARTESIAN_POINT('Ctrl Pts',(-0.717205969444591,2.24245521895696,
8.56242899578111));
#29364=CARTESIAN_POINT('Ctrl Pts',(-2.2736649035305,0.611095506216118,8.68958499319786));
#29365=CARTESIAN_POINT('Ctrl Pts',(-1.74477225780235,-1.58074652604342,
8.81674099061458));
#29366=CARTESIAN_POINT('Ctrl Pts',(0.384384164040551,-2.32276529717725,
8.94389698803133));
#29367=CARTESIAN_POINT('Ctrl Pts',(2.16099253781133,-0.934398770760454,
9.07105298544807));
#29368=CARTESIAN_POINT('Ctrl Pts',(1.95558975609324,1.31097616955231,9.19820898286478));
#29369=CARTESIAN_POINT('Ctrl Pts',(-0.0434336163049105,2.35395482800003,
9.32536498028155));
#29370=CARTESIAN_POINT('Ctrl Pts',(-2.00262070489792,1.2379418902333,9.45252097769825));
#29371=CARTESIAN_POINT('Ctrl Pts',(-2.12505153086449,-1.0134820188099,9.57967697511502));
#29372=CARTESIAN_POINT('Ctrl Pts',(-0.298435441371154,-2.33536423253774,
9.70683297253173));
#29373=CARTESIAN_POINT('Ctrl Pts',(1.80189856414474,-1.51530570374911,9.83398896994848));
#29374=CARTESIAN_POINT('Ctrl Pts',(2.24957389884245,0.694555314520332,9.96114496736521));
#29375=CARTESIAN_POINT('Ctrl Pts',(0.633993352467514,2.26738665434658,10.088300964782));
#29376=CARTESIAN_POINT('Ctrl Pts',(-1.56307087564499,1.76062467578759,10.2154569621987));
#29377=CARTESIAN_POINT('Ctrl Pts',(-2.32652353030908,-0.360940541086664,
10.3426129596154));
#29378=CARTESIAN_POINT('Ctrl Pts',(-0.956143925079784,-2.15145964540702,
10.4697689570321));
#29379=CARTESIAN_POINT('Ctrl Pts',(1.29118823440342,-1.96871093729374,10.5969249544489));
#29380=CARTESIAN_POINT('Ctrl Pts',(2.35427313729481,0.0196927980198272,
10.7240809518656));
#29381=CARTESIAN_POINT('Ctrl Pts',(1.25807449823434,1.99003476556925,10.8512369492824));
#29382=CARTESIAN_POINT('Ctrl Pts',(-0.992000263164342,2.13516399584755,
10.9783929466991));
#29383=CARTESIAN_POINT('Ctrl Pts',(-2.33223588655886,0.321971397376884,
11.1055489441158));
#29384=CARTESIAN_POINT('Ctrl Pts',(-1.53340001225001,-1.78652573832943,
11.2327049415326));
#29385=CARTESIAN_POINT('Ctrl Pts',(0.671834022590375,-2.2564637948285,11.3598609389493));
#29386=CARTESIAN_POINT('Ctrl Pts',(2.26087780961201,-0.656826720898154,
11.4870169363661));
#29387=CARTESIAN_POINT('Ctrl Pts',(1.77629803642563,1.54523625930544,11.6141729337828));
#29388=CARTESIAN_POINT('Ctrl Pts',(-0.337460210105816,2.33004515361337,
11.7413289311995));
#29389=CARTESIAN_POINT('Ctrl Pts',(-2.14170794734164,0.977791838570695,
11.8684849286162));
#29390=CARTESIAN_POINT('Ctrl Pts',(-1.98163189856334,-1.27126898407774,
11.995640926033));
#29391=CARTESIAN_POINT('Ctrl Pts',(-0.0040500230434116,-2.35435201458813,
12.1227969234497));
#29392=CARTESIAN_POINT('Ctrl Pts',(1.97724643765512,-1.27807915876207,12.2499529208664));
#29393=CARTESIAN_POINT('Ctrl Pts',(2.14505931245273,0.970417620069677,12.3771089182832));
#29394=CARTESIAN_POINT('Ctrl Pts',(0.345474608559887,2.32887034978811,12.5042649156999));
#29395=CARTESIAN_POINT('Ctrl Pts',(-1.77097122100624,1.55133837238995,12.6314209131167));
#29396=CARTESIAN_POINT('Ctrl Pts',(-2.26312420612221,-0.649044404448188,
12.7585769105334));
#29397=CARTESIAN_POINT('Ctrl Pts',(-0.679593289374679,-2.25413903127529,
12.8857329079501));
#29398=CARTESIAN_POINT('Ctrl Pts',(1.52724449084658,-1.79179074572356,13.0128889053669));
#29399=CARTESIAN_POINT('Ctrl Pts',(2.33332980892533,0.313945559073971,13.1400449027836));
#29400=CARTESIAN_POINT('Ctrl Pts',(0.999340309624393,2.13173843537186,13.2672009002004));
#29401=CARTESIAN_POINT('Ctrl Pts',(-1.25122044438684,1.99435132582757,13.3943568976171));
#29402=CARTESIAN_POINT('Ctrl Pts',(-2.35419145185632,0.0277924322151094,
13.5215128950338));
#29403=CARTESIAN_POINT('Ctrl Pts',(-1.29795383732276,-1.96425702174153,
13.6486688924505));
#29404=CARTESIAN_POINT('Ctrl Pts',(0.948736284503426,-2.15473647431616,
13.7758248898673));
#29405=CARTESIAN_POINT('Ctrl Pts',(2.32526796450381,-0.368942684619317,
13.902980887284));
#29406=CARTESIAN_POINT('Ctrl Pts',(1.56911895981938,1.75523659408559,14.0301368847008));
#29407=CARTESIAN_POINT('Ctrl Pts',(-0.626188777821492,2.26955445535291,
14.1572928821175));
#29408=CARTESIAN_POINT('Ctrl Pts',(-2.2471710046771,0.702290742513631,14.2844488795342));
#29409=CARTESIAN_POINT('Ctrl Pts',(-1.80710122805693,-1.50909740004977,
14.411604876951));
#29410=CARTESIAN_POINT('Ctrl Pts',(0.29039897945537,-2.33637716219216,14.5387608743677));
#29411=CARTESIAN_POINT('Ctrl Pts',(2.12155212340728,-1.02078714673918,14.6659168717844));
#29412=CARTESIAN_POINT('Ctrl Pts',(2.00686792550758,1.23104465428785,14.7930728692012));
#29413=CARTESIAN_POINT('Ctrl Pts',(0.0515320148678548,2.3537914654288,14.9202288666179));
#29414=CARTESIAN_POINT('Ctrl Pts',(-1.95106783886543,1.3176965126412,15.0473848640346));
#29415=CARTESIAN_POINT('Ctrl Pts',(-2.16419449726058,-0.926958461479726,
15.1745408614514));
#29416=CARTESIAN_POINT('Ctrl Pts',(-0.392373238827692,-2.32142909707225,
15.3016968588681));
#29417=CARTESIAN_POINT('Ctrl Pts',(1.73932345779521,-1.58673996623426,15.4288528562848));
#29418=CARTESIAN_POINT('Ctrl Pts',(2.27575388855762,0.603269467151035,15.5560088537016));
#29419=CARTESIAN_POINT('Ctrl Pts',(0.724916771960646,2.23997443847289,15.6831648511183));
#29420=CARTESIAN_POINT('Ctrl Pts',(-1.49079683249283,1.8222279263339,15.8103208485351));
#29421=CARTESIAN_POINT('Ctrl Pts',(-2.33918690349488,-0.266822865961399,
15.9374768459518));
#29422=CARTESIAN_POINT('Ctrl Pts',(-1.04213016874964,-2.11115004740632,
16.0646328433685));
#29423=CARTESIAN_POINT('Ctrl Pts',(1.2107436656794,-2.0191804246523,16.1917888407853));
#29424=CARTESIAN_POINT('Ctrl Pts',(2.3531520959846,-0.0752663566615951,
16.318944838202));
#29425=CARTESIAN_POINT('Ctrl Pts',(1.33730517686693,1.93768023038033,16.4461008356188));
#29426=CARTESIAN_POINT('Ctrl Pts',(-0.905086365825657,2.17343241939525,
16.5732568330355));
#29427=CARTESIAN_POINT('Ctrl Pts',(-2.31735413791021,0.415763888273461,
16.7004128304522));
#29428=CARTESIAN_POINT('Ctrl Pts',(-1.60419959956003,-1.72323343051753,
16.8275688278689));
#29429=CARTESIAN_POINT('Ctrl Pts',(0.580288803354365,-2.28172187524759,
16.9547248252857));
#29430=CARTESIAN_POINT('Ctrl Pts',(2.23255006456091,-0.747469076625183,
17.0818808227024));
#29431=CARTESIAN_POINT('Ctrl Pts',(1.83716930215367,1.47234464936238,17.2090368201192));
#29432=CARTESIAN_POINT('Ctrl Pts',(-0.243219616307141,2.3417587470799,17.3361928175359));
#29433=CARTESIAN_POINT('Ctrl Pts',(-2.10053326527084,1.0633672050484,17.4633488149526));
#29434=CARTESIAN_POINT('Ctrl Pts',(-2.03128757106783,-1.19031954319298,
17.5905048123694));
#29435=CARTESIAN_POINT('Ctrl Pts',(-0.0989930437893146,-2.35227340854824,
17.7176608097861));
#29436=CARTESIAN_POINT('Ctrl Pts',(1.92409555781977,-1.3567778357786,17.8448168072028));
#29437=CARTESIAN_POINT('Ctrl Pts',(2.18244930121404,0.88312222195582,17.9719728046196));
#29438=CARTESIAN_POINT('Ctrl Pts',(0.439112254103542,2.31304350144521,18.0991288020363));
#29439=CARTESIAN_POINT('Ctrl Pts',(-1.70696814862484,1.62149608413407,18.2262847994531));
#29440=CARTESIAN_POINT('Ctrl Pts',(-2.28745780847244,-0.557249123588607,
18.3534407968698));
#29441=CARTESIAN_POINT('Ctrl Pts',(-0.769945362914689,-2.22489863800758,
18.4805967942865));
#29442=CARTESIAN_POINT('Ctrl Pts',(1.45374272726439,-1.85192383596294,18.6077527917033));
#29443=CARTESIAN_POINT('Ctrl Pts',(2.34409243138809,0.219591630967329,18.73490878912));
#29444=CARTESIAN_POINT('Ctrl Pts',(1.08449609580706,2.0897028567385,18.8620647865367));
#29445=CARTESIAN_POINT('Ctrl Pts',(-1.16977436398285,2.04318813344496,18.9892207839534));
#29446=CARTESIAN_POINT('Ctrl Pts',(-2.35115549248314,0.122709663222533,
19.1163767813702));
#29447=CARTESIAN_POINT('Ctrl Pts',(-1.37611250898677,-1.91031520275895,
19.2435327787869));
#29448=CARTESIAN_POINT('Ctrl Pts',(0.8610682636463,-2.19124422569073,19.3706887762036));
#29449=CARTESIAN_POINT('Ctrl Pts',(2.30849762607345,-0.462415961765052,
19.4978447736204));
#29450=CARTESIAN_POINT('Ctrl Pts',(1.63862766088603,1.69052926631307,19.6250007710371));
#29451=CARTESIAN_POINT('Ctrl Pts',(-0.534152771012978,2.29296110488185,
19.7521567684539));
#29452=CARTESIAN_POINT('Ctrl Pts',(-2.21702093697091,0.79234334496762,19.8793127658706));
#29453=CARTESIAN_POINT('Ctrl Pts',(-1.8664900272104,-1.43499295803357,20.0064687632874));
#29454=CARTESIAN_POINT('Ctrl Pts',(0.195941312932475,-2.34618771908133,
20.1336247607041));
#29455=CARTESIAN_POINT('Ctrl Pts',(2.07865992327303,-1.10551469219562,20.2607807581208));
#29456=CARTESIAN_POINT('Ctrl Pts',(2.05488090148423,1.14911021751495,20.3879367555375));
#29457=CARTESIAN_POINT('Ctrl Pts',(0.146413802956549,2.34979846148252,20.5150927529543));
#29458=CARTESIAN_POINT('Ctrl Pts',(-1.8963405666742,1.3953072301352,20.642248750371));
#29459=CARTESIAN_POINT('Ctrl Pts',(-2.19981629837245,-0.838926733807399,
20.7694047477878));
#29460=CARTESIAN_POINT('Ctrl Pts',(-0.485672641246882,-2.30371697411512,
20.8965607452045));
#29461=CARTESIAN_POINT('Ctrl Pts',(1.67391845543353,-1.65559258751689,21.0237167426212));
#29462=CARTESIAN_POINT('Ctrl Pts',(2.29823120478489,0.511002094550286,21.150872740038));
#29463=CARTESIAN_POINT('Ctrl Pts',(0.814660744886235,2.20891776262115,21.2780287374547));
#29464=CARTESIAN_POINT('Ctrl Pts',(-1.41609724854068,1.88086639449945,21.4051847348714));
#29465=CARTESIAN_POINT('Ctrl Pts',(-2.34804439706675,-0.172271067464243,
21.5323407322882));
#29466=CARTESIAN_POINT('Ctrl Pts',(-1.12642085660117,-2.06740558795213,
21.6594967297049));
#29467=CARTESIAN_POINT('Ctrl Pts',(1.12832920535418,-2.06636468601906,21.7866527271216));
#29468=CARTESIAN_POINT('Ctrl Pts',(2.34820245355783,-0.170103052256023,
21.9138087245384));
#29469=CARTESIAN_POINT('Ctrl Pts',(1.41436004710103,1.88217307080039,22.0409647219551));
#29470=CARTESIAN_POINT('Ctrl Pts',(-0.816699884255499,2.20816464747058,
22.1681207193719));
#29471=CARTESIAN_POINT('Ctrl Pts',(-2.29870203176745,0.508879927320817,
22.2952767167886));
#29472=CARTESIAN_POINT('Ctrl Pts',(-1.6723891386762,-1.65713740532272,22.4224327142054));
#29473=CARTESIAN_POINT('Ctrl Pts',(0.487799448648201,-2.303267572207,22.549588711622));
#29474=CARTESIAN_POINT('Ctrl Pts',(2.20058993905954,-0.836895292967851,
22.6767447090389));
#29475=CARTESIAN_POINT('Ctrl Pts',(1.89505147573867,1.3970575204989,22.8039007064555));
#29476=CARTESIAN_POINT('Ctrl Pts',(-0.148583301850979,2.34966227651824,
22.9310567038723));
#29477=CARTESIAN_POINT('Ctrl Pts',(-2.05594099535328,1.1472124628453,23.058212701289));
#29478=CARTESIAN_POINT('Ctrl Pts',(-2.07763831913675,-1.10743344095094,
23.1853686987058));
#29479=CARTESIAN_POINT('Ctrl Pts',(-0.193775001899879,-2.34636763102471,
23.3125246961225));
#29480=CARTESIAN_POINT('Ctrl Pts',(1.86781415598644,-1.43326902219314,23.4396806935392));
#29481=CARTESIAN_POINT('Ctrl Pts',(2.21628842394943,0.794389975484045,23.566836690956));
#29482=CARTESIAN_POINT('Ctrl Pts',(0.532035459781954,2.29345330905524,23.6939926883727));
#29483=CARTESIAN_POINT('Ctrl Pts',(-1.64018782263076,1.68901560613737,23.8211486857894));
#29484=CARTESIAN_POINT('Ctrl Pts',(-2.3080696949444,-0.464547193039696,
23.9483046832062));
#29485=CARTESIAN_POINT('Ctrl Pts',(-0.859044727936122,-2.19203831323428,
24.0754606806229));
#29486=CARTESIAN_POINT('Ctrl Pts',(1.37787571026816,-1.9090438282907,24.2026166780396));
#29487=CARTESIAN_POINT('Ctrl Pts',(2.35104119289581,0.124880425162849,24.3297726754563));
#29488=CARTESIAN_POINT('Ctrl Pts',(1.16788739640021,2.04426731143737,24.4569286728731));
#29489=CARTESIAN_POINT('Ctrl Pts',(-1.08642504942599,2.08870065429722,24.5840846702898));
#29490=CARTESIAN_POINT('Ctrl Pts',(-2.34429418048653,0.217427244426385,
24.7112406677066));
#29491=CARTESIAN_POINT('Ctrl Pts',(-1.45203223234926,-1.85326528254879,
24.8383966651233));
#29492=CARTESIAN_POINT('Ctrl Pts',(0.771999276433814,-2.22418680161256,
24.9655526625401));
#29493=CARTESIAN_POINT('Ctrl Pts',(2.28797133977901,-0.555136883688751,
25.0927086599568));
#29494=CARTESIAN_POINT('Ctrl Pts',(1.70547029897151,1.6230714311477,25.2198646573735));
#29495=CARTESIAN_POINT('Ctrl Pts',(-0.44124769250315,2.31263708461627,25.3470206547902));
#29496=CARTESIAN_POINT('Ctrl Pts',(-2.18326375485454,0.881106797170618,
25.474176652207));
#29497=CARTESIAN_POINT('Ctrl Pts',(-1.92284202911887,-1.35855376865836,
25.6013326496237));
#29498=CARTESIAN_POINT('Ctrl Pts',(0.101164848006878,-2.35218100596224,
25.7284886470405));
#29499=CARTESIAN_POINT('Ctrl Pts',(2.03238572343009,-1.18844355460383,25.8556446444572));
#29500=CARTESIAN_POINT('Ctrl Pts',(2.09955056644954,1.06530616735437,25.982800641874));
#29501=CARTESIAN_POINT('Ctrl Pts',(0.241057374378188,2.3419823128153,26.1099566392906));
#29502=CARTESIAN_POINT('Ctrl Pts',(-1.83852793012283,1.47064776933163,26.2371126367074));
#29503=CARTESIAN_POINT('Ctrl Pts',(-2.23185897718681,-0.74953006426191,
26.3642686341241));
#29504=CARTESIAN_POINT('Ctrl Pts',(-0.578181849602668,-2.28225668146067,
26.4914246315409));
#29505=CARTESIAN_POINT('Ctrl Pts',(1.60578997162814,-1.72175154371944,26.6185806289576));
#29506=CARTESIAN_POINT('Ctrl Pts',(2.31696927671439,0.417903316621709,26.7457366263743));
#29507=CARTESIAN_POINT('Ctrl Pts',(0.903079256936234,2.17426715630194,26.8728926237911));
#29508=CARTESIAN_POINT('Ctrl Pts',(-1.3390936607308,1.93644467493197,27.0000486212078));
#29509=CARTESIAN_POINT('Ctrl Pts',(-2.35308159979739,-0.0774389822816324,
27.1272046186246));
#29510=CARTESIAN_POINT('Ctrl Pts',(-1.20887884687377,-2.02029743970114,
27.2543606160413));
#29511=CARTESIAN_POINT('Ctrl Pts',(1.04407894254815,-2.1101869521465,27.381516613458));
#29512=CARTESIAN_POINT('Ctrl Pts',(2.33943226313038,-0.264662988546719,
27.5086726108748));
#29513=CARTESIAN_POINT('Ctrl Pts',(1.48911373992093,1.82360359751251,27.6358286082915));
#29514=CARTESIAN_POINT('Ctrl Pts',(-0.726984624110384,2.23930417040404,
27.7629846057082));
#29515=CARTESIAN_POINT('Ctrl Pts',(-2.27630991528687,0.601168013826854,
27.890140603125));
#29516=CARTESIAN_POINT('Ctrl Pts',(-1.73785768456178,-1.58834520161436,
28.0172966005417));
#29517=CARTESIAN_POINT('Ctrl Pts',(0.394516439542522,-2.32106583065033,
28.1444525979584));
#29518=CARTESIAN_POINT('Ctrl Pts',(2.16504943253982,-0.924959872611133,
28.2716085953752));
#29519=CARTESIAN_POINT('Ctrl Pts',(1.94985038232687,1.31949736559857,28.3987645927919));
#29520=CARTESIAN_POINT('Ctrl Pts',(-0.0537052409321449,2.35374288280989,
28.5259205902087));
#29521=CARTESIAN_POINT('Ctrl Pts',(-2.00800368964148,1.22919119491966,28.6530765876254));
#29522=CARTESIAN_POINT('Ctrl Pts',(-2.12060872965672,-1.02274553383799,
28.7802325850421));
#29523=CARTESIAN_POINT('Ctrl Pts',(-0.28824168621664,-2.33664429077444,
28.9073885824589));
#29524=CARTESIAN_POINT('Ctrl Pts',(1.80849380253782,-1.5074282661089,29.0345445798756));
#29525=CARTESIAN_POINT('Ctrl Pts',(2.24652162408042,0.704365248873706,29.1617005772923));
#29526=CARTESIAN_POINT('Ctrl Pts',(0.624093038644794,2.27013164604984,29.2888565747091));
#29527=CARTESIAN_POINT('Ctrl Pts',(-1.57073889525738,1.75378708348746,29.4160125721258));
#29528=CARTESIAN_POINT('Ctrl Pts',(-2.32492632980036,-0.371089439735015,
29.5431685695426));
#29529=CARTESIAN_POINT('Ctrl Pts',(-0.946746418914216,-2.15561152102017,
29.6703245669592));
#29530=CARTESIAN_POINT('Ctrl Pts',(1.29976687622502,-1.96305778792936,29.797480564376));
#29531=CARTESIAN_POINT('Ctrl Pts',(2.35416478774663,0.0299660377042993,
29.9246365617928));
#29532=CARTESIAN_POINT('Ctrl Pts',(1.24937853295487,1.99550572353809,30.0517925592095));
#29533=CARTESIAN_POINT('Ctrl Pts',(-1.00130811085348,2.13081483907472,30.1789485566262));
#29534=CARTESIAN_POINT('Ctrl Pts',(-2.33361867928712,0.311791069410117,
30.306104554043));
#29535=CARTESIAN_POINT('Ctrl Pts',(-1.5255894852895,-1.79320008188034,30.4332605514597));
#29536=CARTESIAN_POINT('Ctrl Pts',(0.681674238965734,-2.25351060419371,
30.5604165488764));
#29537=CARTESIAN_POINT('Ctrl Pts',(2.26372250208576,-0.646954592557379,
30.6875725462932));
#29538=CARTESIAN_POINT('Ctrl Pts',(1.76953812046046,1.55297284313587,30.8147285437099));
#29539=CARTESIAN_POINT('Ctrl Pts',(-0.347624699749826,2.3285503815494,30.9418845411267));
#29540=CARTESIAN_POINT('Ctrl Pts',(-2.14595438158722,0.968436680128043,
31.0690405385433));
#29541=CARTESIAN_POINT('Ctrl Pts',(-1.97606554853479,-1.27990419921524,
31.1961965359601));
#29542=CARTESIAN_POINT('Ctrl Pts',(0.00622378690368324,-2.35434727171091,
31.3233525333769));
#29543=CARTESIAN_POINT('Ctrl Pts',(1.98280481243926,-1.26943880788431,31.4505085307936));
#29544=CARTESIAN_POINT('Ctrl Pts',(2.14080424244349,0.979768853760829,31.5776645282103));
#29545=CARTESIAN_POINT('Ctrl Pts',(0.335308743102262,2.33035573645602,31.704820525627));
#29546=CARTESIAN_POINT('Ctrl Pts',(-1.77772399087328,1.54359555029578,31.8319765230438));
#29547=CARTESIAN_POINT('Ctrl Pts',(-2.26027040006032,-0.658913901795522,
31.9591325204605));
#29548=CARTESIAN_POINT('Ctrl Pts',(-0.669750350324828,-2.25708313576418,
32.0862885178773));
#29549=CARTESIAN_POINT('Ctrl Pts',(1.53504885170168,-1.78510919252983,32.213444515294));
#29550=CARTESIAN_POINT('Ctrl Pts',(2.33193761804057,0.324124603965224,32.3406005127108));
#29551=CARTESIAN_POINT('Ctrl Pts',(0.990028448971534,2.13607900021394,32.4677565101275));
#29552=CARTESIAN_POINT('Ctrl Pts',(-1.25991135203251,1.98887233393488,32.5949125075442));
#29553=CARTESIAN_POINT('Ctrl Pts',(-2.35429032108445,0.0175191107867025,
32.7220685049609));
#29554=CARTESIAN_POINT('Ctrl Pts',(-1.28936997013835,-1.96990227459506,
32.8492245023777));
#29555=CARTESIAN_POINT('Ctrl Pts',(0.958129935167091,-2.15057587320433,
32.9763804997944));
#29556=CARTESIAN_POINT('Ctrl Pts',(2.32685582836193,-0.358792412040517,
33.1035364972112));
#29557=CARTESIAN_POINT('Ctrl Pts',(1.56144456462104,1.76206728746512,33.2306924946279));
#29558=CARTESIAN_POINT('Ctrl Pts',(-0.636086427672334,2.26679997337798,
33.3578484920446));
#29559=CARTESIAN_POINT('Ctrl Pts',(-2.2502144595619,0.692478662443505,33.4850044894614));
#29560=CARTESIAN_POINT('Ctrl Pts',(-1.80049826378972,-1.51697001900675,
33.612160486878));
#29561=CARTESIAN_POINT('Ctrl Pts',(0.300590680029782,-2.33508526368096,
33.7393164842949));
#29562=CARTESIAN_POINT('Ctrl Pts',(2.12598802528465,-1.01152416446146,33.8664724817115));
#29563=CARTESIAN_POINT('Ctrl Pts',(2.00147370727853,1.23979920447876,33.9936284791284));
#29564=CARTESIAN_POINT('Ctrl Pts',(0.0412662164209308,2.35397709479251,
34.120784476545));
#29565=CARTESIAN_POINT('Ctrl Pts',(-1.95681081498566,1.30920211141525,34.2479404739618));
#29566=CARTESIAN_POINT('Ctrl Pts',(-2.16010701708612,-0.936454790837551,
34.3750964713785));
#29567=CARTESIAN_POINT('Ctrl Pts',(-0.382281098867528,-2.32300256131819,
34.5022524687953));
#29568=CARTESIAN_POINT('Ctrl Pts',(1.74631052042418,-1.57935733701702,34.629408466212));
#29569=CARTESIAN_POINT('Ctrl Pts',(2.27294807479828,0.613618922507192,34.7565644636287));
#29570=CARTESIAN_POINT('Ctrl Pts',(0.715424783306792,2.24230425940323,34.8837204610454));
#29571=CARTESIAN_POINT('Ctrl Pts',(-1.49929057408143,1.81728029455531,35.0108764584622));
#29572=CARTESIAN_POINT('Ctrl Pts',(-2.33695427846112,-0.280391065156878,
35.138040218466));
#29573=CARTESIAN_POINT('Ctrl Pts',(-1.46906893796398,-1.49873552768042,
35.2228186459975));
#29574=CARTESIAN_POINT('Ctrl Pts',(-0.873247403090202,-1.78947960423924,
35.2652117410568));
#29575=CARTESIAN_POINT('Ctrl Pts',(-1.16285319861171,1.62483593567698,35.));
#29576=CARTESIAN_POINT('Ctrl Pts',(-1.2034571535085,1.60237251915514,35.));
#29577=CARTESIAN_POINT('Ctrl Pts',(-1.24313101615398,1.5784475810686,35.));
#29578=CARTESIAN_POINT('Ctrl Pts',(-1.28178678438056,1.55308309322909,35.));
#29579=CARTESIAN_POINT('Ctrl Pts',(-1.34124439891837,1.51406920189803,35.));
#29580=CARTESIAN_POINT('Ctrl Pts',(-1.39829464397926,1.4716523739051,35.));
#29581=CARTESIAN_POINT('Ctrl Pts',(-1.45286647428986,1.42618637516297,35.));
#29582=CARTESIAN_POINT('Ctrl Pts',(-1.50919953362205,1.37925302529803,35.));
#29583=CARTESIAN_POINT('Ctrl Pts',(-1.56289222325683,1.3290701152209,35.));
#29584=CARTESIAN_POINT('Ctrl Pts',(-1.61384568307356,1.27597508797261,35.));
#29585=CARTESIAN_POINT('Ctrl Pts',(-1.63889408811983,1.24987390165,35.));
#29586=CARTESIAN_POINT('Ctrl Pts',(-1.66328015009881,1.22306822207441,35.));
#29587=CARTESIAN_POINT('Ctrl Pts',(-1.68698967741847,1.19559427323466,35.));
#29588=CARTESIAN_POINT('Ctrl Pts',(-1.7056134239364,1.17401358745636,35.));
#29589=CARTESIAN_POINT('Ctrl Pts',(-1.72381971498931,1.15202052478812,35.));
#29590=CARTESIAN_POINT('Ctrl Pts',(-1.74160084989885,1.12963170748219,35.));
#29591=CARTESIAN_POINT('Ctrl Pts',(-1.75105180158785,1.1177317004349,35.));
#29592=CARTESIAN_POINT('Ctrl Pts',(-1.76038424143082,1.10571756791684,35.));
#29593=CARTESIAN_POINT('Ctrl Pts',(-1.76958246640894,1.09361130996028,35.));
#29594=CARTESIAN_POINT('Ctrl Pts',(-1.81578754020787,1.03279843099259,35.));
#29595=CARTESIAN_POINT('Ctrl Pts',(-1.85868694579373,0.969568012909778,
35.));
#29596=CARTESIAN_POINT('Ctrl Pts',(-1.89819404295453,0.904303946702904,
35.));
#29597=CARTESIAN_POINT('Ctrl Pts',(-1.9383827536208,0.837913883595611,35.));
#29598=CARTESIAN_POINT('Ctrl Pts',(-1.97506173048199,0.769418694780337,
35.));
#29599=CARTESIAN_POINT('Ctrl Pts',(-2.00810989179612,0.699176647445272,
35.));
#29600=CARTESIAN_POINT('Ctrl Pts',(-2.03387549323432,0.644413280169376,
35.));
#29601=CARTESIAN_POINT('Ctrl Pts',(-2.05743364892923,0.588587058078158,
35.));
#29602=CARTESIAN_POINT('Ctrl Pts',(-2.07871088918223,0.531853309281494,
35.));
#29603=CARTESIAN_POINT('Ctrl Pts',(-2.08934950930873,0.503486434883161,
35.));
#29604=CARTESIAN_POINT('Ctrl Pts',(-2.09941766122464,0.474892509303888,
35.));
#29605=CARTESIAN_POINT('Ctrl Pts',(-2.10890461491907,0.446090093541291,
35.));
#29606=CARTESIAN_POINT('Ctrl Pts',(-2.11515647320623,0.427109435737392,
35.));
#29607=CARTESIAN_POINT('Ctrl Pts',(-2.12115622262752,0.40803718097923,35.));
#29608=CARTESIAN_POINT('Ctrl Pts',(-2.12689957333395,0.388881715849516,
35.));
#29609=CARTESIAN_POINT('Ctrl Pts',(-2.12987153569128,0.378969501845442,
35.));
#29610=CARTESIAN_POINT('Ctrl Pts',(-2.13277431889566,0.36903665131058,35.));
#29611=CARTESIAN_POINT('Ctrl Pts',(-2.13560562780928,0.359090962659784,
35.));
#29612=CARTESIAN_POINT('Ctrl Pts',(-2.15761496010993,0.281777616376262,
35.));
#29613=CARTESIAN_POINT('Ctrl Pts',(-2.17534799254665,0.203559623333045,
35.));
#29614=CARTESIAN_POINT('Ctrl Pts',(-2.18868635601065,0.124817877959984,
35.));
#29615=CARTESIAN_POINT('Ctrl Pts',(-2.20197077284454,0.0463946013273144,
35.));
#29616=CARTESIAN_POINT('Ctrl Pts',(-2.21089654715116,-0.0325491535936027,
35.));
#29617=CARTESIAN_POINT('Ctrl Pts',(-2.2153044627471,-0.111665411483039,
35.));
#29618=CARTESIAN_POINT('Ctrl Pts',(-2.21812153834263,-0.162228194380512,
35.));
#29619=CARTESIAN_POINT('Ctrl Pts',(-2.21909245699586,-0.212861963887261,
35.));
#29620=CARTESIAN_POINT('Ctrl Pts',(-2.21816496049036,-0.263479248160428,
35.));
#29621=CARTESIAN_POINT('Ctrl Pts',(-2.21727633251441,-0.311975317532206,
35.));
#29622=CARTESIAN_POINT('Ctrl Pts',(-2.21464503552917,-0.360456344076136,
35.));
#29623=CARTESIAN_POINT('Ctrl Pts',(-2.21031794958881,-0.408861980263073,
35.));
#29624=CARTESIAN_POINT('Ctrl Pts',(-2.20896704755131,-0.423974061107329,
35.));
#29625=CARTESIAN_POINT('Ctrl Pts',(-2.20745080465866,-0.439078794635521,
35.));
#29626=CARTESIAN_POINT('Ctrl Pts',(-2.20577049210996,-0.454174341115026,
35.));
#29627=CARTESIAN_POINT('Ctrl Pts',(-2.20425945721676,-0.467749135566183,
35.));
#29628=CARTESIAN_POINT('Ctrl Pts',(-2.20261652682881,-0.481309054795014,
35.));
#29629=CARTESIAN_POINT('Ctrl Pts',(-2.2008440773238,-0.494845688706287,
35.));
#29630=CARTESIAN_POINT('Ctrl Pts',(-2.1906273199638,-0.572873583860459,
35.));
#29631=CARTESIAN_POINT('Ctrl Pts',(-2.17610342800899,-0.650199777639862,
35.));
#29632=CARTESIAN_POINT('Ctrl Pts',(-2.15754788660862,-0.726565307611558,
35.));
#29633=CARTESIAN_POINT('Ctrl Pts',(-2.13861027143035,-0.804503266320675,
35.));
#29634=CARTESIAN_POINT('Ctrl Pts',(-2.11547312842759,-0.881441324263912,
35.));
#29635=CARTESIAN_POINT('Ctrl Pts',(-2.08837491381414,-0.957111475263221,
35.));
#29636=CARTESIAN_POINT('Ctrl Pts',(-2.06075709345851,-1.03423259436255,
35.));
#29637=CARTESIAN_POINT('Ctrl Pts',(-2.0290246498135,-1.11003758370528,35.));
#29638=CARTESIAN_POINT('Ctrl Pts',(-1.99337661763573,-1.18423795994886,
35.));
#29639=CARTESIAN_POINT('Ctrl Pts',(-1.98369777462059,-1.20438419943115,
35.));
#29640=CARTESIAN_POINT('Ctrl Pts',(-1.97372999136114,-1.22441208038623,
35.));
#29641=CARTESIAN_POINT('Ctrl Pts',(-1.9634766200881,-1.24431563610298,35.));
#29642=CARTESIAN_POINT('Ctrl Pts',(-1.95462855428264,-1.26149125240076,
35.));
#29643=CARTESIAN_POINT('Ctrl Pts',(-1.94556781553865,-1.27857428649159,
35.));
#29644=CARTESIAN_POINT('Ctrl Pts',(-1.93629640525643,-1.29556083361615,
35.));
#29645=CARTESIAN_POINT('Ctrl Pts',(-1.92954927376081,-1.30792254166459,
35.));
#29646=CARTESIAN_POINT('Ctrl Pts',(-1.92269527151118,-1.32022451322101,
35.));
#29647=CARTESIAN_POINT('Ctrl Pts',(-1.9157363590997,-1.33246413569888,35.));
#29648=CARTESIAN_POINT('Ctrl Pts',(-1.87408701044033,-1.40571872979299,
35.));
#29649=CARTESIAN_POINT('Ctrl Pts',(-1.82867588507373,-1.47675530540997,
35.));
#29650=CARTESIAN_POINT('Ctrl Pts',(-1.77974591339315,-1.54527892431103,
35.));
#29651=CARTESIAN_POINT('Ctrl Pts',(-1.73048679382613,-1.61426349594838,
35.));
#29652=CARTESIAN_POINT('Ctrl Pts',(-1.67766096404848,-1.68070212529753,
35.));
#29653=CARTESIAN_POINT('Ctrl Pts',(-1.62146650439762,-1.74427821650641,
35.));
#29654=CARTESIAN_POINT('Ctrl Pts',(-1.60491685000561,-1.76300181209999,
35.));
#29655=CARTESIAN_POINT('Ctrl Pts',(-1.58807471310564,-1.78147697299719,
35.));
#29656=CARTESIAN_POINT('Ctrl Pts',(-1.57094441010341,-1.79969516910559,
35.));
#29657=CARTESIAN_POINT('Ctrl Pts',(-1.55994931079185,-1.81138853351738,
35.));
#29658=CARTESIAN_POINT('Ctrl Pts',(-1.54884194222482,-1.82296914707541,
35.));
#29659=CARTESIAN_POINT('Ctrl Pts',(-1.53762523100423,-1.83443366707108,
35.));
#29660=CARTESIAN_POINT('Ctrl Pts',(-1.47735309480073,-1.89603738469371,
35.));
#29661=CARTESIAN_POINT('Ctrl Pts',(-1.41391520823538,-1.95430395747543,
35.));
#29662=CARTESIAN_POINT('Ctrl Pts',(-1.34753369268451,-2.00892008903311,
35.));
#29663=CARTESIAN_POINT('Ctrl Pts',(-1.28175657869132,-2.06303894247482,
35.));
#29664=CARTESIAN_POINT('Ctrl Pts',(-1.21308869306104,-2.11357440098649,
35.));
#29665=CARTESIAN_POINT('Ctrl Pts',(-1.14170435717708,-2.1601933216293,35.));
#29666=CARTESIAN_POINT('Ctrl Pts',(-1.11975470438348,-2.17452796674509,
35.));
#29667=CARTESIAN_POINT('Ctrl Pts',(-1.09754794696018,-2.18849205896657,
35.));
#29668=CARTESIAN_POINT('Ctrl Pts',(-1.07508846035141,-2.20207516956602,
35.));
#29669=CARTESIAN_POINT('Ctrl Pts',(1.07765321779378,2.20537369629785,5.));
#29670=CARTESIAN_POINT('Ctrl Pts',(1.12605534704973,2.17638462489288,5.));
#29671=CARTESIAN_POINT('Ctrl Pts',(1.1733135262994,2.14564792857991,5.));
#29672=CARTESIAN_POINT('Ctrl Pts',(1.21932045153113,2.11315756143298,5.));
#29673=CARTESIAN_POINT('Ctrl Pts',(1.28915280522501,2.06384153349108,5.));
#29674=CARTESIAN_POINT('Ctrl Pts',(1.35610447303115,2.01048641170541,5.));
#29675=CARTESIAN_POINT('Ctrl Pts',(1.42000521897292,1.95345758415458,5.));
#29676=CARTESIAN_POINT('Ctrl Pts',(1.45203025925604,1.92487653282728,5.));
#29677=CARTESIAN_POINT('Ctrl Pts',(1.48328834939632,1.89537222664871,5.));
#29678=CARTESIAN_POINT('Ctrl Pts',(1.51375388140517,1.86498810835876,5.));
#29679=CARTESIAN_POINT('Ctrl Pts',(1.52811363799061,1.85066672567029,5.));
#29680=CARTESIAN_POINT('Ctrl Pts',(1.54229727331263,1.83614985958058,5.));
#29681=CARTESIAN_POINT('Ctrl Pts',(1.55630187408297,1.82144196987146,5.));
#29682=CARTESIAN_POINT('Ctrl Pts',(1.56790736208478,1.80925367258614,5.));
#29683=CARTESIAN_POINT('Ctrl Pts',(1.57939111667914,1.79693273685352,5.));
#29684=CARTESIAN_POINT('Ctrl Pts',(1.59073993809508,1.78449460478855,5.));
#29685=CARTESIAN_POINT('Ctrl Pts',(1.6478349293045,1.72191938090552,5.));
#29686=CARTESIAN_POINT('Ctrl Pts',(1.70158263478878,1.65631424483516,5.));
#29687=CARTESIAN_POINT('Ctrl Pts',(1.75181663638728,1.58803510705647,5.));
#29688=CARTESIAN_POINT('Ctrl Pts',(1.80202321464289,1.51979324367655,5.));
#29689=CARTESIAN_POINT('Ctrl Pts',(1.84872029427685,1.44887929457968,5.));
#29690=CARTESIAN_POINT('Ctrl Pts',(1.89169373885761,1.37563015276107,5.));
#29691=CARTESIAN_POINT('Ctrl Pts',(1.89767700253961,1.36543155373656,5.));
#29692=CARTESIAN_POINT('Ctrl Pts',(1.90358800061462,1.35518767071414,5.));
#29693=CARTESIAN_POINT('Ctrl Pts',(1.90942607495413,1.34489940162725,5.));
#29694=CARTESIAN_POINT('Ctrl Pts',(1.91766729738792,1.33037613435231,5.));
#29695=CARTESIAN_POINT('Ctrl Pts',(1.92576320743067,1.31576441843905,5.));
#29696=CARTESIAN_POINT('Ctrl Pts',(1.93371188435635,1.30106677809768,5.));
#29697=CARTESIAN_POINT('Ctrl Pts',(1.94061116483423,1.28830954264504,5.));
#29698=CARTESIAN_POINT('Ctrl Pts',(1.94739530897506,1.27549531421591,5.));
#29699=CARTESIAN_POINT('Ctrl Pts',(1.95406177942983,1.26262928097317,5.));
#29700=CARTESIAN_POINT('Ctrl Pts',(1.99226151800852,1.18890524518061,5.));
#29701=CARTESIAN_POINT('Ctrl Pts',(2.02662081955031,1.11344588745721,5.));
#29702=CARTESIAN_POINT('Ctrl Pts',(2.05697787439092,1.03658084236829,5.));
#29703=CARTESIAN_POINT('Ctrl Pts',(2.08698381426429,0.960604831737085,5.));
#29704=CARTESIAN_POINT('Ctrl Pts',(2.11307977329731,0.883254514836898,5.));
#29705=CARTESIAN_POINT('Ctrl Pts',(2.13505987244827,0.804839634021934,5.));
#29706=CARTESIAN_POINT('Ctrl Pts',(2.15637299228847,0.728804228513231,5.));
#29707=CARTESIAN_POINT('Ctrl Pts',(2.17381627703144,0.651767110791863,5.));
#29708=CARTESIAN_POINT('Ctrl Pts',(2.18715357665171,0.574015077520465,5.));
#29709=CARTESIAN_POINT('Ctrl Pts',(2.19288012175061,0.540631218888172,5.));
#29710=CARTESIAN_POINT('Ctrl Pts',(2.19784909558329,0.507115686650812,5.));
#29711=CARTESIAN_POINT('Ctrl Pts',(2.20203891829051,0.473491966359662,5.));
#29712=CARTESIAN_POINT('Ctrl Pts',(2.203880446088,0.458713533023023,5.));
#29713=CARTESIAN_POINT('Ctrl Pts',(2.20557146498055,0.443912805281082,5.));
#29714=CARTESIAN_POINT('Ctrl Pts',(2.20710823476353,0.429112420088137,5.));
#29715=CARTESIAN_POINT('Ctrl Pts',(2.21517716213172,0.351401864827779,5.));
#29716=CARTESIAN_POINT('Ctrl Pts',(2.21901524210411,0.273570144957761,5.));
#29717=CARTESIAN_POINT('Ctrl Pts',(2.21844424195061,0.195896659425403,5.));
#29718=CARTESIAN_POINT('Ctrl Pts',(2.21822709066427,0.166357442676425,5.));
#29719=CARTESIAN_POINT('Ctrl Pts',(2.21737173543002,0.136841145695996,5.));
#29720=CARTESIAN_POINT('Ctrl Pts',(2.21586638874295,0.107363405091233,5.));
#29721=CARTESIAN_POINT('Ctrl Pts',(2.21181137114425,0.0279579379327235,
5.));
#29722=CARTESIAN_POINT('Ctrl Pts',(2.20304328499261,-0.0511693321485583,
5.));
#29723=CARTESIAN_POINT('Ctrl Pts',(2.18975147681156,-0.129695492434029,
5.));
#29724=CARTESIAN_POINT('Ctrl Pts',(2.17683622913987,-0.20599698542724,5.));
#29725=CARTESIAN_POINT('Ctrl Pts',(2.15964916296706,-0.281731621075645,
5.));
#29726=CARTESIAN_POINT('Ctrl Pts',(2.13832461156907,-0.356577243192453,
5.));
#29727=CARTESIAN_POINT('Ctrl Pts',(2.13318601839716,-0.374612848986876,
5.));
#29728=CARTESIAN_POINT('Ctrl Pts',(2.1278049053625,-0.392602968217722,5.));
#29729=CARTESIAN_POINT('Ctrl Pts',(2.12219400142581,-0.41050867268925,5.));
#29730=CARTESIAN_POINT('Ctrl Pts',(2.09893248463381,-0.484741603770714,
5.));
#29731=CARTESIAN_POINT('Ctrl Pts',(2.07170317080282,-0.557614084834952,
5.));
#29732=CARTESIAN_POINT('Ctrl Pts',(2.04071024615788,-0.628834903151848,
5.));
#29733=CARTESIAN_POINT('Ctrl Pts',(2.00970031783733,-0.7000947954092,5.));
#29734=CARTESIAN_POINT('Ctrl Pts',(1.97492198177241,-0.769702049232439,
5.));
#29735=CARTESIAN_POINT('Ctrl Pts',(1.93653689050298,-0.837335602906435,
5.));
#29736=CARTESIAN_POINT('Ctrl Pts',(1.89892488427954,-0.903607000409294,
5.));
#29737=CARTESIAN_POINT('Ctrl Pts',(1.8578492344502,-0.967984023593398,5.));
#29738=CARTESIAN_POINT('Ctrl Pts',(1.81343121203445,-1.03012582810539,5.));
#29739=CARTESIAN_POINT('Ctrl Pts',(1.79641142470554,-1.05393689036138,5.));
#29740=CARTESIAN_POINT('Ctrl Pts',(1.77890063322063,-1.07741931484657,5.));
#29741=CARTESIAN_POINT('Ctrl Pts',(1.76090475095969,-1.10055208232734,5.));
#29742=CARTESIAN_POINT('Ctrl Pts',(1.75328563734958,-1.11034605524828,5.));
#29743=CARTESIAN_POINT('Ctrl Pts',(1.7455793850169,-1.12007743144322,5.00000000000001));
#29744=CARTESIAN_POINT('Ctrl Pts',(1.7377958257542,-1.12973327713713,5.00000000000001));
#29745=CARTESIAN_POINT('Ctrl Pts',(1.69072775812267,-1.18812327364407,5.));
#29746=CARTESIAN_POINT('Ctrl Pts',(1.64075413084026,-1.24386031821466,5.));
#29747=CARTESIAN_POINT('Ctrl Pts',(1.58802770749618,-1.29665904591518,5.));
#29748=CARTESIAN_POINT('Ctrl Pts',(1.53615683351676,-1.34860105102627,5.));
#29749=CARTESIAN_POINT('Ctrl Pts',(1.48162111426943,-1.39769987612691,5.));
#29750=CARTESIAN_POINT('Ctrl Pts',(1.42453922398786,-1.44364191562489,5.));
#29751=CARTESIAN_POINT('Ctrl Pts',(1.36928567044666,-1.48811242854364,5.));
#29752=CARTESIAN_POINT('Ctrl Pts',(1.31164585798449,-1.52962545660389,5.));
#29753=CARTESIAN_POINT('Ctrl Pts',(1.25171120792614,-1.56785089596259,5.));
#29754=CARTESIAN_POINT('Ctrl Pts',(1.22182449225738,-1.58691220417603,5.00000000000001));
#29755=CARTESIAN_POINT('Ctrl Pts',(1.19136694642474,-1.60515527938473,5.));
#29756=CARTESIAN_POINT('Ctrl Pts',(1.16034898466907,-1.62253437445174,5.));
#29757=CARTESIAN_POINT('Origin',(-0.860389557721271,-5.43228587327326,0.));
#29758=CARTESIAN_POINT('',(-1.10635903124561,-5.38757549311203,4.));
#29759=CARTESIAN_POINT('',(-0.61264241982148,-5.46577252229136,4.));
#29760=CARTESIAN_POINT('Ctrl Pts',(-1.1063590312456,-5.38757549311203,4.));
#29761=CARTESIAN_POINT('Ctrl Pts',(-1.1063590312456,-5.38757549311203,4.02673063961774));
#29762=CARTESIAN_POINT('Ctrl Pts',(-1.10617564982983,-5.38651975223822,
4.05414638576014));
#29763=CARTESIAN_POINT('Ctrl Pts',(-1.10402140302146,-5.37551658340327,
4.19012241323847));
#29764=CARTESIAN_POINT('Ctrl Pts',(-1.09908519447304,-5.35042611089804,
4.2868635932903));
#29765=CARTESIAN_POINT('Ctrl Pts',(-1.0731593931695,-5.29897209514011,4.42646405387435));
#29766=CARTESIAN_POINT('Ctrl Pts',(-1.05808598501925,-5.27637155422115,
4.47482705790044));
#29767=CARTESIAN_POINT('Ctrl Pts',(-1.02277290612915,-5.24115473829855,
4.54353143773206));
#29768=CARTESIAN_POINT('Ctrl Pts',(-1.00509927187885,-5.22683772617801,
4.56934838942209));
#29769=CARTESIAN_POINT('Ctrl Pts',(-0.967491407182819,-5.2057010863751,
4.60714056402289));
#29770=CARTESIAN_POINT('Ctrl Pts',(-0.949946965001191,-5.19797165415639,
4.62089194101728));
#29771=CARTESIAN_POINT('Ctrl Pts',(-0.909396227292148,-5.18618243478151,
4.6438839467319));
#29772=CARTESIAN_POINT('Ctrl Pts',(-0.88662313686,-5.182496726827,4.65258978726599));
#29773=CARTESIAN_POINT('Ctrl Pts',(-0.854886118918664,-5.18223104137204,
4.65886310574997));
#29774=CARTESIAN_POINT('Ctrl Pts',(-0.84722203253019,-5.1825134084958,4.65995935047192));
#29775=CARTESIAN_POINT('Ctrl Pts',(-0.834941493334292,-5.18354193434975,
4.661036848069));
#29776=CARTESIAN_POINT('Ctrl Pts',(-0.830357414107847,-5.18405325452173,
4.66128876278954));
#29777=CARTESIAN_POINT('Ctrl Pts',(-0.821749396602631,-5.18525652141284,
4.6614766362689));
#29778=CARTESIAN_POINT('Ctrl Pts',(-0.81773045401176,-5.18591867583012,
4.66144660123003));
#29779=CARTESIAN_POINT('Ctrl Pts',(-0.808785506788643,-5.18761806734741,
4.66111486035927));
#29780=CARTESIAN_POINT('Ctrl Pts',(-0.803879954994015,-5.1887046972058,
4.6607514048391));
#29781=CARTESIAN_POINT('Ctrl Pts',(-0.789765163415022,-5.19227888074625,
4.65917598249655));
#29782=CARTESIAN_POINT('Ctrl Pts',(-0.780742800229034,-5.19512838427145,
4.65750148702093));
#29783=CARTESIAN_POINT('Ctrl Pts',(-0.750108423554742,-5.20670671111326,
4.64948528566701));
#29784=CARTESIAN_POINT('Ctrl Pts',(-0.730633160772477,-5.21757743244348,
4.64009844156317));
#29785=CARTESIAN_POINT('Ctrl Pts',(-0.696424921417121,-5.24236094114524,
4.61539308723158));
#29786=CARTESIAN_POINT('Ctrl Pts',(-0.682131617948138,-5.25606733420563,
4.60019195379195));
#29787=CARTESIAN_POINT('Ctrl Pts',(-0.654795226139854,-5.28804986143137,
4.56080656181527));
#29788=CARTESIAN_POINT('Ctrl Pts',(-0.643602532663009,-5.30634185619752,
4.53533737515853));
#29789=CARTESIAN_POINT('Ctrl Pts',(-0.623508365378195,-5.34786498829097,
4.46952174021342));
#29790=CARTESIAN_POINT('Ctrl Pts',(-0.616850747770232,-5.37181868573423,
4.42457618200303));
#29791=CARTESIAN_POINT('Ctrl Pts',(-0.606819121617709,-5.43514820992187,
4.27073174534983));
#29792=CARTESIAN_POINT('Ctrl Pts',(-0.6126424198215,-5.46577252229136,4.14407324412986));
#29793=CARTESIAN_POINT('Ctrl Pts',(-0.6126424198215,-5.46577252229136,4.));
#29794=CARTESIAN_POINT('',(-1.10635903124561,-5.38757549311203,0.));
#29795=CARTESIAN_POINT('',(-1.10635903124561,-5.38757549311203,0.));
#29796=CARTESIAN_POINT('',(-0.61264241982148,-5.46577252229136,0.));
#29797=CARTESIAN_POINT('Origin',(-0.860389557721271,-5.43228587327326,0.));
#29798=CARTESIAN_POINT('',(-0.61264241982148,-5.46577252229136,0.));
#29799=CARTESIAN_POINT('Origin',(-1.69959346906221,-5.23081083962335,0.));
#29800=CARTESIAN_POINT('',(-1.93554040580225,-5.14817281542751,4.));
#29801=CARTESIAN_POINT('',(-1.46013497556791,-5.30264140340673,4.));
#29802=CARTESIAN_POINT('Ctrl Pts',(-1.93554040580225,-5.14817281542751,
4.));
#29803=CARTESIAN_POINT('Ctrl Pts',(-1.93554040580225,-5.14817281542751,
4.02673063961772));
#29804=CARTESIAN_POINT('Ctrl Pts',(-1.93519412785719,-5.14715875964944,
4.05414638576009));
#29805=CARTESIAN_POINT('Ctrl Pts',(-1.93134512857136,-5.1366280565286,4.19012241323843));
#29806=CARTESIAN_POINT('Ctrl Pts',(-1.92254467829738,-5.11261868251876,
4.28686359329027));
#29807=CARTESIAN_POINT('Ctrl Pts',(-1.88888888520001,-5.0658538399355,4.42646405387438));
#29808=CARTESIAN_POINT('Ctrl Pts',(-1.87046555218869,-5.04588954971901,
4.47482705790046));
#29809=CARTESIAN_POINT('Ctrl Pts',(-1.83007811213918,-5.01663049384449,
4.54353143773204));
#29810=CARTESIAN_POINT('Ctrl Pts',(-1.81038239552216,-5.00525451342013,
4.56934838942208));
#29811=CARTESIAN_POINT('Ctrl Pts',(-1.76993104710689,-4.99026126692246,
4.6071405640229));
#29812=CARTESIAN_POINT('Ctrl Pts',(-1.75139345652765,-4.98537155226774,
4.62089194101727));
#29813=CARTESIAN_POINT('Ctrl Pts',(-1.70949772546375,-4.98007101070696,
4.64388394673189));
#29814=CARTESIAN_POINT('Ctrl Pts',(-1.68642843781244,-4.97999317615251,
4.65258978726598));
#29815=CARTESIAN_POINT('Ctrl Pts',(-1.65504059286453,-4.98469552515,4.65886310574996));
#29816=CARTESIAN_POINT('Ctrl Pts',(-1.64751503604726,-4.98617334312011,
4.65995935047191));
#29817=CARTESIAN_POINT('Ctrl Pts',(-1.63554658755897,-4.98911030569358,
4.66103684806899));
#29818=CARTESIAN_POINT('Ctrl Pts',(-1.63109893405222,-4.99033243864725,
4.66128876278954));
#29819=CARTESIAN_POINT('Ctrl Pts',(-1.6227851279391,-4.9928674819397,4.66147663626889));
#29820=CARTESIAN_POINT('Ctrl Pts',(-1.61891924897263,-4.99415018527155,
4.66144660123003));
#29821=CARTESIAN_POINT('Ctrl Pts',(-1.610350272296,-4.99722795249295,4.66111486035926));
#29822=CARTESIAN_POINT('Ctrl Pts',(-1.60567510234486,-4.99906860150534,
4.6607514048391));
#29823=CARTESIAN_POINT('Ctrl Pts',(-1.59229321276246,-5.00480682078521,
4.65917598249655));
#29824=CARTESIAN_POINT('Ctrl Pts',(-1.58382769039864,-5.00903265075193,
4.65750148702093));
#29825=CARTESIAN_POINT('Ctrl Pts',(-1.5553817231016,-5.02526070150406,4.64948528566701));
#29826=CARTESIAN_POINT('Ctrl Pts',(-1.53784678859742,-5.03904418853065,
4.64009844156316));
#29827=CARTESIAN_POINT('Ctrl Pts',(-1.50793670435943,-5.06887391873794,
4.61539308723157));
#29828=CARTESIAN_POINT('Ctrl Pts',(-1.49596352744056,-5.08464752863713,
4.60019195379194));
#29829=CARTESIAN_POINT('Ctrl Pts',(-1.47396686151477,-5.12051265170942,
4.56080656181526));
#29830=CARTESIAN_POINT('Ctrl Pts',(-1.4657734670836,-5.14033036468258,4.53533737515852));
#29831=CARTESIAN_POINT('Ctrl Pts',(-1.45242234129827,-5.18448569842586,
4.46952174021348));
#29832=CARTESIAN_POINT('Ctrl Pts',(-1.449593873856,-5.20918596695366,4.42457618200312));
#29833=CARTESIAN_POINT('Ctrl Pts',(-1.44959267390549,-5.27330509167993,
4.2707317453498));
#29834=CARTESIAN_POINT('Ctrl Pts',(-1.46013497556793,-5.30264140340673,
4.14407324412983));
#29835=CARTESIAN_POINT('Ctrl Pts',(-1.46013497556793,-5.30264140340673,
4.));
#29836=CARTESIAN_POINT('',(-1.93554040580225,-5.14817281542751,0.));
#29837=CARTESIAN_POINT('',(-1.93554040580225,-5.14817281542751,0.));
#29838=CARTESIAN_POINT('',(-1.46013497556791,-5.30264140340673,0.));
#29839=CARTESIAN_POINT('Origin',(-1.69959346906221,-5.23081083962335,0.));
#29840=CARTESIAN_POINT('',(-1.46013497556791,-5.30264140340673,0.));
#29841=CARTESIAN_POINT('Origin',(-2.49694774856751,-4.90053588303602,0.));
#29842=CARTESIAN_POINT('',(-2.71706235187773,-4.78200503722117,4.));
#29843=CARTESIAN_POINT('',(-2.2716741623057,-5.00894165471237,4.));
#29844=CARTESIAN_POINT('Ctrl Pts',(-2.71706235187773,-4.78200503722117,
4.));
#29845=CARTESIAN_POINT('Ctrl Pts',(-2.71706235187773,-4.78200503722117,
4.02673063961772));
#29846=CARTESIAN_POINT('Ctrl Pts',(-2.71656170391563,-4.78105763595755,
4.0541463857601));
#29847=CARTESIAN_POINT('Ctrl Pts',(-2.71111272728885,-4.77125869941104,
4.19012241323842));
#29848=CARTESIAN_POINT('Ctrl Pts',(-2.69866473158208,-4.74892161436726,
4.28686359329027));
#29849=CARTESIAN_POINT('Ctrl Pts',(-2.65810766401411,-4.70799745058668,
4.4264640538744));
#29850=CARTESIAN_POINT('Ctrl Pts',(-2.636788049744,-4.69116099815549,4.47482705790047));
#29851=CARTESIAN_POINT('Ctrl Pts',(-2.59232072134732,-4.6685801573899,4.54353143773204));
#29852=CARTESIAN_POINT('Ctrl Pts',(-2.57108789627303,-4.66042532305449,
4.56934838942208));
#29853=CARTESIAN_POINT('Ctrl Pts',(-2.52878911058682,-4.65194465335057,
4.60714056402291));
#29854=CARTESIAN_POINT('Ctrl Pts',(-2.50971482861277,-4.65001505726266,
4.62089194101728));
#29855=CARTESIAN_POINT('Ctrl Pts',(-2.46750571613677,-4.65133371044068,
4.64388394673189));
#29856=CARTESIAN_POINT('Ctrl Pts',(-2.44470827369085,-4.65486566583135,
4.65258978726599));
#29857=CARTESIAN_POINT('Ctrl Pts',(-2.4144424746492,-4.66442026184278,4.65886310574998));
#29858=CARTESIAN_POINT('Ctrl Pts',(-2.4072407515879,-4.66705714187622,4.65995935047192));
#29859=CARTESIAN_POINT('Ctrl Pts',(-2.39587909673009,-4.67183022340341,
4.661036848069));
#29860=CARTESIAN_POINT('Ctrl Pts',(-2.39167738493325,-4.67373307616942,
4.66128876278955));
#29861=CARTESIAN_POINT('Ctrl Pts',(-2.38386250371065,-4.67753747468404,
4.6614766362689));
#29862=CARTESIAN_POINT('Ctrl Pts',(-2.38024487913883,-4.67940914251738,
4.66144660123004));
#29863=CARTESIAN_POINT('Ctrl Pts',(-2.37226286965329,-4.68378950059938,
4.66111486035927));
#29864=CARTESIAN_POINT('Ctrl Pts',(-2.36793319974582,-4.68633884587832,
4.66075140483911));
#29865=CARTESIAN_POINT('Ctrl Pts',(-2.35561371869349,-4.69409980689487,
4.65917598249656));
#29866=CARTESIAN_POINT('Ctrl Pts',(-2.34791348640789,-4.69959790934462,
4.65750148702093));
#29867=CARTESIAN_POINT('Ctrl Pts',(-2.32235636260971,-4.72007609553974,
4.64948528566702));
#29868=CARTESIAN_POINT('Ctrl Pts',(-2.30719352466623,-4.73643295306732,
4.64009844156317));
#29869=CARTESIAN_POINT('Ctrl Pts',(-2.28231808108542,-4.77057439782324,
4.61539308723158));
#29870=CARTESIAN_POINT('Ctrl Pts',(-2.2729598500691,-4.7880268259359,4.60019195379196));
#29871=CARTESIAN_POINT('Ctrl Pts',(-2.25684454094365,-4.82689142649518,
4.56080656181528));
#29872=CARTESIAN_POINT('Ctrl Pts',(-2.25185219412135,-4.84774687981073,
4.53533737515855));
#29873=CARTESIAN_POINT('Ctrl Pts',(-2.24557285886215,-4.89344716434407,
4.46952174021337));
#29874=CARTESIAN_POINT('Ctrl Pts',(-2.2466431878412,-4.91828580136974,4.42457618200295));
#29875=CARTESIAN_POINT('Ctrl Pts',(-2.25667244363945,-4.98161570098457,
4.27073174534984));
#29876=CARTESIAN_POINT('Ctrl Pts',(-2.27167416230572,-5.00894165471236,
4.14407324412988));
#29877=CARTESIAN_POINT('Ctrl Pts',(-2.27167416230572,-5.00894165471236,
4.));
#29878=CARTESIAN_POINT('',(-2.71706235187773,-4.78200503722117,0.));
#29879=CARTESIAN_POINT('',(-2.71706235187773,-4.78200503722117,0.));
#29880=CARTESIAN_POINT('',(-2.2716741623057,-5.00894165471237,0.));
#29881=CARTESIAN_POINT('Origin',(-2.49694774856751,-4.90053588303602,0.));
#29882=CARTESIAN_POINT('',(-2.2716741623057,-5.00894165471237,0.));
#29883=CARTESIAN_POINT('Origin',(-3.2328188876086,-4.44959346906221,0.));
#29884=CARTESIAN_POINT('',(-3.43168120543702,-4.29808842443363,4.));
#29885=CARTESIAN_POINT('',(-3.02727719191323,-4.59190513875472,4.));
#29886=CARTESIAN_POINT('Ctrl Pts',(-3.43168120543702,-4.29808842443363,
4.));
#29887=CARTESIAN_POINT('Ctrl Pts',(-3.43168120543702,-4.29808842443363,
4.02673063961774));
#29888=CARTESIAN_POINT('Ctrl Pts',(-3.43103851507225,-4.2972310058478,4.05414638576013));
#29889=CARTESIAN_POINT('Ctrl Pts',(-3.42412373299319,-4.28840511821421,
4.19012241323849));
#29890=CARTESIAN_POINT('Ctrl Pts',(-3.40833470282043,-4.26829033530279,
4.28686359329032));
#29891=CARTESIAN_POINT('Ctrl Pts',(-3.36187501038667,-4.23421453905677,
4.4264640538742));
#29892=CARTESIAN_POINT('Ctrl Pts',(-3.33818407451688,-4.22092049374668,
4.47482705790034));
#29893=CARTESIAN_POINT('Ctrl Pts',(-3.29073179097662,-4.20557388333114,
4.54353143773207));
#29894=CARTESIAN_POINT('Ctrl Pts',(-3.2684846800661,-4.20084099417036,4.5693483894221));
#29895=CARTESIAN_POINT('Ctrl Pts',(-3.2253799935942,-4.19908172349404,4.60714056402291));
#29896=CARTESIAN_POINT('Ctrl Pts',(-3.20623869235145,-4.20015975903259,
4.62089194101729));
#29897=CARTESIAN_POINT('Ctrl Pts',(-3.16475552689651,-4.20806513733182,
4.6438839467319));
#29898=CARTESIAN_POINT('Ctrl Pts',(-3.14279127834937,-4.215119914204,4.65258978726599));
#29899=CARTESIAN_POINT('Ctrl Pts',(-3.11439276963288,-4.22929149136568,
4.65886310574998));
#29900=CARTESIAN_POINT('Ctrl Pts',(-3.10769221065044,-4.23302250472472,
4.65995935047192));
#29901=CARTESIAN_POINT('Ctrl Pts',(-3.09721711107279,-4.23951417609749,
4.661036848069));
#29902=CARTESIAN_POINT('Ctrl Pts',(-3.09336480107502,-4.24205089412554,
4.66128876278955));
#29903=CARTESIAN_POINT('Ctrl Pts',(-3.08624127305476,-4.24703097094482,
4.6614766362689));
#29904=CARTESIAN_POINT('Ctrl Pts',(-3.08296098080076,-4.24944551660589,
4.66144660123004));
#29905=CARTESIAN_POINT('Ctrl Pts',(-3.07576248207062,-4.25502060659492,
4.66111486035927));
#29906=CARTESIAN_POINT('Ctrl Pts',(-3.0718849230493,-4.25821587479886,4.66075140483911));
#29907=CARTESIAN_POINT('Ctrl Pts',(-3.06093119703656,-4.26780847693471,
4.65917598249656));
#29908=CARTESIAN_POINT('Ctrl Pts',(-3.05418586010366,-4.274443470338,4.65750148702094));
#29909=CARTESIAN_POINT('Ctrl Pts',(-3.03214688101148,-4.2986675510688,4.64948528566701));
#29910=CARTESIAN_POINT('Ctrl Pts',(-3.01972949902144,-4.31719501897975,
4.64009844156317));
#29911=CARTESIAN_POINT('Ctrl Pts',(-3.00050121207563,-4.35480750260545,
4.61539308723158));
#29912=CARTESIAN_POINT('Ctrl Pts',(-2.99398835766767,-4.37350901223015,
4.60019195379196));
#29913=CARTESIAN_POINT('Ctrl Pts',(-2.98415121773687,-4.41441611482645,
4.56080656181527));
#29914=CARTESIAN_POINT('Ctrl Pts',(-2.98248284667088,-4.43579577800849,
4.53533737515853));
#29915=CARTESIAN_POINT('Ctrl Pts',(-2.98342992001184,-4.48191572065595,
4.46952174021345));
#29916=CARTESIAN_POINT('Ctrl Pts',(-2.98837269036046,-4.50628111650125,
4.42457618200307));
#29917=CARTESIAN_POINT('Ctrl Pts',(-3.00818544834456,-4.56726239869638,
4.27073174534983));
#29918=CARTESIAN_POINT('Ctrl Pts',(-3.02727719191324,-4.59190513875471,
4.14407324412986));
#29919=CARTESIAN_POINT('Ctrl Pts',(-3.02727719191324,-4.59190513875471,
4.));
#29920=CARTESIAN_POINT('',(-3.43168120543702,-4.29808842443363,0.));
#29921=CARTESIAN_POINT('',(-3.43168120543702,-4.29808842443363,0.));
#29922=CARTESIAN_POINT('',(-3.02727719191323,-4.59190513875472,0.));
#29923=CARTESIAN_POINT('Origin',(-3.2328188876086,-4.44959346906221,0.));
#29924=CARTESIAN_POINT('',(-3.02727719191323,-4.59190513875472,0.));
#29925=CARTESIAN_POINT('Origin',(-3.88908729652601,-3.88908729652601,0.));
#29926=CARTESIAN_POINT('',(-4.0618006786215,-3.70833861009886,4.));
#29927=CARTESIAN_POINT('',(-3.70833861009886,-4.06180067862149,4.));
#29928=CARTESIAN_POINT('Ctrl Pts',(-4.06180067862149,-3.70833861009886,
4.));
#29929=CARTESIAN_POINT('Ctrl Pts',(-4.06180067862149,-3.70833861009886,
4.02673063961774));
#29930=CARTESIAN_POINT('Ctrl Pts',(-4.06103177102382,-3.70759228668204,
4.05414638576013));
#29931=CARTESIAN_POINT('Ctrl Pts',(-4.0528214483761,-3.69995677060634,4.1901224132385));
#29932=CARTESIAN_POINT('Ctrl Pts',(-4.03408016206102,-3.68255958253971,
4.28686359329032));
#29933=CARTESIAN_POINT('Ctrl Pts',(-3.98286183657994,-3.6561712130228,4.42646405387434));
#29934=CARTESIAN_POINT('Ctrl Pts',(-3.95738292857724,-3.64674691834979,
4.47482705790044));
#29935=CARTESIAN_POINT('Ctrl Pts',(-3.90811412259944,-3.63901242276528,
4.54353143773206));
#29936=CARTESIAN_POINT('Ctrl Pts',(-3.88540052355723,-3.63781801821782,
4.5693483894221));
#29937=CARTESIAN_POINT('Ctrl Pts',(-3.84255131673681,-3.64282346565183,
4.60714056402291));
#29938=CARTESIAN_POINT('Ctrl Pts',(-3.8238143185883,-3.64688258800408,4.62089194101729));
#29939=CARTESIAN_POINT('Ctrl Pts',(-3.78407855336265,-3.66118003477435,
4.6438839467319));
#29940=CARTESIAN_POINT('Ctrl Pts',(-3.76348833140868,-3.67158392110798,
4.65258978726599));
#29941=CARTESIAN_POINT('Ctrl Pts',(-3.73765637855118,-3.69002352815742,
4.65886310574998));
#29942=CARTESIAN_POINT('Ctrl Pts',(-3.73162197364763,-3.69475680491064,
4.65995935047192));
#29943=CARTESIAN_POINT('Ctrl Pts',(-3.72229136106663,-3.70280721963518,
4.661036848069));
#29944=CARTESIAN_POINT('Ctrl Pts',(-3.71888330952516,-3.70591534050852,
4.66128876278955));
#29945=CARTESIAN_POINT('Ctrl Pts',(-3.71262653960873,-3.71194846961323,
4.6614766362689));
#29946=CARTESIAN_POINT('Ctrl Pts',(-3.70976435135453,-3.71484643897442,
4.66144660123004));
#29947=CARTESIAN_POINT('Ctrl Pts',(-3.70352661430895,-3.72147898365232,
4.66111486035927));
#29948=CARTESIAN_POINT('Ctrl Pts',(-3.70019664454577,-3.72524149667359,
4.66075140483911));
#29949=CARTESIAN_POINT('Ctrl Pts',(-3.69087839066037,-3.73642953822814,
4.65917598249656));
#29950=CARTESIAN_POINT('Ctrl Pts',(-3.68525404166195,-3.74403804702711,
4.65750148702093));
#29951=CARTESIAN_POINT('Ctrl Pts',(-3.6672758800842,-3.77141154503088,4.64948528566701));
#29952=CARTESIAN_POINT('Ctrl Pts',(-3.65790971120312,-3.79165341557609,
4.64009844156317));
#29953=CARTESIAN_POINT('Ctrl Pts',(-3.64480204513195,-3.83181079389602,
4.61539308723158));
#29954=CARTESIAN_POINT('Ctrl Pts',(-3.6412949354228,-3.85130089179906,4.60019195379196));
#29955=CARTESIAN_POINT('Ctrl Pts',(-3.63797818771934,-3.89324322780355,
4.56080656181527));
#29956=CARTESIAN_POINT('Ctrl Pts',(-3.6396748732423,-3.9146206625895,4.53533737515852));
#29957=CARTESIAN_POINT('Ctrl Pts',(-3.64782503509459,-3.96002463729987,
4.46952174021346));
#29958=CARTESIAN_POINT('Ctrl Pts',(-3.65651853940272,-3.98331683505495,
4.42457618200308));
#29959=CARTESIAN_POINT('Ctrl Pts',(-3.68562694371632,-4.04044793827742,
4.27073174534979));
#29960=CARTESIAN_POINT('Ctrl Pts',(-3.70833861009888,-4.06180067862148,
4.14407324412981));
#29961=CARTESIAN_POINT('Ctrl Pts',(-3.70833861009888,-4.06180067862148,
4.));
#29962=CARTESIAN_POINT('',(-4.0618006786215,-3.70833861009886,0.));
#29963=CARTESIAN_POINT('',(-4.0618006786215,-3.70833861009886,0.));
#29964=CARTESIAN_POINT('',(-3.70833861009886,-4.06180067862149,0.));
#29965=CARTESIAN_POINT('Origin',(-3.88908729652601,-3.88908729652601,0.));
#29966=CARTESIAN_POINT('',(-3.70833861009886,-4.06180067862149,0.));
#29967=CARTESIAN_POINT('Origin',(-4.44959346906221,-3.2328188876086,0.));
#29968=CARTESIAN_POINT('',(-4.59190513875472,-3.02727719191322,4.));
#29969=CARTESIAN_POINT('',(-4.29808842443363,-3.43168120543702,4.));
#29970=CARTESIAN_POINT('Ctrl Pts',(-4.59190513875472,-3.02727719191322,
4.));
#29971=CARTESIAN_POINT('Ctrl Pts',(-4.59190513875472,-3.02727719191322,
4.02673063961772));
#29972=CARTESIAN_POINT('Ctrl Pts',(-4.59102894698104,-3.02666034062482,
4.05414638576009));
#29973=CARTESIAN_POINT('Ctrl Pts',(-4.58172524915676,-3.02040320785364,
4.1901224132384));
#29974=CARTESIAN_POINT('Ctrl Pts',(-4.56049317936721,-3.00615199113995,
4.28686359329025));
#29975=CARTESIAN_POINT('Ctrl Pts',(-4.50577738599604,-2.98810081758766,
4.42646405387439));
#29976=CARTESIAN_POINT('Ctrl Pts',(-4.47913788113512,-2.98277833096402,
4.47482705790046));
#29977=CARTESIAN_POINT('Ctrl Pts',(-4.42926571423673,-2.98284639916111,
4.54353143773203));
#29978=CARTESIAN_POINT('Ctrl Pts',(-4.40664491125336,-2.98521988943094,
4.56934838942208));
#29979=CARTESIAN_POINT('Ctrl Pts',(-4.3651062737647,-2.99686680424732,4.6071405640229));
#29980=CARTESIAN_POINT('Ctrl Pts',(-4.34723494578937,-3.00380706434951,
4.62089194101728));
#29981=CARTESIAN_POINT('Ctrl Pts',(-4.31022500720832,-3.02414452900082,
4.64388394673189));
#29982=CARTESIAN_POINT('Ctrl Pts',(-4.29151581144706,-3.03764134658585,
4.65258978726599));
#29983=CARTESIAN_POINT('Ctrl Pts',(-4.26888648285923,-3.05989493919994,
4.65886310574997));
#29984=CARTESIAN_POINT('Ctrl Pts',(-4.26366681911034,-3.06551393036483,
4.65995935047192));
#29985=CARTESIAN_POINT('Ctrl Pts',(-4.25571044417423,-3.07492486051285,
4.66103684806901));
#29986=CARTESIAN_POINT('Ctrl Pts',(-4.25283056862868,-3.07852785198032,
4.66128876278955));
#29987=CARTESIAN_POINT('Ctrl Pts',(-4.24759461925647,-3.08546547770909,
4.6614766362689));
#29988=CARTESIAN_POINT('Ctrl Pts',(-4.24522101157593,-3.08877551314693,
4.66144660123004));
#29989=CARTESIAN_POINT('Ctrl Pts',(-4.24009763000285,-3.09630219725155,
4.66111486035927));
#29990=CARTESIAN_POINT('Ctrl Pts',(-4.23739724440491,-3.1005393095325,4.66075140483911));
#29991=CARTESIAN_POINT('Ctrl Pts',(-4.22994390898303,-3.1130473037917,4.65917598249656));
#29992=CARTESIAN_POINT('Ctrl Pts',(-4.22557903805758,-3.12144198124853,
4.65750148702094));
#29993=CARTESIAN_POINT('Ctrl Pts',(-4.2121043759984,-3.15129087015696,4.64948528566702));
#29994=CARTESIAN_POINT('Ctrl Pts',(-4.20602004638866,-3.17274872130469,
4.64009844156318));
#29995=CARTESIAN_POINT('Ctrl Pts',(-4.19935575543264,-3.21446218638993,
4.61539308723159));
#29996=CARTESIAN_POINT('Ctrl Pts',(-4.19894074710277,-3.23426096167702,
4.60019195379196));
#29997=CARTESIAN_POINT('Ctrl Pts',(-4.20222606096277,-3.27620577157863,
4.56080656181528));
#29998=CARTESIAN_POINT('Ctrl Pts',(-4.20724602504612,-3.29705459457642,
4.53533737515853));
#29999=CARTESIAN_POINT('Ctrl Pts',(-4.22239859137612,-3.34062460480519,
4.46952174021345));
#30000=CARTESIAN_POINT('Ctrl Pts',(-4.2346287667156,-3.36227007325895,4.42457618200306));
#30001=CARTESIAN_POINT('Ctrl Pts',(-4.27231607183921,-3.41414424014012,
4.27073174534987));
#30002=CARTESIAN_POINT('Ctrl Pts',(-4.29808842443364,-3.431681205437,4.14407324412991));
#30003=CARTESIAN_POINT('Ctrl Pts',(-4.29808842443364,-3.431681205437,4.));
#30004=CARTESIAN_POINT('',(-4.59190513875472,-3.02727719191322,0.));
#30005=CARTESIAN_POINT('',(-4.59190513875472,-3.02727719191322,0.));
#30006=CARTESIAN_POINT('',(-4.29808842443363,-3.43168120543702,0.));
#30007=CARTESIAN_POINT('Origin',(-4.44959346906221,-3.2328188876086,0.));
#30008=CARTESIAN_POINT('',(-4.29808842443363,-3.43168120543702,0.));
#30009=CARTESIAN_POINT('Origin',(-4.90053588303603,-2.49694774856751,0.));
#30010=CARTESIAN_POINT('',(-5.00894165471237,-2.2716741623057,4.));
#30011=CARTESIAN_POINT('',(-4.78200503722117,-2.71706235187773,4.));
#30012=CARTESIAN_POINT('Ctrl Pts',(-5.00894165471237,-2.2716741623057,4.));
#30013=CARTESIAN_POINT('Ctrl Pts',(-5.00894165471237,-2.2716741623057,4.02673063961771));
#30014=CARTESIAN_POINT('Ctrl Pts',(-5.00797975351207,-2.27120197207165,
4.05414638576009));
#30015=CARTESIAN_POINT('Ctrl Pts',(-4.99781176842887,-2.26647729398004,
4.19012241323838));
#30016=CARTESIAN_POINT('Ctrl Pts',(-4.97461171918825,-2.25572296087186,
4.28686359329023));
#30017=CARTESIAN_POINT('Ctrl Pts',(-4.91774574235115,-2.24645346308547,
4.42646405387434));
#30018=CARTESIAN_POINT('Ctrl Pts',(-4.89060159365313,-2.24536384179618,
4.47482705790043));
#30019=CARTESIAN_POINT('Ctrl Pts',(-4.84135408409937,-2.25323279770997,
4.54353143773201));
#30020=CARTESIAN_POINT('Ctrl Pts',(-4.81938307641843,-2.25911573958947,
4.56934838942206));
#30021=CARTESIAN_POINT('Ctrl Pts',(-4.78017782737534,-2.27711733609156,
4.60714056402289));
#30022=CARTESIAN_POINT('Ctrl Pts',(-4.76361222097949,-2.28676784170657,
4.62089194101727));
#30023=CARTESIAN_POINT('Ctrl Pts',(-4.73023941655985,-2.31264454836302,
4.64388394673188));
#30024=CARTESIAN_POINT('Ctrl Pts',(-4.7138719294832,-2.32890196075715,4.65258978726598));
#30025=CARTESIAN_POINT('Ctrl Pts',(-4.69500243433731,-2.3544215816303,4.65886310574996));
#30026=CARTESIAN_POINT('Ctrl Pts',(-4.69072603718765,-2.36078792899601,
4.65995935047191));
#30027=CARTESIAN_POINT('Ctrl Pts',(-4.6843398122531,-2.37132764623413,4.66103684806899));
#30028=CARTESIAN_POINT('Ctrl Pts',(-4.68205902479715,-2.37533679068818,
4.66128876278954));
#30029=CARTESIAN_POINT('Ctrl Pts',(-4.67797282241978,-2.38300808567095,
4.66147663626889));
#30030=CARTESIAN_POINT('Ctrl Pts',(-4.67614624141154,-2.38664868312759,
4.66144660123003));
#30031=CARTESIAN_POINT('Ctrl Pts',(-4.67226336996884,-2.39488417471662,
4.66111486035926));
#30032=CARTESIAN_POINT('Ctrl Pts',(-4.67025906099163,-2.39949155449073,
4.6607514048391));
#30033=CARTESIAN_POINT('Ctrl Pts',(-4.66485416988756,-2.41301151312426,
4.65917598249655));
#30034=CARTESIAN_POINT('Ctrl Pts',(-4.66185625464343,-2.42198565441961,
4.65750148702092));
#30035=CARTESIAN_POINT('Ctrl Pts',(-4.65321688300255,-2.45357495552502,
4.64948528566701));
#30036=CARTESIAN_POINT('Ctrl Pts',(-4.65056420905188,-2.47572042376548,
4.64009844156316));
#30037=CARTESIAN_POINT('Ctrl Pts',(-4.65050739017188,-2.51796285166656,
4.61539308723158));
#30038=CARTESIAN_POINT('Ctrl Pts',(-4.6531947021037,-2.53758279278175,4.60019195379196));
#30039=CARTESIAN_POINT('Ctrl Pts',(-4.66300118219659,-2.57849725615388,
4.56080656181527));
#30040=CARTESIAN_POINT('Ctrl Pts',(-4.6712208166643,-2.59830410014803,4.53533737515853));
#30041=CARTESIAN_POINT('Ctrl Pts',(-4.69300268100046,-2.63896730764278,
4.46952174021343));
#30042=CARTESIAN_POINT('Ctrl Pts',(-4.70846837986481,-2.6584330635247,4.42457618200304));
#30043=CARTESIAN_POINT('Ctrl Pts',(-4.75380659926932,-2.70377297991549,
4.27073174534987));
#30044=CARTESIAN_POINT('Ctrl Pts',(-4.78200503722118,-2.71706235187771,
4.14407324412992));
#30045=CARTESIAN_POINT('Ctrl Pts',(-4.78200503722118,-2.71706235187771,
4.));
#30046=CARTESIAN_POINT('',(-5.00894165471237,-2.2716741623057,0.));
#30047=CARTESIAN_POINT('',(-5.00894165471237,-2.2716741623057,0.));
#30048=CARTESIAN_POINT('',(-4.78200503722117,-2.71706235187773,0.));
#30049=CARTESIAN_POINT('Origin',(-4.90053588303603,-2.49694774856751,0.));
#30050=CARTESIAN_POINT('',(-4.78200503722117,-2.71706235187773,0.));
#30051=CARTESIAN_POINT('Origin',(-5.23081083962335,-1.69959346906221,0.));
#30052=CARTESIAN_POINT('',(-5.30264140340673,-1.46013497556791,4.));
#30053=CARTESIAN_POINT('',(-5.14817281542751,-1.93554040580225,4.));
#30054=CARTESIAN_POINT('Ctrl Pts',(-5.30264140340673,-1.46013497556791,
4.));
#30055=CARTESIAN_POINT('Ctrl Pts',(-5.30264140340673,-1.46013497556791,
4.02673063961772));
#30056=CARTESIAN_POINT('Ctrl Pts',(-5.30161747797973,-1.45981907327888,
4.05414638576009));
#30057=CARTESIAN_POINT('Ctrl Pts',(-5.29083557517596,-1.45674318712176,
4.19012241323843));
#30058=CARTESIAN_POINT('Ctrl Pts',(-5.26623880869311,-1.4497505449918,4.28686359329027));
#30059=CARTESIAN_POINT('Ctrl Pts',(-5.20862287746719,-1.44949096877052,
4.42646405387427));
#30060=CARTESIAN_POINT('Ctrl Pts',(-5.1816424639593,-1.45266104290795,4.47482705790038));
#30061=CARTESIAN_POINT('Ctrl Pts',(-5.13423224887844,-1.46813712672828,
4.54353143773205));
#30062=CARTESIAN_POINT('Ctrl Pts',(-5.11345203562664,-1.47738466266403,
4.56934838942208));
#30063=CARTESIAN_POINT('Ctrl Pts',(-5.07754553837534,-1.50129768180205,
4.60714056402289));
#30064=CARTESIAN_POINT('Ctrl Pts',(-5.06269355376651,-1.51342080545345,
4.62089194101727));
#30065=CARTESIAN_POINT('Ctrl Pts',(-5.03377963271108,-1.54419958371732,
4.64388394673188));
#30066=CARTESIAN_POINT('Ctrl Pts',(-5.02015687617144,-1.56281727947213,
4.65258978726598));
#30067=CARTESIAN_POINT('Ctrl Pts',(-5.00551184406225,-1.59097455084368,
4.65886310574997));
#30068=CARTESIAN_POINT('Ctrl Pts',(-5.0022840126022,-1.59793149380938,4.65995935047191));
#30069=CARTESIAN_POINT('Ctrl Pts',(-4.99762518772176,-1.60934047531987,
4.66103684806899));
#30070=CARTESIAN_POINT('Ctrl Pts',(-4.99599964891207,-1.61365705431845,
4.66128876278954));
#30071=CARTESIAN_POINT('Ctrl Pts',(-4.99316380939342,-1.62187312581316,
4.6614766362689));
#30072=CARTESIAN_POINT('Ctrl Pts',(-4.99192923154399,-1.62575464169678,
4.66144660123003));
#30073=CARTESIAN_POINT('Ctrl Pts',(-4.98938247941308,-1.63449615563528,
4.66111486035926));
#30074=CARTESIAN_POINT('Ctrl Pts',(-4.98812359979553,-1.63936035392148,
4.6607514048391));
#30075=CARTESIAN_POINT('Ctrl Pts',(-4.98490023936606,-1.6535593706776,4.65917598249655));
#30076=CARTESIAN_POINT('Ctrl Pts',(-4.98334309842607,-1.66289200266933,
4.65750148702093));
#30077=CARTESIAN_POINT('Ctrl Pts',(-4.97975174720573,-1.69544388253963,
4.64948528566701));
#30078=CARTESIAN_POINT('Ctrl Pts',(-4.98059604655052,-1.71773167294815,
4.64009844156316));
#30079=CARTESIAN_POINT('Ctrl Pts',(-4.98714809881592,-1.75946291489558,
4.61539308723157));
#30080=CARTESIAN_POINT('Ctrl Pts',(-4.992871560471,-1.77842091377376,4.60019195379195));
#30081=CARTESIAN_POINT('Ctrl Pts',(-5.00895773871105,-1.81729758074086,
4.56080656181526));
#30082=CARTESIAN_POINT('Ctrl Pts',(-5.02017464888312,-1.83557473549708,
4.53533737515853));
#30083=CARTESIAN_POINT('Ctrl Pts',(-5.04804946943568,-1.87232987713589,
4.46952174021334));
#30084=CARTESIAN_POINT('Ctrl Pts',(-5.06636987499114,-1.88913660893299,
4.42457618200292));
#30085=CARTESIAN_POINT('Ctrl Pts',(-5.11824263124585,-1.9268258556173,4.27073174534982));
#30086=CARTESIAN_POINT('Ctrl Pts',(-5.14817281542752,-1.93554040580223,
4.14407324412985));
#30087=CARTESIAN_POINT('Ctrl Pts',(-5.14817281542752,-1.93554040580223,
4.));
#30088=CARTESIAN_POINT('',(-5.30264140340673,-1.46013497556791,0.));
#30089=CARTESIAN_POINT('',(-5.30264140340673,-1.46013497556791,0.));
#30090=CARTESIAN_POINT('',(-5.14817281542751,-1.93554040580225,0.));
#30091=CARTESIAN_POINT('Origin',(-5.23081083962335,-1.69959346906221,0.));
#30092=CARTESIAN_POINT('',(-5.14817281542751,-1.93554040580225,0.));
#30093=CARTESIAN_POINT('Origin',(-5.43228587327326,-0.860389557721269,0.));
#30094=CARTESIAN_POINT('',(-5.46577252229136,-0.612642419821477,4.));
#30095=CARTESIAN_POINT('',(-5.38757549311203,-1.1063590312456,4.));
#30096=CARTESIAN_POINT('Ctrl Pts',(-5.46577252229136,-0.612642419821477,
4.));
#30097=CARTESIAN_POINT('Ctrl Pts',(-5.46577252229136,-0.612642419821477,
4.02673063961772));
#30098=CARTESIAN_POINT('Ctrl Pts',(-5.46471178507989,-0.612490584040255,
4.0541463857601));
#30099=CARTESIAN_POINT('Ctrl Pts',(-5.45358145078565,-0.611139228343087,
4.19012241323848));
#30100=CARTESIAN_POINT('Ctrl Pts',(-5.42819362108337,-0.608080459247839,
4.28686359329031));
#30101=CARTESIAN_POINT('Ctrl Pts',(-5.37124643091165,-0.61683719621971,
4.42646405387439));
#30102=CARTESIAN_POINT('Ctrl Pts',(-5.34509409991729,-0.624188908037767,
4.47482705790046));
#30103=CARTESIAN_POINT('Ctrl Pts',(-5.30068857615023,-0.646891047218764,
4.54353143773204));
#30104=CARTESIAN_POINT('Ctrl Pts',(-5.2816108351434,-0.659275472185209,
4.56934838942208));
#30105=CARTESIAN_POINT('Ctrl Pts',(-5.24988722681302,-0.688511096065241,
4.6071405640229));
#30106=CARTESIAN_POINT('Ctrl Pts',(-5.23711456914321,-0.702808326214393,
4.62089194101728));
#30107=CARTESIAN_POINT('Ctrl Pts',(-5.21337148814816,-0.737731300415899,
4.64388394673189));
#30108=CARTESIAN_POINT('Ctrl Pts',(-5.20282889962289,-0.758250850073326,
4.65258978726599));
#30109=CARTESIAN_POINT('Ctrl Pts',(-5.19276893984501,-0.788352446473459,
4.65886310574997));
#30110=CARTESIAN_POINT('Ctrl Pts',(-5.19066915399765,-0.795728682014567,
4.65995935047192));
#30111=CARTESIAN_POINT('Ctrl Pts',(-5.1878524449016,-0.807726000808509,
4.661036848069));
#30112=CARTESIAN_POINT('Ctrl Pts',(-5.18692218089855,-0.812243725850724,
4.66128876278954));
#30113=CARTESIAN_POINT('Ctrl Pts',(-5.1854065320192,-0.82080226690951,4.6614766362689));
#30114=CARTESIAN_POINT('Ctrl Pts',(-5.18479435673256,-0.824829125416977,
4.66144660123004));
#30115=CARTESIAN_POINT('Ctrl Pts',(-5.18364643340307,-0.833861416620456,
4.66111486035927));
#30116=CARTESIAN_POINT('Ctrl Pts',(-5.18316398093936,-0.8388626607136,4.6607514048391));
#30117=CARTESIAN_POINT('Ctrl Pts',(-5.18220152101598,-0.853391108675958,
4.65917598249656));
#30118=CARTESIAN_POINT('Ctrl Pts',(-5.18212349635793,-0.86285243099119,
4.65750148702093));
#30119=CARTESIAN_POINT('Ctrl Pts',(-5.18366859654418,-0.895565354310466,
4.64948528566701));
#30120=CARTESIAN_POINT('Ctrl Pts',(-5.18798907973249,-0.917446667518258,
4.64009844156316));
#30121=CARTESIAN_POINT('Ctrl Pts',(-5.2009886698715,-0.957639161837225,
4.61539308723158));
#30122=CARTESIAN_POINT('Ctrl Pts',(-5.20960735062881,-0.975468409628027,
4.60019195379196));
#30123=CARTESIAN_POINT('Ctrl Pts',(-5.23157713192079,-1.01135000762512,
4.56080656181526));
#30124=CARTESIAN_POINT('Ctrl Pts',(-5.245515120242,-1.02764742893492,4.53533737515851));
#30125=CARTESIAN_POINT('Ctrl Pts',(-5.27879652641764,-1.05958947114722,
4.46952174021343));
#30126=CARTESIAN_POINT('Ctrl Pts',(-5.2995205294775,-1.07332334134435,4.42457618200303));
#30127=CARTESIAN_POINT('Ctrl Pts',(-5.35665054316768,-1.10243388398541,
4.27073174534983));
#30128=CARTESIAN_POINT('Ctrl Pts',(-5.38757549311203,-1.10635903124558,
4.14407324412986));
#30129=CARTESIAN_POINT('Ctrl Pts',(-5.38757549311203,-1.10635903124558,
4.));
#30130=CARTESIAN_POINT('',(-5.46577252229136,-0.612642419821477,0.));
#30131=CARTESIAN_POINT('',(-5.46577252229136,-0.612642419821477,0.));
#30132=CARTESIAN_POINT('',(-5.38757549311203,-1.1063590312456,0.));
#30133=CARTESIAN_POINT('Origin',(-5.43228587327326,-0.860389557721269,0.));
#30134=CARTESIAN_POINT('',(-5.38757549311203,-1.1063590312456,0.));
#30135=CARTESIAN_POINT('Origin',(-5.5,1.11022302462516E-15,0.));
#30136=CARTESIAN_POINT('',(-5.49431818181818,0.249935425544578,4.));
#30137=CARTESIAN_POINT('',(-5.25,-6.78278558411441E-16,4.66143782776615));
#30138=CARTESIAN_POINT('Ctrl Pts',(-5.49431818181818,0.249935425544578,
4.));
#30139=CARTESIAN_POINT('Ctrl Pts',(-5.49431818181818,0.249935425544578,
4.1114335267762));
#30140=CARTESIAN_POINT('Ctrl Pts',(-5.4756767400248,0.250197727297926,4.21120478468484));
#30141=CARTESIAN_POINT('Ctrl Pts',(-5.42857544323548,0.240569456691875,
4.36489144191036));
#30142=CARTESIAN_POINT('Ctrl Pts',(-5.4017694101364,0.232168981737913,4.425924297522));
#30143=CARTESIAN_POINT('Ctrl Pts',(-5.354112808079,0.204293630300537,4.51536926219335));
#30144=CARTESIAN_POINT('Ctrl Pts',(-5.33487327574923,0.189393579953126,
4.54624819863964));
#30145=CARTESIAN_POINT('Ctrl Pts',(-5.30503927476288,0.157570272463533,
4.59049297273665));
#30146=CARTESIAN_POINT('Ctrl Pts',(-5.29273012882291,0.141503389631088,
4.6074172319051));
#30147=CARTESIAN_POINT('Ctrl Pts',(-5.27400968904813,0.108133425552988,
4.63197965561651));
#30148=CARTESIAN_POINT('Ctrl Pts',(-5.26698529556665,0.0923722545750434,
4.64078922803164));
#30149=CARTESIAN_POINT('Ctrl Pts',(-5.25718642825102,0.0612525257750982,
4.65284375994342));
#30150=CARTESIAN_POINT('Ctrl Pts',(-5.25391607094643,0.0466559930935807,
4.65676521233374));
#30151=CARTESIAN_POINT('Ctrl Pts',(-5.25122338487753,0.0254407476598933,
4.65998297001336));
#30152=CARTESIAN_POINT('Ctrl Pts',(-5.25067352981899,0.0193427404519049,
4.66063713008572));
#30153=CARTESIAN_POINT('Ctrl Pts',(-5.25012437329208,0.00895709567438105,
4.66129014831286));
#30154=CARTESIAN_POINT('Ctrl Pts',(-5.25000782702704,0.00470041714920988,
4.66142853012161));
#30155=CARTESIAN_POINT('Ctrl Pts',(-5.25000012706038,0.00029104482780982,
4.66143767683269));
#30156=CARTESIAN_POINT('Ctrl Pts',(-5.25,0.000145522242130993,4.66143782776615));
#30157=CARTESIAN_POINT('Ctrl Pts',(-5.25,-7.13617547270521E-16,4.66143782776615));
#30158=CARTESIAN_POINT('',(-5.49431818181818,0.249935425544578,0.));
#30159=CARTESIAN_POINT('',(-5.49431818181818,0.249935425544578,0.));
#30160=CARTESIAN_POINT('',(-5.49431818181818,-0.249935425544576,0.));
#30161=CARTESIAN_POINT('Origin',(-5.5,1.11022302462516E-15,0.));
#30162=CARTESIAN_POINT('',(-5.49431818181818,-0.249935425544576,4.));
#30163=CARTESIAN_POINT('',(-5.49431818181818,-0.249935425544576,0.));
#30164=CARTESIAN_POINT('Ctrl Pts',(-5.25,-7.13617547270521E-16,4.66143782776615));
#30165=CARTESIAN_POINT('Ctrl Pts',(-5.25,-0.00401273696638705,4.66143782776615));
#30166=CARTESIAN_POINT('Ctrl Pts',(-5.25009663683444,-0.00802521271127695,
4.6613230837511));
#30167=CARTESIAN_POINT('Ctrl Pts',(-5.25057191524974,-0.0178887267944777,
4.66075801609034));
#30168=CARTESIAN_POINT('Ctrl Pts',(-5.25105929530591,-0.0237157972436869,
4.66017835073772));
#30169=CARTESIAN_POINT('Ctrl Pts',(-5.25327427371658,-0.0423565274659345,
4.65753338733037));
#30170=CARTESIAN_POINT('Ctrl Pts',(-5.25577300860231,-0.0548474302584322,
4.65454084811324));
#30171=CARTESIAN_POINT('Ctrl Pts',(-5.26513174003141,-0.0885738625581881,
4.64311349551522));
#30172=CARTESIAN_POINT('Ctrl Pts',(-5.27370766679928,-0.108104477794349,
4.63244216484639));
#30173=CARTESIAN_POINT('Ctrl Pts',(-5.29504707030263,-0.144948043057416,
4.60428833810774));
#30174=CARTESIAN_POINT('Ctrl Pts',(-5.30802661494925,-0.161251465092565,
4.58628814678021));
#30175=CARTESIAN_POINT('Ctrl Pts',(-5.33877014255047,-0.192707055001167,
4.54008611674082));
#30176=CARTESIAN_POINT('Ctrl Pts',(-5.35671971365448,-0.205776251869831,
4.51041431850453));
#30177=CARTESIAN_POINT('Ctrl Pts',(-5.40048917407278,-0.231487544890781,
4.42842633637123));
#30178=CARTESIAN_POINT('Ctrl Pts',(-5.42658774433484,-0.239954791804268,
4.36954193373565));
#30179=CARTESIAN_POINT('Ctrl Pts',(-5.47416618476358,-0.250126227193806,
4.21822112899257));
#30180=CARTESIAN_POINT('Ctrl Pts',(-5.49431818181814,-0.249935425544575,
4.11550482956185));
#30181=CARTESIAN_POINT('Ctrl Pts',(-5.49431818181818,-0.249935425544576,
4.00000000000038));
#30182=CARTESIAN_POINT('Origin',(-5.43228587327326,0.860389557721271,0.));
#30183=CARTESIAN_POINT('',(-5.38757549311203,1.10635903124561,4.));
#30184=CARTESIAN_POINT('',(-5.46577252229136,0.61264241982148,4.));
#30185=CARTESIAN_POINT('Ctrl Pts',(-5.38757549311203,1.1063590312456,4.));
#30186=CARTESIAN_POINT('Ctrl Pts',(-5.38757549311203,1.1063590312456,4.02673063961772));
#30187=CARTESIAN_POINT('Ctrl Pts',(-5.38651975223822,1.10617564982983,4.05414638576011));
#30188=CARTESIAN_POINT('Ctrl Pts',(-5.37551658340328,1.10402140302146,4.19012241323843));
#30189=CARTESIAN_POINT('Ctrl Pts',(-5.35042611089805,1.09908519447304,4.28686359329027));
#30190=CARTESIAN_POINT('Ctrl Pts',(-5.29897209514017,1.07315939316953,4.42646405387417));
#30191=CARTESIAN_POINT('Ctrl Pts',(-5.27637155422121,1.05808598501931,4.47482705790032));
#30192=CARTESIAN_POINT('Ctrl Pts',(-5.24115473829857,1.02277290612916,4.54353143773204));
#30193=CARTESIAN_POINT('Ctrl Pts',(-5.22683772617802,1.00509927187887,4.56934838942207));
#30194=CARTESIAN_POINT('Ctrl Pts',(-5.2057010863751,0.967491407182816,4.6071405640229));
#30195=CARTESIAN_POINT('Ctrl Pts',(-5.1979716541564,0.949946965001195,4.62089194101727));
#30196=CARTESIAN_POINT('Ctrl Pts',(-5.18618243478152,0.909396227292173,
4.64388394673188));
#30197=CARTESIAN_POINT('Ctrl Pts',(-5.182496726827,0.886623136860021,4.65258978726598));
#30198=CARTESIAN_POINT('Ctrl Pts',(-5.18223104137204,0.854886118918676,
4.65886310574997));
#30199=CARTESIAN_POINT('Ctrl Pts',(-5.1825134084958,0.8472220325302,4.65995935047192));
#30200=CARTESIAN_POINT('Ctrl Pts',(-5.18354193434975,0.834941493334305,
4.661036848069));
#30201=CARTESIAN_POINT('Ctrl Pts',(-5.18405325452173,0.830357414107855,
4.66128876278954));
#30202=CARTESIAN_POINT('Ctrl Pts',(-5.18525652141284,0.821749396602635,
4.6614766362689));
#30203=CARTESIAN_POINT('Ctrl Pts',(-5.18591867583012,0.817730454011764,
4.66144660123003));
#30204=CARTESIAN_POINT('Ctrl Pts',(-5.18761806734741,0.808785506788655,
4.66111486035927));
#30205=CARTESIAN_POINT('Ctrl Pts',(-5.18870469720579,0.803879954994031,
4.6607514048391));
#30206=CARTESIAN_POINT('Ctrl Pts',(-5.19227888074625,0.789765163415027,
4.65917598249656));
#30207=CARTESIAN_POINT('Ctrl Pts',(-5.19512838427145,0.780742800229034,
4.65750148702093));
#30208=CARTESIAN_POINT('Ctrl Pts',(-5.20670671111325,0.750108423554761,
4.64948528566701));
#30209=CARTESIAN_POINT('Ctrl Pts',(-5.21757743244347,0.730633160772493,
4.64009844156318));
#30210=CARTESIAN_POINT('Ctrl Pts',(-5.24236094114524,0.696424921417127,
4.61539308723158));
#30211=CARTESIAN_POINT('Ctrl Pts',(-5.25606733420563,0.682131617948139,
4.60019195379195));
#30212=CARTESIAN_POINT('Ctrl Pts',(-5.28804986143135,0.654795226139872,
4.56080656181529));
#30213=CARTESIAN_POINT('Ctrl Pts',(-5.30634185619748,0.643602532663021,
4.53533737515858));
#30214=CARTESIAN_POINT('Ctrl Pts',(-5.34786498829106,0.623508365378145,
4.46952174021328));
#30215=CARTESIAN_POINT('Ctrl Pts',(-5.37181868573432,0.616850747770218,
4.42457618200282));
#30216=CARTESIAN_POINT('Ctrl Pts',(-5.43514820992185,0.606819121617711,
4.27073174534987));
#30217=CARTESIAN_POINT('Ctrl Pts',(-5.46577252229136,0.612642419821501,
4.14407324412992));
#30218=CARTESIAN_POINT('Ctrl Pts',(-5.46577252229136,0.612642419821501,
4.));
#30219=CARTESIAN_POINT('',(-5.38757549311203,1.10635903124561,0.));
#30220=CARTESIAN_POINT('',(-5.38757549311203,1.10635903124561,0.));
#30221=CARTESIAN_POINT('',(-5.46577252229136,0.61264241982148,0.));
#30222=CARTESIAN_POINT('Origin',(-5.43228587327326,0.860389557721271,0.));
#30223=CARTESIAN_POINT('',(-5.46577252229136,0.61264241982148,0.));
#30224=CARTESIAN_POINT('Origin',(-5.23081083962335,1.69959346906221,0.));
#30225=CARTESIAN_POINT('',(-5.14817281542751,1.93554040580225,4.));
#30226=CARTESIAN_POINT('',(-5.30264140340673,1.46013497556791,4.));
#30227=CARTESIAN_POINT('Ctrl Pts',(-5.14817281542751,1.93554040580225,4.));
#30228=CARTESIAN_POINT('Ctrl Pts',(-5.14817281542751,1.93554040580225,4.02673063961775));
#30229=CARTESIAN_POINT('Ctrl Pts',(-5.14715875964944,1.9351941278572,4.05414638576016));
#30230=CARTESIAN_POINT('Ctrl Pts',(-5.13662805652858,1.93134512857136,4.19012241323852));
#30231=CARTESIAN_POINT('Ctrl Pts',(-5.11261868251874,1.92254467829737,4.28686359329035));
#30232=CARTESIAN_POINT('Ctrl Pts',(-5.06585383993555,1.88888888520005,4.42646405387421));
#30233=CARTESIAN_POINT('Ctrl Pts',(-5.04588954971906,1.87046555218876,4.47482705790035));
#30234=CARTESIAN_POINT('Ctrl Pts',(-5.01663049384449,1.83007811213917,4.54353143773205));
#30235=CARTESIAN_POINT('Ctrl Pts',(-5.00525451342013,1.81038239552216,4.56934838942209));
#30236=CARTESIAN_POINT('Ctrl Pts',(-4.99026126692246,1.76993104710686,4.60714056402292));
#30237=CARTESIAN_POINT('Ctrl Pts',(-4.98537155226774,1.75139345652763,4.62089194101728));
#30238=CARTESIAN_POINT('Ctrl Pts',(-4.98007101070696,1.70949772546375,4.64388394673188));
#30239=CARTESIAN_POINT('Ctrl Pts',(-4.97999317615251,1.68642843781244,4.65258978726598));
#30240=CARTESIAN_POINT('Ctrl Pts',(-4.98469552515,1.6550405928645,4.65886310574997));
#30241=CARTESIAN_POINT('Ctrl Pts',(-4.98617334312012,1.64751503604724,4.65995935047191));
#30242=CARTESIAN_POINT('Ctrl Pts',(-4.98911030569358,1.635546587559,4.66103684806899));
#30243=CARTESIAN_POINT('Ctrl Pts',(-4.99033243864724,1.63109893405223,4.66128876278954));
#30244=CARTESIAN_POINT('Ctrl Pts',(-4.9928674819397,1.6227851279391,4.6614766362689));
#30245=CARTESIAN_POINT('Ctrl Pts',(-4.99415018527155,1.61891924897262,4.66144660123003));
#30246=CARTESIAN_POINT('Ctrl Pts',(-4.99722795249295,1.610350272296,4.66111486035926));
#30247=CARTESIAN_POINT('Ctrl Pts',(-4.99906860150534,1.60567510234486,4.6607514048391));
#30248=CARTESIAN_POINT('Ctrl Pts',(-5.0048068207852,1.59229321276247,4.65917598249655));
#30249=CARTESIAN_POINT('Ctrl Pts',(-5.00903265075192,1.58382769039865,4.65750148702093));
#30250=CARTESIAN_POINT('Ctrl Pts',(-5.02526070150406,1.5553817231016,4.64948528566701));
#30251=CARTESIAN_POINT('Ctrl Pts',(-5.03904418853066,1.53784678859742,4.64009844156316));
#30252=CARTESIAN_POINT('Ctrl Pts',(-5.06887391873792,1.50793670435945,4.61539308723159));
#30253=CARTESIAN_POINT('Ctrl Pts',(-5.08464752863709,1.49596352744058,4.60019195379199));
#30254=CARTESIAN_POINT('Ctrl Pts',(-5.12051265170942,1.47396686151477,4.56080656181526));
#30255=CARTESIAN_POINT('Ctrl Pts',(-5.14033036468259,1.46577346708359,4.53533737515849));
#30256=CARTESIAN_POINT('Ctrl Pts',(-5.18448569842593,1.45242234129825,4.46952174021338));
#30257=CARTESIAN_POINT('Ctrl Pts',(-5.20918596695372,1.449593873856,4.42457618200296));
#30258=CARTESIAN_POINT('Ctrl Pts',(-5.2733050916799,1.44959267390549,4.27073174534986));
#30259=CARTESIAN_POINT('Ctrl Pts',(-5.30264140340673,1.46013497556793,4.14407324412991));
#30260=CARTESIAN_POINT('Ctrl Pts',(-5.30264140340673,1.46013497556793,4.));
#30261=CARTESIAN_POINT('',(-5.14817281542751,1.93554040580225,0.));
#30262=CARTESIAN_POINT('',(-5.14817281542751,1.93554040580225,0.));
#30263=CARTESIAN_POINT('',(-5.30264140340673,1.46013497556791,0.));
#30264=CARTESIAN_POINT('Origin',(-5.23081083962335,1.69959346906221,0.));
#30265=CARTESIAN_POINT('',(-5.30264140340673,1.46013497556791,0.));
#30266=CARTESIAN_POINT('Origin',(-4.90053588303602,2.49694774856751,0.));
#30267=CARTESIAN_POINT('',(-4.78200503722117,2.71706235187773,4.));
#30268=CARTESIAN_POINT('',(-5.00894165471237,2.2716741623057,4.));
#30269=CARTESIAN_POINT('Ctrl Pts',(-4.78200503722117,2.71706235187773,4.));
#30270=CARTESIAN_POINT('Ctrl Pts',(-4.78200503722117,2.71706235187773,4.02673063961767));
#30271=CARTESIAN_POINT('Ctrl Pts',(-4.78105763595755,2.71656170391563,4.05414638575999));
#30272=CARTESIAN_POINT('Ctrl Pts',(-4.77125869941107,2.71111272728886,4.19012241323822));
#30273=CARTESIAN_POINT('Ctrl Pts',(-4.7489216143673,2.69866473158211,4.2868635932901));
#30274=CARTESIAN_POINT('Ctrl Pts',(-4.7079974505867,2.65810766401414,4.42646405387435));
#30275=CARTESIAN_POINT('Ctrl Pts',(-4.69116099815551,2.63678804974402,4.47482705790043));
#30276=CARTESIAN_POINT('Ctrl Pts',(-4.66858015738992,2.59232072134735,4.54353143773199));
#30277=CARTESIAN_POINT('Ctrl Pts',(-4.6604253230545,2.57108789627306,4.56934838942204));
#30278=CARTESIAN_POINT('Ctrl Pts',(-4.65194465335057,2.52878911058685,4.60714056402288));
#30279=CARTESIAN_POINT('Ctrl Pts',(-4.65001505726266,2.5097148286128,4.62089194101726));
#30280=CARTESIAN_POINT('Ctrl Pts',(-4.65133371044068,2.46750571613681,4.64388394673187));
#30281=CARTESIAN_POINT('Ctrl Pts',(-4.65486566583134,2.44470827369088,4.65258978726598));
#30282=CARTESIAN_POINT('Ctrl Pts',(-4.66442026184277,2.41444247464924,4.65886310574997));
#30283=CARTESIAN_POINT('Ctrl Pts',(-4.66705714187621,2.40724075158792,4.65995935047192));
#30284=CARTESIAN_POINT('Ctrl Pts',(-4.67183022340342,2.39587909673004,4.661036848069));
#30285=CARTESIAN_POINT('Ctrl Pts',(-4.67373307616942,2.39167738493323,4.66128876278955));
#30286=CARTESIAN_POINT('Ctrl Pts',(-4.67753747468403,2.38386250371066,4.6614766362689));
#30287=CARTESIAN_POINT('Ctrl Pts',(-4.67940914251737,2.38024487913886,4.66144660123004));
#30288=CARTESIAN_POINT('Ctrl Pts',(-4.68378950059938,2.37226286965328,4.66111486035927));
#30289=CARTESIAN_POINT('Ctrl Pts',(-4.68633884587834,2.3679331997458,4.66075140483911));
#30290=CARTESIAN_POINT('Ctrl Pts',(-4.69409980689487,2.3556137186935,4.65917598249656));
#30291=CARTESIAN_POINT('Ctrl Pts',(-4.6995979093446,2.34791348640791,4.65750148702094));
#30292=CARTESIAN_POINT('Ctrl Pts',(-4.72007609553974,2.32235636260972,4.64948528566702));
#30293=CARTESIAN_POINT('Ctrl Pts',(-4.73643295306733,2.30719352466623,4.64009844156317));
#30294=CARTESIAN_POINT('Ctrl Pts',(-4.77057439782323,2.28231808108543,4.61539308723159));
#30295=CARTESIAN_POINT('Ctrl Pts',(-4.78802682593589,2.2729598500691,4.60019195379197));
#30296=CARTESIAN_POINT('Ctrl Pts',(-4.82689142649517,2.25684454094365,4.56080656181529));
#30297=CARTESIAN_POINT('Ctrl Pts',(-4.84774687981072,2.25185219412136,4.53533737515855));
#30298=CARTESIAN_POINT('Ctrl Pts',(-4.89344716434411,2.24557285886215,4.46952174021331));
#30299=CARTESIAN_POINT('Ctrl Pts',(-4.91828580136978,2.2466431878412,4.42457618200287));
#30300=CARTESIAN_POINT('Ctrl Pts',(-4.98161570098456,2.25667244363945,4.27073174534989));
#30301=CARTESIAN_POINT('Ctrl Pts',(-5.00894165471236,2.27167416230572,4.14407324412994));
#30302=CARTESIAN_POINT('Ctrl Pts',(-5.00894165471236,2.27167416230572,4.));
#30303=CARTESIAN_POINT('',(-4.78200503722117,2.71706235187773,0.));
#30304=CARTESIAN_POINT('',(-4.78200503722117,2.71706235187773,0.));
#30305=CARTESIAN_POINT('',(-5.00894165471237,2.2716741623057,0.));
#30306=CARTESIAN_POINT('Origin',(-4.90053588303602,2.49694774856751,0.));
#30307=CARTESIAN_POINT('',(-5.00894165471237,2.2716741623057,0.));
#30308=CARTESIAN_POINT('Origin',(-4.44959346906221,3.2328188876086,0.));
#30309=CARTESIAN_POINT('',(-4.29808842443363,3.43168120543702,4.));
#30310=CARTESIAN_POINT('',(-4.59190513875472,3.02727719191323,4.));
#30311=CARTESIAN_POINT('Ctrl Pts',(-4.29808842443363,3.43168120543702,4.));
#30312=CARTESIAN_POINT('Ctrl Pts',(-4.29808842443363,3.43168120543702,4.02673063961775));
#30313=CARTESIAN_POINT('Ctrl Pts',(-4.29723100584781,3.43103851507225,4.05414638576015));
#30314=CARTESIAN_POINT('Ctrl Pts',(-4.28840511821421,3.42412373299318,4.19012241323848));
#30315=CARTESIAN_POINT('Ctrl Pts',(-4.26829033530279,3.40833470282044,4.2868635932903));
#30316=CARTESIAN_POINT('Ctrl Pts',(-4.23421453905669,3.36187501038656,4.42646405387453));
#30317=CARTESIAN_POINT('Ctrl Pts',(-4.22092049374663,3.33818407451672,4.47482705790057));
#30318=CARTESIAN_POINT('Ctrl Pts',(-4.20557388333115,3.29073179097664,4.54353143773204));
#30319=CARTESIAN_POINT('Ctrl Pts',(-4.20084099417036,3.26848468006611,4.56934838942209));
#30320=CARTESIAN_POINT('Ctrl Pts',(-4.19908172349404,3.22537999359419,4.60714056402292));
#30321=CARTESIAN_POINT('Ctrl Pts',(-4.20015975903259,3.20623869235145,4.62089194101729));
#30322=CARTESIAN_POINT('Ctrl Pts',(-4.20806513733182,3.16475552689651,4.6438839467319));
#30323=CARTESIAN_POINT('Ctrl Pts',(-4.215119914204,3.14279127834937,4.652589787266));
#30324=CARTESIAN_POINT('Ctrl Pts',(-4.22929149136569,3.11439276963285,4.65886310574998));
#30325=CARTESIAN_POINT('Ctrl Pts',(-4.23302250472473,3.10769221065042,4.65995935047192));
#30326=CARTESIAN_POINT('Ctrl Pts',(-4.2395141760975,3.09721711107278,4.661036848069));
#30327=CARTESIAN_POINT('Ctrl Pts',(-4.24205089412554,3.09336480107502,4.66128876278955));
#30328=CARTESIAN_POINT('Ctrl Pts',(-4.24703097094481,3.08624127305477,4.6614766362689));
#30329=CARTESIAN_POINT('Ctrl Pts',(-4.24944551660587,3.08296098080079,4.66144660123004));
#30330=CARTESIAN_POINT('Ctrl Pts',(-4.25502060659492,3.07576248207062,4.66111486035927));
#30331=CARTESIAN_POINT('Ctrl Pts',(-4.25821587479887,3.07188492304929,4.66075140483911));
#30332=CARTESIAN_POINT('Ctrl Pts',(-4.26780847693471,3.06093119703656,4.65917598249656));
#30333=CARTESIAN_POINT('Ctrl Pts',(-4.274443470338,3.05418586010366,4.65750148702094));
#30334=CARTESIAN_POINT('Ctrl Pts',(-4.29866755106879,3.03214688101149,4.64948528566702));
#30335=CARTESIAN_POINT('Ctrl Pts',(-4.31719501897974,3.01972949902145,4.64009844156318));
#30336=CARTESIAN_POINT('Ctrl Pts',(-4.35480750260545,3.00050121207563,4.61539308723159));
#30337=CARTESIAN_POINT('Ctrl Pts',(-4.37350901223016,2.99398835766767,4.60019195379195));
#30338=CARTESIAN_POINT('Ctrl Pts',(-4.41441611482645,2.98415121773687,4.56080656181527));
#30339=CARTESIAN_POINT('Ctrl Pts',(-4.4357957780085,2.98248284667088,4.53533737515851));
#30340=CARTESIAN_POINT('Ctrl Pts',(-4.48191572065581,2.98342992001184,4.46952174021366));
#30341=CARTESIAN_POINT('Ctrl Pts',(-4.50628111650113,2.98837269036042,4.42457618200336));
#30342=CARTESIAN_POINT('Ctrl Pts',(-4.56726239869638,3.00818544834456,4.27073174534982));
#30343=CARTESIAN_POINT('Ctrl Pts',(-4.59190513875471,3.02727719191324,4.14407324412986));
#30344=CARTESIAN_POINT('Ctrl Pts',(-4.59190513875471,3.02727719191324,4.));
#30345=CARTESIAN_POINT('',(-4.29808842443363,3.43168120543702,0.));
#30346=CARTESIAN_POINT('',(-4.29808842443363,3.43168120543702,0.));
#30347=CARTESIAN_POINT('',(-4.59190513875472,3.02727719191323,0.));
#30348=CARTESIAN_POINT('Origin',(-4.44959346906221,3.2328188876086,0.));
#30349=CARTESIAN_POINT('',(-4.59190513875472,3.02727719191323,0.));
#30350=CARTESIAN_POINT('Origin',(-3.88908729652601,3.88908729652601,0.));
#30351=CARTESIAN_POINT('',(-3.70833861009886,4.0618006786215,4.));
#30352=CARTESIAN_POINT('',(-4.0618006786215,3.70833861009886,4.));
#30353=CARTESIAN_POINT('Ctrl Pts',(-3.70833861009886,4.06180067862149,4.));
#30354=CARTESIAN_POINT('Ctrl Pts',(-3.70833861009886,4.06180067862149,4.02673063961768));
#30355=CARTESIAN_POINT('Ctrl Pts',(-3.70759228668204,4.06103177102382,4.05414638576001));
#30356=CARTESIAN_POINT('Ctrl Pts',(-3.69995677060637,4.05282144837612,4.19012241323826));
#30357=CARTESIAN_POINT('Ctrl Pts',(-3.68255958253974,4.03408016206108,4.28686359329013));
#30358=CARTESIAN_POINT('Ctrl Pts',(-3.65617121302277,3.9828618365799,4.42646405387448));
#30359=CARTESIAN_POINT('Ctrl Pts',(-3.64674691834979,3.95738292857717,4.47482705790052));
#30360=CARTESIAN_POINT('Ctrl Pts',(-3.63901242276529,3.90811412259949,4.543531437732));
#30361=CARTESIAN_POINT('Ctrl Pts',(-3.63781801821782,3.88540052355728,4.56934838942205));
#30362=CARTESIAN_POINT('Ctrl Pts',(-3.64282346565182,3.84255131673685,4.60714056402287));
#30363=CARTESIAN_POINT('Ctrl Pts',(-3.64688258800407,3.82381431858834,4.62089194101726));
#30364=CARTESIAN_POINT('Ctrl Pts',(-3.66118003477433,3.78407855336268,4.64388394673188));
#30365=CARTESIAN_POINT('Ctrl Pts',(-3.67158392110796,3.76348833140871,4.65258978726598));
#30366=CARTESIAN_POINT('Ctrl Pts',(-3.69002352815739,3.73765637855122,4.65886310574997));
#30367=CARTESIAN_POINT('Ctrl Pts',(-3.69475680491062,3.73162197364765,4.65995935047192));
#30368=CARTESIAN_POINT('Ctrl Pts',(-3.70280721963517,3.72229136106664,4.661036848069));
#30369=CARTESIAN_POINT('Ctrl Pts',(-3.70591534050851,3.71888330952516,4.66128876278955));
#30370=CARTESIAN_POINT('Ctrl Pts',(-3.71194846961323,3.71262653960874,4.6614766362689));
#30371=CARTESIAN_POINT('Ctrl Pts',(-3.71484643897442,3.70976435135453,4.66144660123004));
#30372=CARTESIAN_POINT('Ctrl Pts',(-3.72147898365232,3.70352661430895,4.66111486035927));
#30373=CARTESIAN_POINT('Ctrl Pts',(-3.7252414966736,3.70019664454576,4.66075140483911));
#30374=CARTESIAN_POINT('Ctrl Pts',(-3.73642953822813,3.69087839066038,4.65917598249656));
#30375=CARTESIAN_POINT('Ctrl Pts',(-3.74403804702709,3.68525404166196,4.65750148702094));
#30376=CARTESIAN_POINT('Ctrl Pts',(-3.77141154503086,3.66727588008421,4.64948528566702));
#30377=CARTESIAN_POINT('Ctrl Pts',(-3.79165341557607,3.65790971120312,4.64009844156318));
#30378=CARTESIAN_POINT('Ctrl Pts',(-3.831810793896,3.64480204513195,4.61539308723159));
#30379=CARTESIAN_POINT('Ctrl Pts',(-3.85130089179906,3.6412949354228,4.60019195379196));
#30380=CARTESIAN_POINT('Ctrl Pts',(-3.89324322780352,3.63797818771934,4.56080656181529));
#30381=CARTESIAN_POINT('Ctrl Pts',(-3.91462066258947,3.63967487324229,4.53533737515857));
#30382=CARTESIAN_POINT('Ctrl Pts',(-3.96002463729984,3.64782503509458,4.46952174021349));
#30383=CARTESIAN_POINT('Ctrl Pts',(-3.98331683505493,3.65651853940271,4.42457618200313));
#30384=CARTESIAN_POINT('Ctrl Pts',(-4.0404479382774,3.68562694371631,4.27073174534985));
#30385=CARTESIAN_POINT('Ctrl Pts',(-4.06180067862148,3.70833861009888,4.1440732441299));
#30386=CARTESIAN_POINT('Ctrl Pts',(-4.06180067862148,3.70833861009888,4.));
#30387=CARTESIAN_POINT('',(-3.70833861009886,4.0618006786215,0.));
#30388=CARTESIAN_POINT('',(-3.70833861009886,4.0618006786215,0.));
#30389=CARTESIAN_POINT('',(-4.0618006786215,3.70833861009886,0.));
#30390=CARTESIAN_POINT('Origin',(-3.88908729652601,3.88908729652601,0.));
#30391=CARTESIAN_POINT('',(-4.06180067862149,3.70833861009886,0.));
#30392=CARTESIAN_POINT('Origin',(-3.2328188876086,4.44959346906221,0.));
#30393=CARTESIAN_POINT('',(-3.02727719191323,4.59190513875472,4.));
#30394=CARTESIAN_POINT('',(-3.43168120543702,4.29808842443363,4.));
#30395=CARTESIAN_POINT('Ctrl Pts',(-3.02727719191322,4.59190513875472,4.));
#30396=CARTESIAN_POINT('Ctrl Pts',(-3.02727719191322,4.59190513875472,4.02673063961773));
#30397=CARTESIAN_POINT('Ctrl Pts',(-3.02666034062482,4.59102894698104,4.05414638576012));
#30398=CARTESIAN_POINT('Ctrl Pts',(-3.02040320785364,4.58172524915676,4.19012241323842));
#30399=CARTESIAN_POINT('Ctrl Pts',(-3.00615199113995,4.5604931793672,4.28686359329027));
#30400=CARTESIAN_POINT('Ctrl Pts',(-2.98810081758769,4.50577738599611,4.4264640538742));
#30401=CARTESIAN_POINT('Ctrl Pts',(-2.98277833096402,4.47913788113521,4.47482705790034));
#30402=CARTESIAN_POINT('Ctrl Pts',(-2.98284639916111,4.42926571423672,4.54353143773204));
#30403=CARTESIAN_POINT('Ctrl Pts',(-2.98521988943094,4.40664491125336,4.56934838942208));
#30404=CARTESIAN_POINT('Ctrl Pts',(-2.99686680424732,4.36510627376469,4.60714056402291));
#30405=CARTESIAN_POINT('Ctrl Pts',(-3.00380706434952,4.34723494578936,4.62089194101728));
#30406=CARTESIAN_POINT('Ctrl Pts',(-3.02414452900081,4.31022500720833,4.64388394673188));
#30407=CARTESIAN_POINT('Ctrl Pts',(-3.03764134658585,4.29151581144707,4.65258978726599));
#30408=CARTESIAN_POINT('Ctrl Pts',(-3.05989493919994,4.26888648285924,4.65886310574997));
#30409=CARTESIAN_POINT('Ctrl Pts',(-3.06551393036483,4.26366681911034,4.65995935047192));
#30410=CARTESIAN_POINT('Ctrl Pts',(-3.07492486051283,4.25571044417425,4.661036848069));
#30411=CARTESIAN_POINT('Ctrl Pts',(-3.07852785198031,4.25283056862869,4.66128876278955));
#30412=CARTESIAN_POINT('Ctrl Pts',(-3.08546547770911,4.24759461925646,4.6614766362689));
#30413=CARTESIAN_POINT('Ctrl Pts',(-3.08877551314696,4.24522101157591,4.66144660123004));
#30414=CARTESIAN_POINT('Ctrl Pts',(-3.09630219725155,4.24009763000285,4.66111486035927));
#30415=CARTESIAN_POINT('Ctrl Pts',(-3.10053930953249,4.23739724440492,4.66075140483911));
#30416=CARTESIAN_POINT('Ctrl Pts',(-3.11304730379171,4.22994390898303,4.65917598249656));
#30417=CARTESIAN_POINT('Ctrl Pts',(-3.12144198124854,4.22557903805757,4.65750148702093));
#30418=CARTESIAN_POINT('Ctrl Pts',(-3.15129087015696,4.2121043759984,4.64948528566702));
#30419=CARTESIAN_POINT('Ctrl Pts',(-3.17274872130468,4.20602004638866,4.64009844156319));
#30420=CARTESIAN_POINT('Ctrl Pts',(-3.21446218638992,4.19935575543265,4.61539308723159));
#30421=CARTESIAN_POINT('Ctrl Pts',(-3.23426096167701,4.19894074710277,4.60019195379197));
#30422=CARTESIAN_POINT('Ctrl Pts',(-3.27620577157862,4.20222606096277,4.56080656181529));
#30423=CARTESIAN_POINT('Ctrl Pts',(-3.29705459457641,4.20724602504611,4.53533737515856));
#30424=CARTESIAN_POINT('Ctrl Pts',(-3.34062460480529,4.22239859137615,4.46952174021329));
#30425=CARTESIAN_POINT('Ctrl Pts',(-3.36227007325902,4.23462876671565,4.42457618200284));
#30426=CARTESIAN_POINT('Ctrl Pts',(-3.41414424014011,4.27231607183921,4.27073174534989));
#30427=CARTESIAN_POINT('Ctrl Pts',(-3.431681205437,4.29808842443364,4.14407324412994));
#30428=CARTESIAN_POINT('Ctrl Pts',(-3.431681205437,4.29808842443364,4.));
#30429=CARTESIAN_POINT('',(-3.02727719191323,4.59190513875472,0.));
#30430=CARTESIAN_POINT('',(-3.02727719191322,4.59190513875472,0.));
#30431=CARTESIAN_POINT('',(-3.43168120543702,4.29808842443363,0.));
#30432=CARTESIAN_POINT('Origin',(-3.2328188876086,4.44959346906221,0.));
#30433=CARTESIAN_POINT('',(-3.43168120543702,4.29808842443363,0.));
#30434=CARTESIAN_POINT('Origin',(-2.49694774856751,4.90053588303602,0.));
#30435=CARTESIAN_POINT('',(-2.2716741623057,5.00894165471237,4.));
#30436=CARTESIAN_POINT('',(-2.71706235187773,4.78200503722117,4.));
#30437=CARTESIAN_POINT('Ctrl Pts',(-2.2716741623057,5.00894165471237,4.));
#30438=CARTESIAN_POINT('Ctrl Pts',(-2.2716741623057,5.00894165471237,4.02673063961772));
#30439=CARTESIAN_POINT('Ctrl Pts',(-2.27120197207165,5.00797975351207,4.05414638576009));
#30440=CARTESIAN_POINT('Ctrl Pts',(-2.26647729398003,4.99781176842887,4.19012241323845));
#30441=CARTESIAN_POINT('Ctrl Pts',(-2.25572296087186,4.97461171918823,4.28686359329029));
#30442=CARTESIAN_POINT('Ctrl Pts',(-2.24645346308548,4.91774574235115,4.42646405387434));
#30443=CARTESIAN_POINT('Ctrl Pts',(-2.24536384179618,4.89060159365313,4.47482705790043));
#30444=CARTESIAN_POINT('Ctrl Pts',(-2.25323279770997,4.84135408409937,4.54353143773202));
#30445=CARTESIAN_POINT('Ctrl Pts',(-2.25911573958947,4.81938307641843,4.56934838942208));
#30446=CARTESIAN_POINT('Ctrl Pts',(-2.27711733609156,4.78017782737532,4.60714056402291));
#30447=CARTESIAN_POINT('Ctrl Pts',(-2.28676784170657,4.76361222097947,4.62089194101728));
#30448=CARTESIAN_POINT('Ctrl Pts',(-2.31264454836303,4.73023941655983,4.6438839467319));
#30449=CARTESIAN_POINT('Ctrl Pts',(-2.32890196075715,4.71387192948318,4.65258978726599));
#30450=CARTESIAN_POINT('Ctrl Pts',(-2.35442158163031,4.69500243433729,4.65886310574998));
#30451=CARTESIAN_POINT('Ctrl Pts',(-2.36078792899602,4.69072603718763,4.65995935047192));
#30452=CARTESIAN_POINT('Ctrl Pts',(-2.37132764623411,4.68433981225311,4.661036848069));
#30453=CARTESIAN_POINT('Ctrl Pts',(-2.37533679068817,4.68205902479715,4.66128876278955));
#30454=CARTESIAN_POINT('Ctrl Pts',(-2.38300808567094,4.67797282241978,4.6614766362689));
#30455=CARTESIAN_POINT('Ctrl Pts',(-2.38664868312757,4.67614624141154,4.66144660123004));
#30456=CARTESIAN_POINT('Ctrl Pts',(-2.39488417471663,4.67226336996882,4.66111486035927));
#30457=CARTESIAN_POINT('Ctrl Pts',(-2.39949155449074,4.67025906099161,4.66075140483911));
#30458=CARTESIAN_POINT('Ctrl Pts',(-2.41301151312427,4.66485416988754,4.65917598249656));
#30459=CARTESIAN_POINT('Ctrl Pts',(-2.42198565441963,4.66185625464341,4.65750148702093));
#30460=CARTESIAN_POINT('Ctrl Pts',(-2.45357495552502,4.65321688300254,4.64948528566701));
#30461=CARTESIAN_POINT('Ctrl Pts',(-2.47572042376548,4.65056420905187,4.64009844156318));
#30462=CARTESIAN_POINT('Ctrl Pts',(-2.51796285166657,4.65050739017187,4.61539308723158));
#30463=CARTESIAN_POINT('Ctrl Pts',(-2.53758279278176,4.65319470210369,4.60019195379196));
#30464=CARTESIAN_POINT('Ctrl Pts',(-2.5784972561539,4.66300118219658,4.56080656181527));
#30465=CARTESIAN_POINT('Ctrl Pts',(-2.59830410014805,4.6712208166643,4.53533737515851));
#30466=CARTESIAN_POINT('Ctrl Pts',(-2.63896730764275,4.69300268100044,4.46952174021349));
#30467=CARTESIAN_POINT('Ctrl Pts',(-2.65843306352468,4.70846837986478,4.42457618200312));
#30468=CARTESIAN_POINT('Ctrl Pts',(-2.70377297991551,4.75380659926932,4.27073174534983));
#30469=CARTESIAN_POINT('Ctrl Pts',(-2.71706235187771,4.78200503722118,4.14407324412986));
#30470=CARTESIAN_POINT('Ctrl Pts',(-2.71706235187771,4.78200503722118,4.));
#30471=CARTESIAN_POINT('',(-2.2716741623057,5.00894165471237,0.));
#30472=CARTESIAN_POINT('',(-2.2716741623057,5.00894165471237,0.));
#30473=CARTESIAN_POINT('',(-2.71706235187773,4.78200503722117,0.));
#30474=CARTESIAN_POINT('Origin',(-2.49694774856751,4.90053588303602,0.));
#30475=CARTESIAN_POINT('',(-2.71706235187773,4.78200503722117,0.));
#30476=CARTESIAN_POINT('Origin',(-1.69959346906221,5.23081083962335,0.));
#30477=CARTESIAN_POINT('',(-1.46013497556791,5.30264140340673,4.));
#30478=CARTESIAN_POINT('',(-1.93554040580225,5.14817281542751,4.));
#30479=CARTESIAN_POINT('Ctrl Pts',(-1.46013497556791,5.30264140340673,4.));
#30480=CARTESIAN_POINT('Ctrl Pts',(-1.46013497556791,5.30264140340673,4.02673063961775));
#30481=CARTESIAN_POINT('Ctrl Pts',(-1.45981907327888,5.30161747797973,4.05414638576016));
#30482=CARTESIAN_POINT('Ctrl Pts',(-1.45674318712176,5.29083557517594,4.19012241323845));
#30483=CARTESIAN_POINT('Ctrl Pts',(-1.44975054499179,5.26623880869311,4.28686359329028));
#30484=CARTESIAN_POINT('Ctrl Pts',(-1.44949096877052,5.20862287746718,4.42646405387428));
#30485=CARTESIAN_POINT('Ctrl Pts',(-1.45266104290795,5.18164246395929,4.4748270579004));
#30486=CARTESIAN_POINT('Ctrl Pts',(-1.46813712672828,5.13423224887844,4.54353143773205));
#30487=CARTESIAN_POINT('Ctrl Pts',(-1.47738466266403,5.11345203562664,4.56934838942209));
#30488=CARTESIAN_POINT('Ctrl Pts',(-1.50129768180207,5.07754553837531,4.60714056402292));
#30489=CARTESIAN_POINT('Ctrl Pts',(-1.51342080545347,5.0626935537665,4.62089194101728));
#30490=CARTESIAN_POINT('Ctrl Pts',(-1.54419958371733,5.03377963271106,4.6438839467319));
#30491=CARTESIAN_POINT('Ctrl Pts',(-1.56281727947214,5.02015687617144,4.65258978726599));
#30492=CARTESIAN_POINT('Ctrl Pts',(-1.59097455084368,5.00551184406225,4.65886310574997));
#30493=CARTESIAN_POINT('Ctrl Pts',(-1.59793149380938,5.00228401260219,4.65995935047191));
#30494=CARTESIAN_POINT('Ctrl Pts',(-1.60934047531988,4.99762518772176,4.66103684806899));
#30495=CARTESIAN_POINT('Ctrl Pts',(-1.61365705431846,4.99599964891207,4.66128876278954));
#30496=CARTESIAN_POINT('Ctrl Pts',(-1.62187312581316,4.99316380939343,4.6614766362689));
#30497=CARTESIAN_POINT('Ctrl Pts',(-1.62575464169676,4.99192923154399,4.66144660123003));
#30498=CARTESIAN_POINT('Ctrl Pts',(-1.63449615563526,4.98938247941308,4.66111486035926));
#30499=CARTESIAN_POINT('Ctrl Pts',(-1.63936035392143,4.98812359979554,4.66075140483911));
#30500=CARTESIAN_POINT('Ctrl Pts',(-1.65355937067761,4.98490023936606,4.65917598249655));
#30501=CARTESIAN_POINT('Ctrl Pts',(-1.66289200266934,4.98334309842607,4.65750148702093));
#30502=CARTESIAN_POINT('Ctrl Pts',(-1.69544388253963,4.97975174720573,4.64948528566701));
#30503=CARTESIAN_POINT('Ctrl Pts',(-1.71773167294816,4.98059604655052,4.64009844156316));
#30504=CARTESIAN_POINT('Ctrl Pts',(-1.75946291489557,4.98714809881592,4.61539308723158));
#30505=CARTESIAN_POINT('Ctrl Pts',(-1.77842091377375,4.992871560471,4.60019195379196));
#30506=CARTESIAN_POINT('Ctrl Pts',(-1.81729758074085,5.00895773871105,4.56080656181527));
#30507=CARTESIAN_POINT('Ctrl Pts',(-1.83557473549708,5.02017464888311,4.53533737515854));
#30508=CARTESIAN_POINT('Ctrl Pts',(-1.87232987713593,5.0480494694357,4.46952174021328));
#30509=CARTESIAN_POINT('Ctrl Pts',(-1.88913660893301,5.06636987499118,4.42457618200282));
#30510=CARTESIAN_POINT('Ctrl Pts',(-1.92682585561729,5.11824263124584,4.27073174534986));
#30511=CARTESIAN_POINT('Ctrl Pts',(-1.93554040580223,5.14817281542752,4.1440732441299));
#30512=CARTESIAN_POINT('Ctrl Pts',(-1.93554040580223,5.14817281542752,4.));
#30513=CARTESIAN_POINT('',(-1.46013497556791,5.30264140340673,0.));
#30514=CARTESIAN_POINT('',(-1.46013497556791,5.30264140340673,0.));
#30515=CARTESIAN_POINT('',(-1.93554040580225,5.14817281542751,0.));
#30516=CARTESIAN_POINT('Origin',(-1.69959346906221,5.23081083962335,0.));
#30517=CARTESIAN_POINT('',(-1.93554040580225,5.14817281542751,0.));
#30518=CARTESIAN_POINT('Origin',(-0.860389557721269,5.43228587327326,0.));
#30519=CARTESIAN_POINT('',(-0.612642419821478,5.46577252229136,4.));
#30520=CARTESIAN_POINT('',(-1.1063590312456,5.38757549311203,4.));
#30521=CARTESIAN_POINT('Ctrl Pts',(-0.612642419821477,5.46577252229136,
4.));
#30522=CARTESIAN_POINT('Ctrl Pts',(-0.612642419821477,5.46577252229136,
4.02673063961771));
#30523=CARTESIAN_POINT('Ctrl Pts',(-0.612490584040256,5.46471178507989,
4.05414638576007));
#30524=CARTESIAN_POINT('Ctrl Pts',(-0.61113922834309,5.45358145078566,4.19012241323841));
#30525=CARTESIAN_POINT('Ctrl Pts',(-0.608080459247833,5.42819362108339,
4.28686359329025));
#30526=CARTESIAN_POINT('Ctrl Pts',(-0.616837196219717,5.37124643091157,
4.42646405387458));
#30527=CARTESIAN_POINT('Ctrl Pts',(-0.624188908037812,5.34509409991721,
4.47482705790059));
#30528=CARTESIAN_POINT('Ctrl Pts',(-0.646891047218759,5.30068857615024,
4.54353143773202));
#30529=CARTESIAN_POINT('Ctrl Pts',(-0.659275472185204,5.2816108351434,4.56934838942207));
#30530=CARTESIAN_POINT('Ctrl Pts',(-0.688511096065249,5.24988722681301,
4.60714056402291));
#30531=CARTESIAN_POINT('Ctrl Pts',(-0.702808326214398,5.23711456914321,
4.62089194101728));
#30532=CARTESIAN_POINT('Ctrl Pts',(-0.737731300415893,5.21337148814817,
4.64388394673189));
#30533=CARTESIAN_POINT('Ctrl Pts',(-0.758250850073323,5.20282889962289,
4.65258978726598));
#30534=CARTESIAN_POINT('Ctrl Pts',(-0.788352446473459,5.19276893984501,
4.65886310574997));
#30535=CARTESIAN_POINT('Ctrl Pts',(-0.795728682014567,5.19066915399765,
4.65995935047192));
#30536=CARTESIAN_POINT('Ctrl Pts',(-0.807726000808486,5.18785244490161,
4.661036848069));
#30537=CARTESIAN_POINT('Ctrl Pts',(-0.812243725850714,5.18692218089855,
4.66128876278954));
#30538=CARTESIAN_POINT('Ctrl Pts',(-0.820802266909525,5.1854065320192,4.6614766362689));
#30539=CARTESIAN_POINT('Ctrl Pts',(-0.824829125417006,5.18479435673255,
4.66144660123004));
#30540=CARTESIAN_POINT('Ctrl Pts',(-0.833861416620445,5.18364643340307,
4.66111486035927));
#30541=CARTESIAN_POINT('Ctrl Pts',(-0.838862660713575,5.18316398093936,
4.66075140483911));
#30542=CARTESIAN_POINT('Ctrl Pts',(-0.853391108675981,5.18220152101598,
4.65917598249655));
#30543=CARTESIAN_POINT('Ctrl Pts',(-0.862852430991235,5.18212349635794,
4.65750148702092));
#30544=CARTESIAN_POINT('Ctrl Pts',(-0.895565354310451,5.18366859654418,
4.64948528566701));
#30545=CARTESIAN_POINT('Ctrl Pts',(-0.917446667518231,5.18798907973248,
4.64009844156318));
#30546=CARTESIAN_POINT('Ctrl Pts',(-0.957639161837241,5.20098866987151,
4.61539308723157));
#30547=CARTESIAN_POINT('Ctrl Pts',(-0.975468409628044,5.20960735062882,
4.60019195379194));
#30548=CARTESIAN_POINT('Ctrl Pts',(-1.01135000762512,5.2315771319208,4.56080656181526));
#30549=CARTESIAN_POINT('Ctrl Pts',(-1.02764742893493,5.24551512024201,4.53533737515851));
#30550=CARTESIAN_POINT('Ctrl Pts',(-1.05958947114721,5.27879652641763,4.46952174021344));
#30551=CARTESIAN_POINT('Ctrl Pts',(-1.07332334134435,5.29952052947749,4.42457618200306));
#30552=CARTESIAN_POINT('Ctrl Pts',(-1.10243388398541,5.35665054316769,4.2707317453498));
#30553=CARTESIAN_POINT('Ctrl Pts',(-1.10635903124558,5.38757549311203,4.14407324412982));
#30554=CARTESIAN_POINT('Ctrl Pts',(-1.10635903124558,5.38757549311203,4.));
#30555=CARTESIAN_POINT('',(-0.612642419821478,5.46577252229136,0.));
#30556=CARTESIAN_POINT('',(-0.612642419821478,5.46577252229136,0.));
#30557=CARTESIAN_POINT('',(-1.1063590312456,5.38757549311203,0.));
#30558=CARTESIAN_POINT('Origin',(-0.860389557721269,5.43228587327326,0.));
#30559=CARTESIAN_POINT('',(-1.1063590312456,5.38757549311203,0.));
#30560=CARTESIAN_POINT('Origin',(5.55111512312578E-16,5.5,0.));
#30561=CARTESIAN_POINT('',(0.249935425544578,5.49431818181818,4.));
#30562=CARTESIAN_POINT('',(-0.249935425544576,5.49431818181818,4.));
#30563=CARTESIAN_POINT('Ctrl Pts',(0.249935425544578,5.49431818181818,4.));
#30564=CARTESIAN_POINT('Ctrl Pts',(0.249935425544578,5.49431818181818,4.02673063961771));
#30565=CARTESIAN_POINT('Ctrl Pts',(0.249919456117149,5.49324675169276,4.05414638576008));
#30566=CARTESIAN_POINT('Ctrl Pts',(0.249513006492202,5.48204205167786,4.19012241323844));
#30567=CARTESIAN_POINT('Ctrl Pts',(0.248562585506145,5.45648829138081,4.28686359329028));
#30568=CARTESIAN_POINT('Ctrl Pts',(0.231005155267317,5.40161207108225,4.42646405387434));
#30569=CARTESIAN_POINT('Ctrl Pts',(0.219652829312556,5.37693177978513,4.47482705790043));
#30570=CARTESIAN_POINT('Ctrl Pts',(0.190283636781579,5.33662435870042,4.54353143773203));
#30571=CARTESIAN_POINT('Ctrl Pts',(0.175067268428665,5.31971884723752,4.56934838942208));
#30572=CARTESIAN_POINT('Ctrl Pts',(0.141228917894012,5.29295926834978,4.60714056402291));
#30573=CARTESIAN_POINT('Ctrl Pts',(0.125109626503174,5.28258044284084,4.62089194101728));
#30574=CARTESIAN_POINT('Ctrl Pts',(0.0869023758915849,5.26459283535906,
4.64388394673189));
#30575=CARTESIAN_POINT('Ctrl Pts',(0.064986231744588,5.25739000836648,4.65258978726599));
#30576=CARTESIAN_POINT('Ctrl Pts',(0.0336815115206837,5.25216283051672,
4.65886310574997));
#30577=CARTESIAN_POINT('Ctrl Pts',(0.0260676108035225,5.25124279397842,
4.65995935047192));
#30578=CARTESIAN_POINT('Ctrl Pts',(0.0137773685317983,5.25033755739286,
4.661036848069));
#30579=CARTESIAN_POINT('Ctrl Pts',(0.00916973882989,5.25012547438354,4.66128876278955));
#30580=CARTESIAN_POINT('Ctrl Pts',(0.000479467891945075,5.24996733644903,
4.6614766362689));
#30581=CARTESIAN_POINT('Ctrl Pts',(-0.00359357861859843,5.24999263751242,
4.66144660123004));
#30582=CARTESIAN_POINT('Ctrl Pts',(-0.0126942421010641,5.25027180866649,
4.66111486035927));
#30583=CARTESIAN_POINT('Ctrl Pts',(-0.0177093847734033,5.25057766293744,
4.66075140483911));
#30584=CARTESIAN_POINT('Ctrl Pts',(-0.0322095253360055,5.25189980247768,
4.65917598249656));
#30585=CARTESIAN_POINT('Ctrl Pts',(-0.0415665688190214,5.25330281532761,
4.65750148702093));
#30586=CARTESIAN_POINT('Ctrl Pts',(-0.0736350348471669,5.25994632142597,
4.64948528566701));
#30587=CARTESIAN_POINT('Ctrl Pts',(-0.0945710803031294,5.26763660382283,
4.64009844156317));
#30588=CARTESIAN_POINT('Ctrl Pts',(-0.13223515439229,5.28676363878308,4.61539308723158));
#30589=CARTESIAN_POINT('Ctrl Pts',(-0.148496635843228,5.29806531811862,
4.60019195379194));
#30590=CARTESIAN_POINT('Ctrl Pts',(-0.180499640843389,5.32537773353358,
4.56080656181527));
#30591=CARTESIAN_POINT('Ctrl Pts',(-0.194416032106083,5.34169360047391,
4.53533737515855));
#30592=CARTESIAN_POINT('Ctrl Pts',(-0.220758455803101,5.37956209359798,
4.46952174021344));
#30593=CARTESIAN_POINT('Ctrl Pts',(-0.231081290935902,5.40217940042789,
4.42457618200305));
#30594=CARTESIAN_POINT('Ctrl Pts',(-0.250896331361511,5.46315994101283,
4.27073174534979));
#30595=CARTESIAN_POINT('Ctrl Pts',(-0.249935425544556,5.49431818181818,
4.14407324412982));
#30596=CARTESIAN_POINT('Ctrl Pts',(-0.249935425544556,5.49431818181818,
4.));
#30597=CARTESIAN_POINT('',(0.249935425544578,5.49431818181818,0.));
#30598=CARTESIAN_POINT('',(0.249935425544578,5.49431818181818,0.));
#30599=CARTESIAN_POINT('',(-0.249935425544576,5.49431818181818,0.));
#30600=CARTESIAN_POINT('Origin',(5.55111512312578E-16,5.5,0.));
#30601=CARTESIAN_POINT('',(-0.249935425544576,5.49431818181818,0.));
#30602=CARTESIAN_POINT('Origin',(0.860389557721271,5.43228587327326,0.));
#30603=CARTESIAN_POINT('',(1.1063590312456,5.38757549311203,4.));
#30604=CARTESIAN_POINT('',(0.612642419821479,5.46577252229136,4.));
#30605=CARTESIAN_POINT('Ctrl Pts',(1.1063590312456,5.38757549311203,4.));
#30606=CARTESIAN_POINT('Ctrl Pts',(1.1063590312456,5.38757549311203,4.02673063961778));
#30607=CARTESIAN_POINT('Ctrl Pts',(1.10617564982983,5.38651975223822,4.05414638576023));
#30608=CARTESIAN_POINT('Ctrl Pts',(1.10402140302145,5.37551658340324,4.19012241323862));
#30609=CARTESIAN_POINT('Ctrl Pts',(1.09908519447303,5.350426110898,4.28686359329042));
#30610=CARTESIAN_POINT('Ctrl Pts',(1.0731593931695,5.29897209514011,4.42646405387433));
#30611=CARTESIAN_POINT('Ctrl Pts',(1.05808598501926,5.27637155422115,4.47482705790043));
#30612=CARTESIAN_POINT('Ctrl Pts',(1.02277290612914,5.24115473829854,4.54353143773207));
#30613=CARTESIAN_POINT('Ctrl Pts',(1.00509927187884,5.22683772617799,4.56934838942211));
#30614=CARTESIAN_POINT('Ctrl Pts',(0.96749140718278,5.20570108637508,4.60714056402294));
#30615=CARTESIAN_POINT('Ctrl Pts',(0.949946965001159,5.19797165415638,4.6208919410173));
#30616=CARTESIAN_POINT('Ctrl Pts',(0.909396227292128,5.18618243478151,4.6438839467319));
#30617=CARTESIAN_POINT('Ctrl Pts',(0.886623136859981,5.182496726827,4.65258978726599));
#30618=CARTESIAN_POINT('Ctrl Pts',(0.854886118918656,5.18223104137204,4.65886310574997));
#30619=CARTESIAN_POINT('Ctrl Pts',(0.847222032530184,5.1825134084958,4.65995935047192));
#30620=CARTESIAN_POINT('Ctrl Pts',(0.834941493334322,5.18354193434975,4.66103684806899));
#30621=CARTESIAN_POINT('Ctrl Pts',(0.830357414107859,5.18405325452173,4.66128876278954));
#30622=CARTESIAN_POINT('Ctrl Pts',(0.821749396602616,5.18525652141284,4.6614766362689));
#30623=CARTESIAN_POINT('Ctrl Pts',(0.817730454011735,5.18591867583013,4.66144660123003));
#30624=CARTESIAN_POINT('Ctrl Pts',(0.808785506788659,5.18761806734741,4.66111486035927));
#30625=CARTESIAN_POINT('Ctrl Pts',(0.803879954994051,5.18870469720579,4.66075140483911));
#30626=CARTESIAN_POINT('Ctrl Pts',(0.78976516341501,5.19227888074625,4.65917598249655));
#30627=CARTESIAN_POINT('Ctrl Pts',(0.780742800229017,5.19512838427146,4.65750148702093));
#30628=CARTESIAN_POINT('Ctrl Pts',(0.750108423554737,5.20670671111326,4.64948528566701));
#30629=CARTESIAN_POINT('Ctrl Pts',(0.730633160772473,5.21757743244348,4.64009844156316));
#30630=CARTESIAN_POINT('Ctrl Pts',(0.696424921417117,5.24236094114525,4.61539308723157));
#30631=CARTESIAN_POINT('Ctrl Pts',(0.682131617948134,5.25606733420563,4.60019195379195));
#30632=CARTESIAN_POINT('Ctrl Pts',(0.654795226139856,5.28804986143137,4.56080656181527));
#30633=CARTESIAN_POINT('Ctrl Pts',(0.64360253266301,5.30634185619751,4.53533737515854));
#30634=CARTESIAN_POINT('Ctrl Pts',(0.623508365378152,5.34786498829105,4.4695217402133));
#30635=CARTESIAN_POINT('Ctrl Pts',(0.61685074777022,5.3718186857343,4.42457618200285));
#30636=CARTESIAN_POINT('Ctrl Pts',(0.606819121617707,5.43514820992188,4.27073174534981));
#30637=CARTESIAN_POINT('Ctrl Pts',(0.6126424198215,5.46577252229136,4.14407324412984));
#30638=CARTESIAN_POINT('Ctrl Pts',(0.6126424198215,5.46577252229136,4.));
#30639=CARTESIAN_POINT('',(1.1063590312456,5.38757549311203,0.));
#30640=CARTESIAN_POINT('',(1.1063590312456,5.38757549311203,0.));
#30641=CARTESIAN_POINT('',(0.612642419821479,5.46577252229136,0.));
#30642=CARTESIAN_POINT('Origin',(0.860389557721271,5.43228587327326,0.));
#30643=CARTESIAN_POINT('',(0.612642419821479,5.46577252229136,0.));
#30644=CARTESIAN_POINT('Origin',(1.69959346906221,5.23081083962335,0.));
#30645=CARTESIAN_POINT('',(1.93554040580225,5.14817281542751,4.));
#30646=CARTESIAN_POINT('',(1.46013497556791,5.30264140340673,4.));
#30647=CARTESIAN_POINT('Ctrl Pts',(1.93554040580225,5.14817281542752,4.));
#30648=CARTESIAN_POINT('Ctrl Pts',(1.93554040580225,5.14817281542752,4.02673063961771));
#30649=CARTESIAN_POINT('Ctrl Pts',(1.9351941278572,5.14715875964944,4.05414638576008));
#30650=CARTESIAN_POINT('Ctrl Pts',(1.93134512857137,5.1366280565286,4.19012241323841));
#30651=CARTESIAN_POINT('Ctrl Pts',(1.92254467829738,5.11261868251876,4.28686359329026));
#30652=CARTESIAN_POINT('Ctrl Pts',(1.88888888520004,5.06585383993554,4.42646405387427));
#30653=CARTESIAN_POINT('Ctrl Pts',(1.87046555218873,5.04588954971905,4.47482705790038));
#30654=CARTESIAN_POINT('Ctrl Pts',(1.8300781121392,5.01663049384451,4.54353143773201));
#30655=CARTESIAN_POINT('Ctrl Pts',(1.81038239552218,5.00525451342014,4.56934838942206));
#30656=CARTESIAN_POINT('Ctrl Pts',(1.76993104710689,4.99026126692246,4.6071405640229));
#30657=CARTESIAN_POINT('Ctrl Pts',(1.75139345652766,4.98537155226774,4.62089194101727));
#30658=CARTESIAN_POINT('Ctrl Pts',(1.70949772546377,4.98007101070696,4.64388394673188));
#30659=CARTESIAN_POINT('Ctrl Pts',(1.68642843781245,4.97999317615251,4.65258978726598));
#30660=CARTESIAN_POINT('Ctrl Pts',(1.65504059286449,4.98469552515,4.65886310574997));
#30661=CARTESIAN_POINT('Ctrl Pts',(1.64751503604724,4.98617334312012,4.65995935047191));
#30662=CARTESIAN_POINT('Ctrl Pts',(1.63554658755904,4.98911030569357,4.66103684806899));
#30663=CARTESIAN_POINT('Ctrl Pts',(1.63109893405225,4.99033243864724,4.66128876278954));
#30664=CARTESIAN_POINT('Ctrl Pts',(1.62278512793909,4.9928674819397,4.6614766362689));
#30665=CARTESIAN_POINT('Ctrl Pts',(1.61891924897259,4.99415018527156,4.66144660123003));
#30666=CARTESIAN_POINT('Ctrl Pts',(1.61035027229599,4.99722795249295,4.66111486035926));
#30667=CARTESIAN_POINT('Ctrl Pts',(1.60567510234484,4.99906860150535,4.6607514048391));
#30668=CARTESIAN_POINT('Ctrl Pts',(1.59229321276247,5.0048068207852,4.65917598249655));
#30669=CARTESIAN_POINT('Ctrl Pts',(1.58382769039865,5.00903265075193,4.65750148702093));
#30670=CARTESIAN_POINT('Ctrl Pts',(1.55538172310161,5.02526070150406,4.64948528566701));
#30671=CARTESIAN_POINT('Ctrl Pts',(1.53784678859743,5.03904418853064,4.64009844156317));
#30672=CARTESIAN_POINT('Ctrl Pts',(1.50793670435945,5.06887391873793,4.61539308723159));
#30673=CARTESIAN_POINT('Ctrl Pts',(1.49596352744057,5.0846475286371,4.60019195379198));
#30674=CARTESIAN_POINT('Ctrl Pts',(1.47396686151476,5.12051265170942,4.56080656181526));
#30675=CARTESIAN_POINT('Ctrl Pts',(1.46577346708359,5.14033036468259,4.53533737515849));
#30676=CARTESIAN_POINT('Ctrl Pts',(1.45242234129825,5.18448569842591,4.4695217402134));
#30677=CARTESIAN_POINT('Ctrl Pts',(1.449593873856,5.20918596695371,4.424576182003));
#30678=CARTESIAN_POINT('Ctrl Pts',(1.44959267390549,5.2733050916799,4.27073174534986));
#30679=CARTESIAN_POINT('Ctrl Pts',(1.46013497556793,5.30264140340673,4.14407324412991));
#30680=CARTESIAN_POINT('Ctrl Pts',(1.46013497556793,5.30264140340673,4.));
#30681=CARTESIAN_POINT('',(1.93554040580225,5.14817281542751,0.));
#30682=CARTESIAN_POINT('',(1.93554040580225,5.14817281542751,0.));
#30683=CARTESIAN_POINT('',(1.46013497556791,5.30264140340673,0.));
#30684=CARTESIAN_POINT('Origin',(1.69959346906221,5.23081083962335,0.));
#30685=CARTESIAN_POINT('',(1.46013497556791,5.30264140340673,0.));
#30686=CARTESIAN_POINT('Origin',(2.49694774856751,4.90053588303602,0.));
#30687=CARTESIAN_POINT('',(2.71706235187773,4.78200503722117,4.));
#30688=CARTESIAN_POINT('',(2.2716741623057,5.00894165471237,4.));
#30689=CARTESIAN_POINT('Ctrl Pts',(2.71706235187773,4.78200503722117,4.));
#30690=CARTESIAN_POINT('Ctrl Pts',(2.71706235187773,4.78200503722117,4.02673063961773));
#30691=CARTESIAN_POINT('Ctrl Pts',(2.71656170391563,4.78105763595755,4.05414638576012));
#30692=CARTESIAN_POINT('Ctrl Pts',(2.71111272728885,4.77125869941104,4.19012241323842));
#30693=CARTESIAN_POINT('Ctrl Pts',(2.69866473158208,4.74892161436726,4.28686359329027));
#30694=CARTESIAN_POINT('Ctrl Pts',(2.65810766401412,4.70799745058669,4.42646405387437));
#30695=CARTESIAN_POINT('Ctrl Pts',(2.63678804974402,4.6911609981555,4.47482705790045));
#30696=CARTESIAN_POINT('Ctrl Pts',(2.59232072134733,4.66858015738991,4.54353143773201));
#30697=CARTESIAN_POINT('Ctrl Pts',(2.57108789627304,4.66042532305449,4.56934838942207));
#30698=CARTESIAN_POINT('Ctrl Pts',(2.52878911058682,4.65194465335057,4.60714056402291));
#30699=CARTESIAN_POINT('Ctrl Pts',(2.50971482861278,4.65001505726266,4.62089194101728));
#30700=CARTESIAN_POINT('Ctrl Pts',(2.46750571613677,4.65133371044068,4.64388394673189));
#30701=CARTESIAN_POINT('Ctrl Pts',(2.44470827369085,4.65486566583135,4.65258978726599));
#30702=CARTESIAN_POINT('Ctrl Pts',(2.41444247464919,4.66442026184278,4.65886310574998));
#30703=CARTESIAN_POINT('Ctrl Pts',(2.40724075158789,4.66705714187622,4.65995935047192));
#30704=CARTESIAN_POINT('Ctrl Pts',(2.3958790967301,4.6718302234034,4.661036848069));
#30705=CARTESIAN_POINT('Ctrl Pts',(2.39167738493326,4.67373307616941,4.66128876278955));
#30706=CARTESIAN_POINT('Ctrl Pts',(2.38386250371063,4.67753747468405,4.6614766362689));
#30707=CARTESIAN_POINT('Ctrl Pts',(2.3802448791388,4.67940914251739,4.66144660123004));
#30708=CARTESIAN_POINT('Ctrl Pts',(2.37226286965328,4.68378950059938,4.66111486035927));
#30709=CARTESIAN_POINT('Ctrl Pts',(2.36793319974581,4.68633884587833,4.66075140483911));
#30710=CARTESIAN_POINT('Ctrl Pts',(2.35561371869349,4.69409980689487,4.65917598249656));
#30711=CARTESIAN_POINT('Ctrl Pts',(2.3479134864079,4.69959790934461,4.65750148702094));
#30712=CARTESIAN_POINT('Ctrl Pts',(2.32235636260971,4.72007609553974,4.64948528566702));
#30713=CARTESIAN_POINT('Ctrl Pts',(2.30719352466623,4.73643295306733,4.64009844156317));
#30714=CARTESIAN_POINT('Ctrl Pts',(2.28231808108543,4.77057439782323,4.61539308723159));
#30715=CARTESIAN_POINT('Ctrl Pts',(2.27295985006911,4.78802682593589,4.60019195379197));
#30716=CARTESIAN_POINT('Ctrl Pts',(2.25684454094365,4.82689142649517,4.56080656181529));
#30717=CARTESIAN_POINT('Ctrl Pts',(2.25185219412136,4.84774687981072,4.53533737515856));
#30718=CARTESIAN_POINT('Ctrl Pts',(2.24557285886215,4.89344716434413,4.46952174021327));
#30719=CARTESIAN_POINT('Ctrl Pts',(2.24664318784121,4.9182858013698,4.42457618200281));
#30720=CARTESIAN_POINT('Ctrl Pts',(2.25667244363945,4.98161570098455,4.2707317453499));
#30721=CARTESIAN_POINT('Ctrl Pts',(2.27167416230572,5.00894165471236,4.14407324412995));
#30722=CARTESIAN_POINT('Ctrl Pts',(2.27167416230572,5.00894165471236,4.));
#30723=CARTESIAN_POINT('',(2.71706235187773,4.78200503722117,0.));
#30724=CARTESIAN_POINT('',(2.71706235187773,4.78200503722117,0.));
#30725=CARTESIAN_POINT('',(2.2716741623057,5.00894165471237,0.));
#30726=CARTESIAN_POINT('Origin',(2.49694774856751,4.90053588303602,0.));
#30727=CARTESIAN_POINT('',(2.2716741623057,5.00894165471237,0.));
#30728=CARTESIAN_POINT('Origin',(3.2328188876086,4.44959346906221,0.));
#30729=CARTESIAN_POINT('',(3.43168120543702,4.29808842443363,4.));
#30730=CARTESIAN_POINT('',(3.02727719191323,4.59190513875472,4.));
#30731=CARTESIAN_POINT('Ctrl Pts',(3.43168120543702,4.29808842443363,4.));
#30732=CARTESIAN_POINT('Ctrl Pts',(3.43168120543702,4.29808842443363,4.02673063961771));
#30733=CARTESIAN_POINT('Ctrl Pts',(3.43103851507226,4.29723100584781,4.05414638576007));
#30734=CARTESIAN_POINT('Ctrl Pts',(3.4241237329932,4.28840511821422,4.19012241323845));
#30735=CARTESIAN_POINT('Ctrl Pts',(3.40833470282044,4.26829033530279,4.28686359329029));
#30736=CARTESIAN_POINT('Ctrl Pts',(3.36187501038662,4.23421453905672,4.4264640538744));
#30737=CARTESIAN_POINT('Ctrl Pts',(3.33818407451679,4.22092049374665,4.47482705790047));
#30738=CARTESIAN_POINT('Ctrl Pts',(3.29073179097663,4.20557388333114,4.54353143773206));
#30739=CARTESIAN_POINT('Ctrl Pts',(3.26848468006611,4.20084099417036,4.56934838942209));
#30740=CARTESIAN_POINT('Ctrl Pts',(3.22537999359419,4.19908172349404,4.60714056402291));
#30741=CARTESIAN_POINT('Ctrl Pts',(3.20623869235145,4.20015975903259,4.62089194101728));
#30742=CARTESIAN_POINT('Ctrl Pts',(3.16475552689653,4.20806513733182,4.64388394673189));
#30743=CARTESIAN_POINT('Ctrl Pts',(3.14279127834938,4.215119914204,4.65258978726599));
#30744=CARTESIAN_POINT('Ctrl Pts',(3.11439276963289,4.22929149136567,4.65886310574998));
#30745=CARTESIAN_POINT('Ctrl Pts',(3.10769221065044,4.23302250472471,4.65995935047192));
#30746=CARTESIAN_POINT('Ctrl Pts',(3.0972171110728,4.23951417609748,4.661036848069));
#30747=CARTESIAN_POINT('Ctrl Pts',(3.09336480107503,4.24205089412553,4.66128876278955));
#30748=CARTESIAN_POINT('Ctrl Pts',(3.08624127305476,4.24703097094481,4.6614766362689));
#30749=CARTESIAN_POINT('Ctrl Pts',(3.08296098080077,4.24944551660588,4.66144660123004));
#30750=CARTESIAN_POINT('Ctrl Pts',(3.07576248207062,4.25502060659492,4.66111486035927));
#30751=CARTESIAN_POINT('Ctrl Pts',(3.07188492304929,4.25821587479887,4.66075140483911));
#30752=CARTESIAN_POINT('Ctrl Pts',(3.06093119703656,4.26780847693471,4.65917598249656));
#30753=CARTESIAN_POINT('Ctrl Pts',(3.05418586010366,4.27444347033801,4.65750148702093));
#30754=CARTESIAN_POINT('Ctrl Pts',(3.03214688101148,4.2986675510688,4.64948528566702));
#30755=CARTESIAN_POINT('Ctrl Pts',(3.01972949902144,4.31719501897974,4.64009844156318));
#30756=CARTESIAN_POINT('Ctrl Pts',(3.00050121207562,4.35480750260546,4.61539308723158));
#30757=CARTESIAN_POINT('Ctrl Pts',(2.99398835766767,4.37350901223017,4.60019195379194));
#30758=CARTESIAN_POINT('Ctrl Pts',(2.98415121773687,4.41441611482646,4.56080656181526));
#30759=CARTESIAN_POINT('Ctrl Pts',(2.98248284667088,4.43579577800851,4.53533737515849));
#30760=CARTESIAN_POINT('Ctrl Pts',(2.98342992001184,4.48191572065583,4.46952174021363));
#30761=CARTESIAN_POINT('Ctrl Pts',(2.98837269036043,4.50628111650115,4.42457618200332));
#30762=CARTESIAN_POINT('Ctrl Pts',(3.00818544834457,4.56726239869641,4.27073174534976));
#30763=CARTESIAN_POINT('Ctrl Pts',(3.02727719191324,4.59190513875471,4.14407324412977));
#30764=CARTESIAN_POINT('Ctrl Pts',(3.02727719191324,4.59190513875471,4.));
#30765=CARTESIAN_POINT('',(3.43168120543702,4.29808842443363,0.));
#30766=CARTESIAN_POINT('',(3.43168120543702,4.29808842443363,0.));
#30767=CARTESIAN_POINT('',(3.02727719191323,4.59190513875472,0.));
#30768=CARTESIAN_POINT('Origin',(3.2328188876086,4.44959346906221,0.));
#30769=CARTESIAN_POINT('',(3.02727719191323,4.59190513875472,0.));
#30770=CARTESIAN_POINT('Origin',(3.88908729652601,3.88908729652601,0.));
#30771=CARTESIAN_POINT('',(4.06180067862149,3.70833861009886,4.));
#30772=CARTESIAN_POINT('',(3.70833861009886,4.0618006786215,4.));
#30773=CARTESIAN_POINT('Ctrl Pts',(4.06180067862149,3.70833861009886,4.));
#30774=CARTESIAN_POINT('Ctrl Pts',(4.06180067862149,3.70833861009886,4.02673063961773));
#30775=CARTESIAN_POINT('Ctrl Pts',(4.06103177102382,3.70759228668204,4.05414638576012));
#30776=CARTESIAN_POINT('Ctrl Pts',(4.0528214483761,3.69995677060634,4.19012241323843));
#30777=CARTESIAN_POINT('Ctrl Pts',(4.03408016206104,3.68255958253971,4.28686359329027));
#30778=CARTESIAN_POINT('Ctrl Pts',(3.98286183657991,3.65617121302278,4.42646405387441));
#30779=CARTESIAN_POINT('Ctrl Pts',(3.9573829285772,3.64674691834979,4.47482705790048));
#30780=CARTESIAN_POINT('Ctrl Pts',(3.90811412259945,3.63901242276528,4.54353143773204));
#30781=CARTESIAN_POINT('Ctrl Pts',(3.88540052355725,3.63781801821782,4.56934838942208));
#30782=CARTESIAN_POINT('Ctrl Pts',(3.84255131673683,3.64282346565182,4.60714056402289));
#30783=CARTESIAN_POINT('Ctrl Pts',(3.82381431858832,3.64688258800408,4.62089194101728));
#30784=CARTESIAN_POINT('Ctrl Pts',(3.78407855336266,3.66118003477434,4.64388394673189));
#30785=CARTESIAN_POINT('Ctrl Pts',(3.7634883314087,3.67158392110797,4.65258978726599));
#30786=CARTESIAN_POINT('Ctrl Pts',(3.73765637855118,3.69002352815742,4.65886310574998));
#30787=CARTESIAN_POINT('Ctrl Pts',(3.73162197364763,3.69475680491063,4.65995935047192));
#30788=CARTESIAN_POINT('Ctrl Pts',(3.72229136106665,3.70280721963516,4.661036848069));
#30789=CARTESIAN_POINT('Ctrl Pts',(3.71888330952516,3.70591534050851,4.66128876278955));
#30790=CARTESIAN_POINT('Ctrl Pts',(3.71262653960873,3.71194846961323,4.6614766362689));
#30791=CARTESIAN_POINT('Ctrl Pts',(3.70976435135452,3.71484643897443,4.66144660123004));
#30792=CARTESIAN_POINT('Ctrl Pts',(3.70352661430894,3.72147898365233,4.66111486035927));
#30793=CARTESIAN_POINT('Ctrl Pts',(3.70019664454575,3.72524149667361,4.6607514048391));
#30794=CARTESIAN_POINT('Ctrl Pts',(3.69087839066038,3.73642953822813,4.65917598249656));
#30795=CARTESIAN_POINT('Ctrl Pts',(3.68525404166196,3.7440380470271,4.65750148702094));
#30796=CARTESIAN_POINT('Ctrl Pts',(3.66727588008421,3.77141154503087,4.64948528566702));
#30797=CARTESIAN_POINT('Ctrl Pts',(3.65790971120312,3.79165341557608,4.64009844156317));
#30798=CARTESIAN_POINT('Ctrl Pts',(3.64480204513195,3.831810793896,4.61539308723159));
#30799=CARTESIAN_POINT('Ctrl Pts',(3.6412949354228,3.85130089179904,4.60019195379197));
#30800=CARTESIAN_POINT('Ctrl Pts',(3.63797818771934,3.89324322780353,4.56080656181529));
#30801=CARTESIAN_POINT('Ctrl Pts',(3.63967487324229,3.91462066258948,4.53533737515856));
#30802=CARTESIAN_POINT('Ctrl Pts',(3.6478250350946,3.96002463729993,4.46952174021337));
#30803=CARTESIAN_POINT('Ctrl Pts',(3.65651853940274,3.98331683505499,4.42457618200295));
#30804=CARTESIAN_POINT('Ctrl Pts',(3.6856269437163,4.04044793827739,4.27073174534987));
#30805=CARTESIAN_POINT('Ctrl Pts',(3.70833861009888,4.06180067862148,4.14407324412992));
#30806=CARTESIAN_POINT('Ctrl Pts',(3.70833861009888,4.06180067862148,4.));
#30807=CARTESIAN_POINT('',(4.06180067862149,3.70833861009886,0.));
#30808=CARTESIAN_POINT('',(4.0618006786215,3.70833861009886,0.));
#30809=CARTESIAN_POINT('',(3.70833861009886,4.0618006786215,0.));
#30810=CARTESIAN_POINT('Origin',(3.88908729652601,3.88908729652601,0.));
#30811=CARTESIAN_POINT('',(3.70833861009886,4.06180067862149,0.));
#30812=CARTESIAN_POINT('Origin',(4.44959346906221,3.2328188876086,0.));
#30813=CARTESIAN_POINT('',(4.59190513875472,3.02727719191323,4.));
#30814=CARTESIAN_POINT('',(4.29808842443363,3.43168120543702,4.));
#30815=CARTESIAN_POINT('Ctrl Pts',(4.59190513875472,3.02727719191322,4.));
#30816=CARTESIAN_POINT('Ctrl Pts',(4.59190513875472,3.02727719191322,4.02673063961771));
#30817=CARTESIAN_POINT('Ctrl Pts',(4.59102894698104,3.02666034062482,4.05414638576008));
#30818=CARTESIAN_POINT('Ctrl Pts',(4.58172524915676,3.02040320785364,4.19012241323846));
#30819=CARTESIAN_POINT('Ctrl Pts',(4.56049317936719,3.00615199113995,4.28686359329029));
#30820=CARTESIAN_POINT('Ctrl Pts',(4.5057773859961,2.98810081758768,4.42646405387423));
#30821=CARTESIAN_POINT('Ctrl Pts',(4.47913788113519,2.98277833096402,4.47482705790036));
#30822=CARTESIAN_POINT('Ctrl Pts',(4.42926571423672,2.98284639916111,4.54353143773204));
#30823=CARTESIAN_POINT('Ctrl Pts',(4.40664491125335,2.98521988943094,4.56934838942208));
#30824=CARTESIAN_POINT('Ctrl Pts',(4.3651062737647,2.99686680424732,4.60714056402289));
#30825=CARTESIAN_POINT('Ctrl Pts',(4.34723494578937,3.00380706434951,4.62089194101728));
#30826=CARTESIAN_POINT('Ctrl Pts',(4.3102250072083,3.02414452900082,4.6438839467319));
#30827=CARTESIAN_POINT('Ctrl Pts',(4.29151581144705,3.03764134658586,4.65258978726599));
#30828=CARTESIAN_POINT('Ctrl Pts',(4.26888648285923,3.05989493919995,4.65886310574998));
#30829=CARTESIAN_POINT('Ctrl Pts',(4.26366681911034,3.06551393036484,4.65995935047192));
#30830=CARTESIAN_POINT('Ctrl Pts',(4.25571044417427,3.07492486051281,4.661036848069));
#30831=CARTESIAN_POINT('Ctrl Pts',(4.2528305686287,3.0785278519803,4.66128876278955));
#30832=CARTESIAN_POINT('Ctrl Pts',(4.24759461925646,3.08546547770911,4.6614766362689));
#30833=CARTESIAN_POINT('Ctrl Pts',(4.24522101157591,3.08877551314697,4.66144660123004));
#30834=CARTESIAN_POINT('Ctrl Pts',(4.24009763000285,3.09630219725156,4.66111486035927));
#30835=CARTESIAN_POINT('Ctrl Pts',(4.2373972444049,3.10053930953252,4.66075140483911));
#30836=CARTESIAN_POINT('Ctrl Pts',(4.22994390898303,3.11304730379171,4.65917598249656));
#30837=CARTESIAN_POINT('Ctrl Pts',(4.22557903805757,3.12144198124854,4.65750148702093));
#30838=CARTESIAN_POINT('Ctrl Pts',(4.21210437599839,3.15129087015698,4.64948528566701));
#30839=CARTESIAN_POINT('Ctrl Pts',(4.20602004638866,3.1727487213047,4.64009844156317));
#30840=CARTESIAN_POINT('Ctrl Pts',(4.19935575543264,3.21446218638994,4.61539308723158));
#30841=CARTESIAN_POINT('Ctrl Pts',(4.19894074710277,3.23426096167702,4.60019195379196));
#30842=CARTESIAN_POINT('Ctrl Pts',(4.20222606096277,3.27620577157864,4.56080656181527));
#30843=CARTESIAN_POINT('Ctrl Pts',(4.20724602504612,3.29705459457643,4.53533737515852));
#30844=CARTESIAN_POINT('Ctrl Pts',(4.22239859137616,3.3406246048053,4.46952174021328));
#30845=CARTESIAN_POINT('Ctrl Pts',(4.23462876671566,3.36227007325903,4.42457618200282));
#30846=CARTESIAN_POINT('Ctrl Pts',(4.27231607183923,3.41414424014013,4.27073174534982));
#30847=CARTESIAN_POINT('Ctrl Pts',(4.29808842443364,3.431681205437,4.14407324412984));
#30848=CARTESIAN_POINT('Ctrl Pts',(4.29808842443364,3.431681205437,4.));
#30849=CARTESIAN_POINT('',(4.59190513875472,3.02727719191323,0.));
#30850=CARTESIAN_POINT('',(4.59190513875472,3.02727719191322,0.));
#30851=CARTESIAN_POINT('',(4.29808842443363,3.43168120543702,0.));
#30852=CARTESIAN_POINT('Origin',(4.44959346906221,3.2328188876086,0.));
#30853=CARTESIAN_POINT('',(4.29808842443363,3.43168120543702,0.));
#30854=CARTESIAN_POINT('Origin',(4.90053588303602,2.49694774856751,0.));
#30855=CARTESIAN_POINT('',(5.00894165471237,2.2716741623057,4.));
#30856=CARTESIAN_POINT('',(4.78200503722117,2.71706235187773,4.));
#30857=CARTESIAN_POINT('Ctrl Pts',(5.00894165471237,2.2716741623057,4.));
#30858=CARTESIAN_POINT('Ctrl Pts',(5.00894165471237,2.2716741623057,4.02673063961773));
#30859=CARTESIAN_POINT('Ctrl Pts',(5.00797975351207,2.27120197207165,4.05414638576012));
#30860=CARTESIAN_POINT('Ctrl Pts',(4.99781176842886,2.26647729398004,4.19012241323845));
#30861=CARTESIAN_POINT('Ctrl Pts',(4.97461171918823,2.25572296087186,4.28686359329029));
#30862=CARTESIAN_POINT('Ctrl Pts',(4.91774574235111,2.24645346308547,4.42646405387443));
#30863=CARTESIAN_POINT('Ctrl Pts',(4.89060159365309,2.24536384179619,4.47482705790049));
#30864=CARTESIAN_POINT('Ctrl Pts',(4.84135408409934,2.25323279770997,4.54353143773205));
#30865=CARTESIAN_POINT('Ctrl Pts',(4.81938307641841,2.25911573958948,4.56934838942209));
#30866=CARTESIAN_POINT('Ctrl Pts',(4.78017782737534,2.27711733609155,4.60714056402289));
#30867=CARTESIAN_POINT('Ctrl Pts',(4.76361222097947,2.28676784170657,4.62089194101728));
#30868=CARTESIAN_POINT('Ctrl Pts',(4.73023941655983,2.31264454836303,4.6438839467319));
#30869=CARTESIAN_POINT('Ctrl Pts',(4.71387192948318,2.32890196075716,4.65258978726599));
#30870=CARTESIAN_POINT('Ctrl Pts',(4.6950024343373,2.3544215816303,4.65886310574997));
#30871=CARTESIAN_POINT('Ctrl Pts',(4.69072603718763,2.36078792899602,4.65995935047192));
#30872=CARTESIAN_POINT('Ctrl Pts',(4.68433981225311,2.37132764623411,4.661036848069));
#30873=CARTESIAN_POINT('Ctrl Pts',(4.68205902479715,2.37533679068817,4.66128876278955));
#30874=CARTESIAN_POINT('Ctrl Pts',(4.67797282241977,2.38300808567095,4.6614766362689));
#30875=CARTESIAN_POINT('Ctrl Pts',(4.67614624141153,2.38664868312759,4.66144660123004));
#30876=CARTESIAN_POINT('Ctrl Pts',(4.67226336996882,2.39488417471663,4.66111486035927));
#30877=CARTESIAN_POINT('Ctrl Pts',(4.67025906099161,2.39949155449074,4.66075140483911));
#30878=CARTESIAN_POINT('Ctrl Pts',(4.66485416988754,2.41301151312426,4.65917598249656));
#30879=CARTESIAN_POINT('Ctrl Pts',(4.66185625464341,2.42198565441962,4.65750148702093));
#30880=CARTESIAN_POINT('Ctrl Pts',(4.65321688300254,2.45357495552503,4.64948528566701));
#30881=CARTESIAN_POINT('Ctrl Pts',(4.65056420905187,2.47572042376549,4.64009844156317));
#30882=CARTESIAN_POINT('Ctrl Pts',(4.65050739017187,2.51796285166657,4.61539308723158));
#30883=CARTESIAN_POINT('Ctrl Pts',(4.65319470210369,2.53758279278176,4.60019195379196));
#30884=CARTESIAN_POINT('Ctrl Pts',(4.66300118219658,2.57849725615389,4.56080656181528));
#30885=CARTESIAN_POINT('Ctrl Pts',(4.67122081666429,2.59830410014804,4.53533737515854));
#30886=CARTESIAN_POINT('Ctrl Pts',(4.69300268100047,2.63896730764281,4.4695217402134));
#30887=CARTESIAN_POINT('Ctrl Pts',(4.70846837986482,2.65843306352472,4.424576182003));
#30888=CARTESIAN_POINT('Ctrl Pts',(4.75380659926932,2.70377297991551,4.27073174534984));
#30889=CARTESIAN_POINT('Ctrl Pts',(4.78200503722118,2.71706235187771,4.14407324412987));
#30890=CARTESIAN_POINT('Ctrl Pts',(4.78200503722118,2.71706235187771,4.));
#30891=CARTESIAN_POINT('',(5.00894165471237,2.2716741623057,0.));
#30892=CARTESIAN_POINT('',(5.00894165471237,2.2716741623057,0.));
#30893=CARTESIAN_POINT('',(4.78200503722117,2.71706235187773,0.));
#30894=CARTESIAN_POINT('Origin',(4.90053588303602,2.49694774856751,0.));
#30895=CARTESIAN_POINT('',(4.78200503722117,2.71706235187773,0.));
#30896=CARTESIAN_POINT('Origin',(5.23081083962335,1.69959346906221,0.));
#30897=CARTESIAN_POINT('',(5.30264140340673,1.46013497556791,4.));
#30898=CARTESIAN_POINT('',(5.14817281542751,1.93554040580225,4.));
#30899=CARTESIAN_POINT('Ctrl Pts',(5.30264140340673,1.46013497556791,4.));
#30900=CARTESIAN_POINT('Ctrl Pts',(5.30264140340673,1.46013497556791,4.02673063961776));
#30901=CARTESIAN_POINT('Ctrl Pts',(5.30161747797973,1.45981907327888,4.05414638576018));
#30902=CARTESIAN_POINT('Ctrl Pts',(5.29083557517593,1.45674318712175,4.19012241323858));
#30903=CARTESIAN_POINT('Ctrl Pts',(5.26623880869307,1.4497505449918,4.28686359329039));
#30904=CARTESIAN_POINT('Ctrl Pts',(5.2086228774672,1.44949096877052,4.42646405387422));
#30905=CARTESIAN_POINT('Ctrl Pts',(5.18164246395932,1.45266104290794,4.47482705790035));
#30906=CARTESIAN_POINT('Ctrl Pts',(5.13423224887842,1.46813712672829,4.54353143773208));
#30907=CARTESIAN_POINT('Ctrl Pts',(5.11345203562662,1.47738466266404,4.5693483894221));
#30908=CARTESIAN_POINT('Ctrl Pts',(5.07754553837533,1.50129768180206,4.6071405640229));
#30909=CARTESIAN_POINT('Ctrl Pts',(5.0626935537665,1.51342080545347,4.62089194101728));
#30910=CARTESIAN_POINT('Ctrl Pts',(5.03377963271106,1.54419958371734,4.6438839467319));
#30911=CARTESIAN_POINT('Ctrl Pts',(5.02015687617143,1.56281727947215,4.65258978726599));
#30912=CARTESIAN_POINT('Ctrl Pts',(5.00551184406225,1.59097455084369,4.65886310574997));
#30913=CARTESIAN_POINT('Ctrl Pts',(5.00228401260219,1.59793149380939,4.65995935047191));
#30914=CARTESIAN_POINT('Ctrl Pts',(4.99762518772177,1.60934047531985,4.66103684806899));
#30915=CARTESIAN_POINT('Ctrl Pts',(4.99599964891208,1.61365705431844,4.66128876278954));
#30916=CARTESIAN_POINT('Ctrl Pts',(4.99316380939342,1.62187312581317,4.6614766362689));
#30917=CARTESIAN_POINT('Ctrl Pts',(4.99192923154398,1.62575464169678,4.66144660123003));
#30918=CARTESIAN_POINT('Ctrl Pts',(4.98938247941308,1.63449615563528,4.66111486035926));
#30919=CARTESIAN_POINT('Ctrl Pts',(4.98812359979553,1.63936035392149,4.6607514048391));
#30920=CARTESIAN_POINT('Ctrl Pts',(4.98490023936606,1.6535593706776,4.65917598249655));
#30921=CARTESIAN_POINT('Ctrl Pts',(4.98334309842607,1.66289200266933,4.65750148702093));
#30922=CARTESIAN_POINT('Ctrl Pts',(4.97975174720573,1.69544388253964,4.649485285667));
#30923=CARTESIAN_POINT('Ctrl Pts',(4.98059604655052,1.71773167294816,4.64009844156315));
#30924=CARTESIAN_POINT('Ctrl Pts',(4.98714809881592,1.75946291489558,4.61539308723157));
#30925=CARTESIAN_POINT('Ctrl Pts',(4.992871560471,1.77842091377375,4.60019195379196));
#30926=CARTESIAN_POINT('Ctrl Pts',(5.00895773871105,1.81729758074086,4.56080656181526));
#30927=CARTESIAN_POINT('Ctrl Pts',(5.02017464888312,1.83557473549709,4.53533737515852));
#30928=CARTESIAN_POINT('Ctrl Pts',(5.04804946943565,1.87232987713585,4.46952174021341));
#30929=CARTESIAN_POINT('Ctrl Pts',(5.06636987499111,1.88913660893297,4.42457618200302));
#30930=CARTESIAN_POINT('Ctrl Pts',(5.11824263124586,1.9268258556173,4.27073174534981));
#30931=CARTESIAN_POINT('Ctrl Pts',(5.14817281542752,1.93554040580223,4.14407324412983));
#30932=CARTESIAN_POINT('Ctrl Pts',(5.14817281542752,1.93554040580223,4.));
#30933=CARTESIAN_POINT('',(5.30264140340673,1.46013497556791,0.));
#30934=CARTESIAN_POINT('',(5.30264140340673,1.46013497556791,0.));
#30935=CARTESIAN_POINT('',(5.14817281542751,1.93554040580225,0.));
#30936=CARTESIAN_POINT('Origin',(5.23081083962335,1.69959346906221,0.));
#30937=CARTESIAN_POINT('',(5.14817281542751,1.93554040580225,0.));
#30938=CARTESIAN_POINT('Origin',(5.43228587327326,0.86038955772127,0.));
#30939=CARTESIAN_POINT('',(5.46577252229136,0.612642419821478,4.));
#30940=CARTESIAN_POINT('',(5.38757549311203,1.1063590312456,4.));
#30941=CARTESIAN_POINT('Ctrl Pts',(5.46577252229136,0.612642419821478,4.));
#30942=CARTESIAN_POINT('Ctrl Pts',(5.46577252229136,0.612642419821478,4.02673063961772));
#30943=CARTESIAN_POINT('Ctrl Pts',(5.46471178507988,0.612490584040257,4.0541463857601));
#30944=CARTESIAN_POINT('Ctrl Pts',(5.45358145078565,0.611139228343089,4.19012241323844));
#30945=CARTESIAN_POINT('Ctrl Pts',(5.42819362108338,0.608080459247841,4.28686359329029));
#30946=CARTESIAN_POINT('Ctrl Pts',(5.37124643091175,0.616837196219698,4.42646405387413));
#30947=CARTESIAN_POINT('Ctrl Pts',(5.34509409991741,0.624188908037709,4.47482705790029));
#30948=CARTESIAN_POINT('Ctrl Pts',(5.30068857615022,0.646891047218769,4.54353143773206));
#30949=CARTESIAN_POINT('Ctrl Pts',(5.2816108351434,0.659275472185214,4.56934838942208));
#30950=CARTESIAN_POINT('Ctrl Pts',(5.24988722681303,0.688511096065236,4.60714056402288));
#30951=CARTESIAN_POINT('Ctrl Pts',(5.23711456914321,0.702808326214387,4.62089194101727));
#30952=CARTESIAN_POINT('Ctrl Pts',(5.21337148814817,0.737731300415894,4.64388394673189));
#30953=CARTESIAN_POINT('Ctrl Pts',(5.20282889962289,0.758250850073321,4.65258978726599));
#30954=CARTESIAN_POINT('Ctrl Pts',(5.19276893984501,0.788352446473467,4.65886310574997));
#30955=CARTESIAN_POINT('Ctrl Pts',(5.19066915399765,0.795728682014571,4.65995935047192));
#30956=CARTESIAN_POINT('Ctrl Pts',(5.18785244490161,0.8077260008085,4.661036848069));
#30957=CARTESIAN_POINT('Ctrl Pts',(5.18692218089855,0.812243725850719,4.66128876278954));
#30958=CARTESIAN_POINT('Ctrl Pts',(5.1854065320192,0.820802266909536,4.6614766362689));
#30959=CARTESIAN_POINT('Ctrl Pts',(5.18479435673255,0.824829125417031,4.66144660123003));
#30960=CARTESIAN_POINT('Ctrl Pts',(5.18364643340307,0.833861416620435,4.66111486035927));
#30961=CARTESIAN_POINT('Ctrl Pts',(5.18316398093936,0.838862660713559,4.66075140483911));
#30962=CARTESIAN_POINT('Ctrl Pts',(5.18220152101598,0.853391108675971,4.65917598249655));
#30963=CARTESIAN_POINT('Ctrl Pts',(5.18212349635794,0.862852430991219,4.65750148702092));
#30964=CARTESIAN_POINT('Ctrl Pts',(5.18366859654418,0.895565354310452,4.64948528566701));
#30965=CARTESIAN_POINT('Ctrl Pts',(5.18798907973248,0.917446667518238,4.64009844156317));
#30966=CARTESIAN_POINT('Ctrl Pts',(5.2009886698715,0.957639161837228,4.61539308723158));
#30967=CARTESIAN_POINT('Ctrl Pts',(5.20960735062881,0.975468409628032,4.60019195379195));
#30968=CARTESIAN_POINT('Ctrl Pts',(5.23157713192079,1.01135000762511,4.56080656181527));
#30969=CARTESIAN_POINT('Ctrl Pts',(5.245515120242,1.02764742893492,4.53533737515852));
#30970=CARTESIAN_POINT('Ctrl Pts',(5.27879652641762,1.0595894711472,4.46952174021347));
#30971=CARTESIAN_POINT('Ctrl Pts',(5.29952052947748,1.07332334134434,4.42457618200309));
#30972=CARTESIAN_POINT('Ctrl Pts',(5.35665054316768,1.10243388398541,4.27073174534985));
#30973=CARTESIAN_POINT('Ctrl Pts',(5.38757549311203,1.10635903124558,4.14407324412988));
#30974=CARTESIAN_POINT('Ctrl Pts',(5.38757549311203,1.10635903124558,4.));
#30975=CARTESIAN_POINT('',(5.46577252229136,0.612642419821478,0.));
#30976=CARTESIAN_POINT('',(5.46577252229136,0.612642419821478,0.));
#30977=CARTESIAN_POINT('',(5.38757549311203,1.1063590312456,0.));
#30978=CARTESIAN_POINT('Origin',(5.43228587327326,0.86038955772127,0.));
#30979=CARTESIAN_POINT('',(5.38757549311203,1.1063590312456,0.));
#30980=CARTESIAN_POINT('Origin',(5.5,-2.77555756156289E-16,0.));
#30981=CARTESIAN_POINT('',(5.49431818181818,-0.249935425544577,4.));
#30982=CARTESIAN_POINT('',(5.49431818181818,0.249935425544577,4.));
#30983=CARTESIAN_POINT('Ctrl Pts',(5.49431818181818,-0.249935425544577,
4.));
#30984=CARTESIAN_POINT('Ctrl Pts',(5.49431818181818,-0.249935425544577,
4.02673063961774));
#30985=CARTESIAN_POINT('Ctrl Pts',(5.49324675169276,-0.249919456117149,
4.05414638576014));
#30986=CARTESIAN_POINT('Ctrl Pts',(5.48204205167785,-0.2495130064922,4.19012241323845));
#30987=CARTESIAN_POINT('Ctrl Pts',(5.45648829138081,-0.248562585506152,
4.28686359329028));
#30988=CARTESIAN_POINT('Ctrl Pts',(5.4016120710822,-0.231005155267301,4.42646405387446));
#30989=CARTESIAN_POINT('Ctrl Pts',(5.37693177978508,-0.219652829312523,
4.47482705790052));
#30990=CARTESIAN_POINT('Ctrl Pts',(5.3366243587004,-0.190283636781565,4.54353143773205));
#30991=CARTESIAN_POINT('Ctrl Pts',(5.31971884723751,-0.175067268428654,
4.56934838942209));
#30992=CARTESIAN_POINT('Ctrl Pts',(5.29295926834979,-0.14122891789402,4.60714056402289));
#30993=CARTESIAN_POINT('Ctrl Pts',(5.28258044284084,-0.125109626503179,
4.62089194101728));
#30994=CARTESIAN_POINT('Ctrl Pts',(5.26459283535906,-0.086902375891581,
4.64388394673189));
#30995=CARTESIAN_POINT('Ctrl Pts',(5.25739000836648,-0.0649862317445868,
4.65258978726599));
#30996=CARTESIAN_POINT('Ctrl Pts',(5.25216283051672,-0.0336815115206723,
4.65886310574998));
#30997=CARTESIAN_POINT('Ctrl Pts',(5.25124279397842,-0.0260676108035159,
4.65995935047192));
#30998=CARTESIAN_POINT('Ctrl Pts',(5.25033755739286,-0.0137773685317611,
4.661036848069));
#30999=CARTESIAN_POINT('Ctrl Pts',(5.25012547438354,-0.00916973882987097,
4.66128876278955));
#31000=CARTESIAN_POINT('Ctrl Pts',(5.24996733644903,-0.00047946789193707,
4.6614766362689));
#31001=CARTESIAN_POINT('Ctrl Pts',(5.24999263751242,0.00359357861861347,
4.66144660123004));
#31002=CARTESIAN_POINT('Ctrl Pts',(5.25027180866649,0.0126942421010739,
4.66111486035927));
#31003=CARTESIAN_POINT('Ctrl Pts',(5.25057766293744,0.0177093847734224,
4.6607514048391));
#31004=CARTESIAN_POINT('Ctrl Pts',(5.25189980247768,0.0322095253359952,
4.65917598249656));
#31005=CARTESIAN_POINT('Ctrl Pts',(5.25330281532761,0.0415665688190047,
4.65750148702093));
#31006=CARTESIAN_POINT('Ctrl Pts',(5.25994632142597,0.0736350348471544,
4.64948528566701));
#31007=CARTESIAN_POINT('Ctrl Pts',(5.26763660382283,0.0945710803031198,
4.64009844156318));
#31008=CARTESIAN_POINT('Ctrl Pts',(5.28676363878308,0.132235154392277,4.61539308723158));
#31009=CARTESIAN_POINT('Ctrl Pts',(5.29806531811861,0.148496635843216,4.60019195379196));
#31010=CARTESIAN_POINT('Ctrl Pts',(5.32537773353357,0.180499640843384,4.56080656181528));
#31011=CARTESIAN_POINT('Ctrl Pts',(5.3416936004739,0.194416032106081,4.53533737515856));
#31012=CARTESIAN_POINT('Ctrl Pts',(5.37956209359802,0.220758455803131,4.46952174021337));
#31013=CARTESIAN_POINT('Ctrl Pts',(5.40217940042793,0.231081290935914,4.42457618200295));
#31014=CARTESIAN_POINT('Ctrl Pts',(5.4631599410128,0.250896331361503,4.27073174534984));
#31015=CARTESIAN_POINT('Ctrl Pts',(5.49431818181818,0.249935425544556,4.14407324412989));
#31016=CARTESIAN_POINT('Ctrl Pts',(5.49431818181818,0.249935425544556,4.));
#31017=CARTESIAN_POINT('',(5.49431818181818,-0.249935425544577,0.));
#31018=CARTESIAN_POINT('',(5.49431818181818,-0.249935425544577,0.));
#31019=CARTESIAN_POINT('',(5.49431818181818,0.249935425544577,0.));
#31020=CARTESIAN_POINT('Origin',(5.5,-2.77555756156289E-16,0.));
#31021=CARTESIAN_POINT('',(5.49431818181818,0.249935425544577,0.));
#31022=CARTESIAN_POINT('Origin',(5.43228587327326,-0.86038955772127,0.));
#31023=CARTESIAN_POINT('',(5.38757549311203,-1.1063590312456,4.));
#31024=CARTESIAN_POINT('',(5.46577252229136,-0.612642419821479,4.));
#31025=CARTESIAN_POINT('Ctrl Pts',(5.38757549311203,-1.1063590312456,4.));
#31026=CARTESIAN_POINT('Ctrl Pts',(5.38757549311203,-1.1063590312456,4.02673063961776));
#31027=CARTESIAN_POINT('Ctrl Pts',(5.38651975223822,-1.10617564982983,4.05414638576019));
#31028=CARTESIAN_POINT('Ctrl Pts',(5.37551658340325,-1.10402140302146,4.19012241323857));
#31029=CARTESIAN_POINT('Ctrl Pts',(5.35042611089801,-1.09908519447303,4.28686359329038));
#31030=CARTESIAN_POINT('Ctrl Pts',(5.29897209514011,-1.0731593931695,4.42646405387435));
#31031=CARTESIAN_POINT('Ctrl Pts',(5.27637155422115,-1.05808598501925,4.47482705790044));
#31032=CARTESIAN_POINT('Ctrl Pts',(5.24115473829854,-1.02277290612914,4.54353143773208));
#31033=CARTESIAN_POINT('Ctrl Pts',(5.226837726178,-1.00509927187884,4.56934838942211));
#31034=CARTESIAN_POINT('Ctrl Pts',(5.20570108637508,-0.967491407182789,
4.60714056402292));
#31035=CARTESIAN_POINT('Ctrl Pts',(5.19797165415638,-0.949946965001165,
4.62089194101729));
#31036=CARTESIAN_POINT('Ctrl Pts',(5.18618243478152,-0.909396227292144,
4.64388394673189));
#31037=CARTESIAN_POINT('Ctrl Pts',(5.182496726827,-0.88662313685999,4.65258978726599));
#31038=CARTESIAN_POINT('Ctrl Pts',(5.18223104137204,-0.854886118918637,
4.65886310574998));
#31039=CARTESIAN_POINT('Ctrl Pts',(5.1825134084958,-0.847222032530173,4.65995935047192));
#31040=CARTESIAN_POINT('Ctrl Pts',(5.18354193434976,-0.834941493334267,
4.661036848069));
#31041=CARTESIAN_POINT('Ctrl Pts',(5.18405325452173,-0.830357414107832,
4.66128876278954));
#31042=CARTESIAN_POINT('Ctrl Pts',(5.18525652141284,-0.821749396602635,
4.6614766362689));
#31043=CARTESIAN_POINT('Ctrl Pts',(5.18591867583012,-0.817730454011772,
4.66144660123003));
#31044=CARTESIAN_POINT('Ctrl Pts',(5.18761806734741,-0.808785506788643,
4.66111486035927));
#31045=CARTESIAN_POINT('Ctrl Pts',(5.1887046972058,-0.803879954994019,4.6607514048391));
#31046=CARTESIAN_POINT('Ctrl Pts',(5.19227888074625,-0.789765163415024,
4.65917598249656));
#31047=CARTESIAN_POINT('Ctrl Pts',(5.19512838427145,-0.780742800229044,
4.65750148702093));
#31048=CARTESIAN_POINT('Ctrl Pts',(5.20670671111326,-0.750108423554733,
4.64948528566701));
#31049=CARTESIAN_POINT('Ctrl Pts',(5.21757743244349,-0.730633160772468,
4.64009844156316));
#31050=CARTESIAN_POINT('Ctrl Pts',(5.24236094114524,-0.696424921417119,
4.61539308723158));
#31051=CARTESIAN_POINT('Ctrl Pts',(5.25606733420563,-0.682131617948136,
4.60019195379195));
#31052=CARTESIAN_POINT('Ctrl Pts',(5.28804986143138,-0.654795226139849,
4.56080656181526));
#31053=CARTESIAN_POINT('Ctrl Pts',(5.30634185619752,-0.643602532663006,
4.53533737515852));
#31054=CARTESIAN_POINT('Ctrl Pts',(5.34786498829094,-0.623508365378209,
4.46952174021347));
#31055=CARTESIAN_POINT('Ctrl Pts',(5.3718186857342,-0.616850747770234,4.42457618200311));
#31056=CARTESIAN_POINT('Ctrl Pts',(5.43514820992188,-0.606819121617703,
4.27073174534979));
#31057=CARTESIAN_POINT('Ctrl Pts',(5.46577252229136,-0.612642419821499,
4.14407324412982));
#31058=CARTESIAN_POINT('Ctrl Pts',(5.46577252229136,-0.612642419821499,
4.));
#31059=CARTESIAN_POINT('',(5.38757549311203,-1.1063590312456,0.));
#31060=CARTESIAN_POINT('',(5.38757549311203,-1.1063590312456,0.));
#31061=CARTESIAN_POINT('',(5.46577252229136,-0.612642419821479,0.));
#31062=CARTESIAN_POINT('Origin',(5.43228587327326,-0.86038955772127,0.));
#31063=CARTESIAN_POINT('',(5.46577252229136,-0.612642419821479,0.));
#31064=CARTESIAN_POINT('Origin',(5.23081083962335,-1.69959346906221,0.));
#31065=CARTESIAN_POINT('',(5.14817281542751,-1.93554040580225,4.));
#31066=CARTESIAN_POINT('',(5.30264140340673,-1.46013497556791,4.));
#31067=CARTESIAN_POINT('Ctrl Pts',(5.14817281542752,-1.93554040580225,4.));
#31068=CARTESIAN_POINT('Ctrl Pts',(5.14817281542752,-1.93554040580225,4.02673063961775));
#31069=CARTESIAN_POINT('Ctrl Pts',(5.14715875964944,-1.93519412785719,4.05414638576015));
#31070=CARTESIAN_POINT('Ctrl Pts',(5.13662805652859,-1.93134512857135,4.19012241323851));
#31071=CARTESIAN_POINT('Ctrl Pts',(5.11261868251874,-1.92254467829737,4.28686359329034));
#31072=CARTESIAN_POINT('Ctrl Pts',(5.06585383993552,-1.88888888520002,4.42646405387432));
#31073=CARTESIAN_POINT('Ctrl Pts',(5.04588954971903,-1.87046555218872,4.47482705790042));
#31074=CARTESIAN_POINT('Ctrl Pts',(5.01663049384449,-1.83007811213917,4.54353143773206));
#31075=CARTESIAN_POINT('Ctrl Pts',(5.00525451342013,-1.81038239552215,4.56934838942209));
#31076=CARTESIAN_POINT('Ctrl Pts',(4.99026126692246,-1.76993104710687,4.60714056402291));
#31077=CARTESIAN_POINT('Ctrl Pts',(4.98537155226774,-1.75139345652764,4.62089194101728));
#31078=CARTESIAN_POINT('Ctrl Pts',(4.98007101070696,-1.70949772546375,4.64388394673189));
#31079=CARTESIAN_POINT('Ctrl Pts',(4.97999317615251,-1.68642843781244,4.65258978726599));
#31080=CARTESIAN_POINT('Ctrl Pts',(4.98469552515001,-1.65504059286449,4.65886310574997));
#31081=CARTESIAN_POINT('Ctrl Pts',(4.98617334312012,-1.64751503604723,4.65995935047191));
#31082=CARTESIAN_POINT('Ctrl Pts',(4.98911030569358,-1.63554658755898,4.66103684806899));
#31083=CARTESIAN_POINT('Ctrl Pts',(4.99033243864725,-1.63109893405222,4.66128876278954));
#31084=CARTESIAN_POINT('Ctrl Pts',(4.9928674819397,-1.6227851279391,4.66147663626889));
#31085=CARTESIAN_POINT('Ctrl Pts',(4.99415018527155,-1.61891924897263,4.66144660123003));
#31086=CARTESIAN_POINT('Ctrl Pts',(4.99722795249295,-1.610350272296,4.66111486035926));
#31087=CARTESIAN_POINT('Ctrl Pts',(4.99906860150534,-1.60567510234485,4.6607514048391));
#31088=CARTESIAN_POINT('Ctrl Pts',(5.00480682078521,-1.59229321276246,4.65917598249655));
#31089=CARTESIAN_POINT('Ctrl Pts',(5.00903265075193,-1.58382769039864,4.65750148702093));
#31090=CARTESIAN_POINT('Ctrl Pts',(5.02526070150406,-1.5553817231016,4.64948528566701));
#31091=CARTESIAN_POINT('Ctrl Pts',(5.03904418853065,-1.53784678859743,4.64009844156316));
#31092=CARTESIAN_POINT('Ctrl Pts',(5.06887391873794,-1.50793670435944,4.61539308723158));
#31093=CARTESIAN_POINT('Ctrl Pts',(5.08464752863712,-1.49596352744056,4.60019195379196));
#31094=CARTESIAN_POINT('Ctrl Pts',(5.12051265170942,-1.47396686151477,4.56080656181526));
#31095=CARTESIAN_POINT('Ctrl Pts',(5.14033036468258,-1.4657734670836,4.53533737515852));
#31096=CARTESIAN_POINT('Ctrl Pts',(5.18448569842586,-1.45242234129827,4.46952174021348));
#31097=CARTESIAN_POINT('Ctrl Pts',(5.20918596695366,-1.449593873856,4.42457618200312));
#31098=CARTESIAN_POINT('Ctrl Pts',(5.27330509167992,-1.44959267390549,4.27073174534981));
#31099=CARTESIAN_POINT('Ctrl Pts',(5.30264140340673,-1.46013497556793,4.14407324412984));
#31100=CARTESIAN_POINT('Ctrl Pts',(5.30264140340673,-1.46013497556793,4.));
#31101=CARTESIAN_POINT('',(5.14817281542751,-1.93554040580225,0.));
#31102=CARTESIAN_POINT('',(5.14817281542751,-1.93554040580225,0.));
#31103=CARTESIAN_POINT('',(5.30264140340673,-1.46013497556791,0.));
#31104=CARTESIAN_POINT('Origin',(5.23081083962335,-1.69959346906221,0.));
#31105=CARTESIAN_POINT('',(5.30264140340673,-1.46013497556791,0.));
#31106=CARTESIAN_POINT('Origin',(4.90053588303602,-2.49694774856751,0.));
#31107=CARTESIAN_POINT('',(4.78200503722117,-2.71706235187773,4.));
#31108=CARTESIAN_POINT('',(5.00894165471237,-2.2716741623057,4.));
#31109=CARTESIAN_POINT('Ctrl Pts',(4.78200503722117,-2.71706235187773,4.));
#31110=CARTESIAN_POINT('Ctrl Pts',(4.78200503722117,-2.71706235187773,4.02673063961772));
#31111=CARTESIAN_POINT('Ctrl Pts',(4.78105763595755,-2.71656170391563,4.0541463857601));
#31112=CARTESIAN_POINT('Ctrl Pts',(4.77125869941104,-2.71111272728885,4.19012241323846));
#31113=CARTESIAN_POINT('Ctrl Pts',(4.74892161436725,-2.69866473158207,4.28686359329029));
#31114=CARTESIAN_POINT('Ctrl Pts',(4.70799745058672,-2.65810766401414,4.42646405387428));
#31115=CARTESIAN_POINT('Ctrl Pts',(4.69116099815552,-2.63678804974405,4.47482705790039));
#31116=CARTESIAN_POINT('Ctrl Pts',(4.6685801573899,-2.5923207213473,4.54353143773206));
#31117=CARTESIAN_POINT('Ctrl Pts',(4.66042532305449,-2.57108789627302,4.56934838942209));
#31118=CARTESIAN_POINT('Ctrl Pts',(4.65194465335057,-2.52878911058683,4.60714056402289));
#31119=CARTESIAN_POINT('Ctrl Pts',(4.65001505726266,-2.50971482861278,4.62089194101728));
#31120=CARTESIAN_POINT('Ctrl Pts',(4.65133371044068,-2.46750571613676,4.6438839467319));
#31121=CARTESIAN_POINT('Ctrl Pts',(4.65486566583135,-2.44470827369084,4.65258978726599));
#31122=CARTESIAN_POINT('Ctrl Pts',(4.66442026184278,-2.41444247464922,4.65886310574997));
#31123=CARTESIAN_POINT('Ctrl Pts',(4.66705714187622,-2.40724075158791,4.65995935047192));
#31124=CARTESIAN_POINT('Ctrl Pts',(4.67183022340342,-2.39587909673005,4.661036848069));
#31125=CARTESIAN_POINT('Ctrl Pts',(4.67373307616942,-2.39167738493324,4.66128876278955));
#31126=CARTESIAN_POINT('Ctrl Pts',(4.67753747468404,-2.38386250371066,4.6614766362689));
#31127=CARTESIAN_POINT('Ctrl Pts',(4.67940914251737,-2.38024487913885,4.66144660123004));
#31128=CARTESIAN_POINT('Ctrl Pts',(4.68378950059938,-2.37226286965329,4.66111486035927));
#31129=CARTESIAN_POINT('Ctrl Pts',(4.68633884587832,-2.36793319974582,4.66075140483911));
#31130=CARTESIAN_POINT('Ctrl Pts',(4.69409980689487,-2.35561371869349,4.65917598249656));
#31131=CARTESIAN_POINT('Ctrl Pts',(4.69959790934461,-2.34791348640789,4.65750148702094));
#31132=CARTESIAN_POINT('Ctrl Pts',(4.72007609553975,-2.32235636260971,4.64948528566701));
#31133=CARTESIAN_POINT('Ctrl Pts',(4.73643295306733,-2.30719352466623,4.64009844156317));
#31134=CARTESIAN_POINT('Ctrl Pts',(4.77057439782324,-2.28231808108542,4.61539308723158));
#31135=CARTESIAN_POINT('Ctrl Pts',(4.7880268259359,-2.2729598500691,4.60019195379196));
#31136=CARTESIAN_POINT('Ctrl Pts',(4.82689142649519,-2.25684454094364,4.56080656181527));
#31137=CARTESIAN_POINT('Ctrl Pts',(4.84774687981075,-2.25185219412135,4.53533737515851));
#31138=CARTESIAN_POINT('Ctrl Pts',(4.893447164344,-2.24557285886217,4.46952174021346));
#31139=CARTESIAN_POINT('Ctrl Pts',(4.91828580136969,-2.24664318784119,4.42457618200308));
#31140=CARTESIAN_POINT('Ctrl Pts',(4.98161570098458,-2.25667244363946,4.27073174534982));
#31141=CARTESIAN_POINT('Ctrl Pts',(5.00894165471236,-2.27167416230572,4.14407324412985));
#31142=CARTESIAN_POINT('Ctrl Pts',(5.00894165471236,-2.27167416230572,4.));
#31143=CARTESIAN_POINT('',(4.78200503722117,-2.71706235187773,0.));
#31144=CARTESIAN_POINT('',(4.78200503722117,-2.71706235187773,0.));
#31145=CARTESIAN_POINT('',(5.00894165471237,-2.2716741623057,0.));
#31146=CARTESIAN_POINT('Origin',(4.90053588303602,-2.49694774856751,0.));
#31147=CARTESIAN_POINT('',(5.00894165471237,-2.2716741623057,0.));
#31148=CARTESIAN_POINT('Origin',(4.44959346906221,-3.2328188876086,0.));
#31149=CARTESIAN_POINT('',(4.29808842443363,-3.43168120543702,4.));
#31150=CARTESIAN_POINT('',(4.59190513875472,-3.02727719191323,4.));
#31151=CARTESIAN_POINT('Ctrl Pts',(4.29808842443363,-3.43168120543702,4.));
#31152=CARTESIAN_POINT('Ctrl Pts',(4.29808842443363,-3.43168120543702,4.02673063961769));
#31153=CARTESIAN_POINT('Ctrl Pts',(4.29723100584781,-3.43103851507226,4.05414638576003));
#31154=CARTESIAN_POINT('Ctrl Pts',(4.28840511821423,-3.4241237329932,4.19012241323837));
#31155=CARTESIAN_POINT('Ctrl Pts',(4.26829033530281,-3.40833470282046,4.28686359329022));
#31156=CARTESIAN_POINT('Ctrl Pts',(4.23421453905673,-3.36187501038663,4.42646405387436));
#31157=CARTESIAN_POINT('Ctrl Pts',(4.22092049374666,-3.3381840745168,4.47482705790044));
#31158=CARTESIAN_POINT('Ctrl Pts',(4.20557388333116,-3.29073179097666,4.54353143773201));
#31159=CARTESIAN_POINT('Ctrl Pts',(4.20084099417037,-3.26848468006614,4.56934838942206));
#31160=CARTESIAN_POINT('Ctrl Pts',(4.19908172349404,-3.22537999359422,4.6071405640229));
#31161=CARTESIAN_POINT('Ctrl Pts',(4.20015975903259,-3.20623869235147,4.62089194101727));
#31162=CARTESIAN_POINT('Ctrl Pts',(4.20806513733181,-3.16475552689654,4.64388394673188));
#31163=CARTESIAN_POINT('Ctrl Pts',(4.21511991420399,-3.14279127834939,4.65258978726599));
#31164=CARTESIAN_POINT('Ctrl Pts',(4.22929149136567,-3.1143927696329,4.65886310574997));
#31165=CARTESIAN_POINT('Ctrl Pts',(4.23302250472471,-3.10769221065045,4.65995935047192));
#31166=CARTESIAN_POINT('Ctrl Pts',(4.23951417609748,-3.0972171110728,4.661036848069));
#31167=CARTESIAN_POINT('Ctrl Pts',(4.24205089412553,-3.09336480107503,4.66128876278955));
#31168=CARTESIAN_POINT('Ctrl Pts',(4.24703097094481,-3.08624127305476,4.6614766362689));
#31169=CARTESIAN_POINT('Ctrl Pts',(4.24944551660588,-3.08296098080077,4.66144660123004));
#31170=CARTESIAN_POINT('Ctrl Pts',(4.25502060659492,-3.07576248207062,4.66111486035927));
#31171=CARTESIAN_POINT('Ctrl Pts',(4.25821587479886,-3.0718849230493,4.66075140483911));
#31172=CARTESIAN_POINT('Ctrl Pts',(4.26780847693471,-3.06093119703656,4.65917598249656));
#31173=CARTESIAN_POINT('Ctrl Pts',(4.27444347033799,-3.05418586010367,4.65750148702094));
#31174=CARTESIAN_POINT('Ctrl Pts',(4.2986675510688,-3.03214688101148,4.64948528566702));
#31175=CARTESIAN_POINT('Ctrl Pts',(4.31719501897975,-3.01972949902144,4.64009844156317));
#31176=CARTESIAN_POINT('Ctrl Pts',(4.35480750260544,-3.00050121207564,4.61539308723159));
#31177=CARTESIAN_POINT('Ctrl Pts',(4.37350901223014,-2.99398835766768,4.60019195379197));
#31178=CARTESIAN_POINT('Ctrl Pts',(4.41441611482644,-2.98415121773687,4.56080656181528));
#31179=CARTESIAN_POINT('Ctrl Pts',(4.43579577800848,-2.98248284667088,4.53533737515853));
#31180=CARTESIAN_POINT('Ctrl Pts',(4.48191572065602,-2.98342992001184,4.46952174021336));
#31181=CARTESIAN_POINT('Ctrl Pts',(4.5062811165013,-2.98837269036048,4.42457618200294));
#31182=CARTESIAN_POINT('Ctrl Pts',(4.56726239869637,-3.00818544834456,4.27073174534984));
#31183=CARTESIAN_POINT('Ctrl Pts',(4.59190513875471,-3.02727719191324,4.14407324412988));
#31184=CARTESIAN_POINT('Ctrl Pts',(4.59190513875471,-3.02727719191324,4.));
#31185=CARTESIAN_POINT('',(4.29808842443363,-3.43168120543702,0.));
#31186=CARTESIAN_POINT('',(4.29808842443363,-3.43168120543702,0.));
#31187=CARTESIAN_POINT('',(4.59190513875472,-3.02727719191323,0.));
#31188=CARTESIAN_POINT('Origin',(4.44959346906221,-3.2328188876086,0.));
#31189=CARTESIAN_POINT('',(4.59190513875472,-3.02727719191322,0.));
#31190=CARTESIAN_POINT('Origin',(3.88908729652601,-3.88908729652601,0.));
#31191=CARTESIAN_POINT('',(3.70833861009886,-4.06180067862149,4.));
#31192=CARTESIAN_POINT('',(4.0618006786215,-3.70833861009886,4.));
#31193=CARTESIAN_POINT('Ctrl Pts',(3.70833861009886,-4.06180067862149,4.));
#31194=CARTESIAN_POINT('Ctrl Pts',(3.70833861009886,-4.06180067862149,4.02673063961773));
#31195=CARTESIAN_POINT('Ctrl Pts',(3.70759228668204,-4.06103177102382,4.05414638576013));
#31196=CARTESIAN_POINT('Ctrl Pts',(3.69995677060634,-4.0528214483761,4.19012241323846));
#31197=CARTESIAN_POINT('Ctrl Pts',(3.68255958253971,-4.03408016206103,4.2868635932903));
#31198=CARTESIAN_POINT('Ctrl Pts',(3.6561712130228,-3.98286183657994,4.42646405387435));
#31199=CARTESIAN_POINT('Ctrl Pts',(3.64674691834979,-3.95738292857724,4.47482705790044));
#31200=CARTESIAN_POINT('Ctrl Pts',(3.63901242276528,-3.90811412259946,4.54353143773204));
#31201=CARTESIAN_POINT('Ctrl Pts',(3.63781801821782,-3.88540052355725,4.56934838942208));
#31202=CARTESIAN_POINT('Ctrl Pts',(3.64282346565182,-3.84255131673681,4.60714056402291));
#31203=CARTESIAN_POINT('Ctrl Pts',(3.64688258800408,-3.8238143185883,4.62089194101728));
#31204=CARTESIAN_POINT('Ctrl Pts',(3.66118003477434,-3.78407855336266,4.6438839467319));
#31205=CARTESIAN_POINT('Ctrl Pts',(3.67158392110798,-3.76348833140869,4.65258978726599));
#31206=CARTESIAN_POINT('Ctrl Pts',(3.69002352815741,-3.73765637855119,4.65886310574997));
#31207=CARTESIAN_POINT('Ctrl Pts',(3.69475680491063,-3.73162197364764,4.65995935047192));
#31208=CARTESIAN_POINT('Ctrl Pts',(3.70280721963516,-3.72229136106665,4.661036848069));
#31209=CARTESIAN_POINT('Ctrl Pts',(3.70591534050851,-3.71888330952516,4.66128876278955));
#31210=CARTESIAN_POINT('Ctrl Pts',(3.71194846961324,-3.71262653960872,4.6614766362689));
#31211=CARTESIAN_POINT('Ctrl Pts',(3.71484643897445,-3.70976435135451,4.66144660123004));
#31212=CARTESIAN_POINT('Ctrl Pts',(3.72147898365232,-3.70352661430895,4.66111486035927));
#31213=CARTESIAN_POINT('Ctrl Pts',(3.72524149667359,-3.70019664454577,4.66075140483911));
#31214=CARTESIAN_POINT('Ctrl Pts',(3.73642953822814,-3.69087839066037,4.65917598249656));
#31215=CARTESIAN_POINT('Ctrl Pts',(3.74403804702711,-3.68525404166196,4.65750148702094));
#31216=CARTESIAN_POINT('Ctrl Pts',(3.77141154503086,-3.66727588008421,4.64948528566702));
#31217=CARTESIAN_POINT('Ctrl Pts',(3.79165341557607,-3.65790971120312,4.64009844156318));
#31218=CARTESIAN_POINT('Ctrl Pts',(3.83181079389601,-3.64480204513195,4.61539308723159));
#31219=CARTESIAN_POINT('Ctrl Pts',(3.85130089179905,-3.6412949354228,4.60019195379196));
#31220=CARTESIAN_POINT('Ctrl Pts',(3.89324322780354,-3.63797818771934,4.56080656181528));
#31221=CARTESIAN_POINT('Ctrl Pts',(3.91462066258949,-3.63967487324229,4.53533737515854));
#31222=CARTESIAN_POINT('Ctrl Pts',(3.96002463729994,-3.6478250350946,4.46952174021335));
#31223=CARTESIAN_POINT('Ctrl Pts',(3.983316835055,-3.65651853940275,4.42457618200292));
#31224=CARTESIAN_POINT('Ctrl Pts',(4.04044793827739,-3.68562694371631,4.27073174534986));
#31225=CARTESIAN_POINT('Ctrl Pts',(4.06180067862148,-3.70833861009888,4.1440732441299));
#31226=CARTESIAN_POINT('Ctrl Pts',(4.06180067862148,-3.70833861009888,4.));
#31227=CARTESIAN_POINT('',(3.70833861009886,-4.06180067862149,0.));
#31228=CARTESIAN_POINT('',(3.70833861009886,-4.06180067862149,0.));
#31229=CARTESIAN_POINT('',(4.0618006786215,-3.70833861009886,0.));
#31230=CARTESIAN_POINT('Origin',(3.88908729652601,-3.88908729652601,0.));
#31231=CARTESIAN_POINT('',(4.06180067862149,-3.70833861009886,0.));
#31232=CARTESIAN_POINT('Origin',(3.2328188876086,-4.44959346906221,0.));
#31233=CARTESIAN_POINT('',(3.02727719191323,-4.59190513875472,4.));
#31234=CARTESIAN_POINT('',(3.43168120543702,-4.29808842443363,4.));
#31235=CARTESIAN_POINT('Ctrl Pts',(3.02727719191322,-4.59190513875472,4.));
#31236=CARTESIAN_POINT('Ctrl Pts',(3.02727719191322,-4.59190513875472,4.02673063961775));
#31237=CARTESIAN_POINT('Ctrl Pts',(3.02666034062482,-4.59102894698104,4.05414638576016));
#31238=CARTESIAN_POINT('Ctrl Pts',(3.02040320785363,-4.58172524915675,4.19012241323852));
#31239=CARTESIAN_POINT('Ctrl Pts',(3.00615199113994,-4.56049317936718,4.28686359329035));
#31240=CARTESIAN_POINT('Ctrl Pts',(2.98810081758767,-4.50577738599606,4.42646405387433));
#31241=CARTESIAN_POINT('Ctrl Pts',(2.98277833096401,-4.47913788113514,4.47482705790043));
#31242=CARTESIAN_POINT('Ctrl Pts',(2.98284639916111,-4.4292657142367,4.54353143773207));
#31243=CARTESIAN_POINT('Ctrl Pts',(2.98521988943094,-4.40664491125333,4.5693483894221));
#31244=CARTESIAN_POINT('Ctrl Pts',(2.99686680424733,-4.36510627376467,4.60714056402292));
#31245=CARTESIAN_POINT('Ctrl Pts',(3.00380706434952,-4.34723494578935,4.62089194101729));
#31246=CARTESIAN_POINT('Ctrl Pts',(3.02414452900082,-4.31022500720831,4.6438839467319));
#31247=CARTESIAN_POINT('Ctrl Pts',(3.03764134658586,-4.29151581144705,4.65258978726599));
#31248=CARTESIAN_POINT('Ctrl Pts',(3.05989493919995,-4.26888648285923,4.65886310574998));
#31249=CARTESIAN_POINT('Ctrl Pts',(3.06551393036484,-4.26366681911033,4.65995935047192));
#31250=CARTESIAN_POINT('Ctrl Pts',(3.07492486051284,-4.25571044417424,4.661036848069));
#31251=CARTESIAN_POINT('Ctrl Pts',(3.07852785198032,-4.25283056862869,4.66128876278955));
#31252=CARTESIAN_POINT('Ctrl Pts',(3.08546547770909,-4.24759461925647,4.6614766362689));
#31253=CARTESIAN_POINT('Ctrl Pts',(3.08877551314693,-4.24522101157593,4.66144660123004));
#31254=CARTESIAN_POINT('Ctrl Pts',(3.09630219725157,-4.24009763000284,4.66111486035927));
#31255=CARTESIAN_POINT('Ctrl Pts',(3.10053930953254,-4.23739724440489,4.66075140483911));
#31256=CARTESIAN_POINT('Ctrl Pts',(3.11304730379171,-4.22994390898303,4.65917598249656));
#31257=CARTESIAN_POINT('Ctrl Pts',(3.12144198124853,-4.22557903805758,4.65750148702094));
#31258=CARTESIAN_POINT('Ctrl Pts',(3.15129087015698,-4.21210437599839,4.64948528566701));
#31259=CARTESIAN_POINT('Ctrl Pts',(3.17274872130471,-4.20602004638866,4.64009844156317));
#31260=CARTESIAN_POINT('Ctrl Pts',(3.21446218638993,-4.19935575543265,4.61539308723158));
#31261=CARTESIAN_POINT('Ctrl Pts',(3.23426096167702,-4.19894074710278,4.60019195379196));
#31262=CARTESIAN_POINT('Ctrl Pts',(3.27620577157864,-4.20222606096277,4.56080656181527));
#31263=CARTESIAN_POINT('Ctrl Pts',(3.29705459457642,-4.20724602504612,4.53533737515854));
#31264=CARTESIAN_POINT('Ctrl Pts',(3.34062460480514,-4.2223985913761,4.46952174021351));
#31265=CARTESIAN_POINT('Ctrl Pts',(3.36227007325892,-4.23462876671557,4.42457618200316));
#31266=CARTESIAN_POINT('Ctrl Pts',(3.41414424014014,-4.27231607183923,4.27073174534981));
#31267=CARTESIAN_POINT('Ctrl Pts',(3.431681205437,-4.29808842443364,4.14407324412984));
#31268=CARTESIAN_POINT('Ctrl Pts',(3.431681205437,-4.29808842443364,4.));
#31269=CARTESIAN_POINT('',(3.02727719191323,-4.59190513875472,0.));
#31270=CARTESIAN_POINT('',(3.02727719191322,-4.59190513875472,0.));
#31271=CARTESIAN_POINT('',(3.43168120543702,-4.29808842443363,0.));
#31272=CARTESIAN_POINT('Origin',(3.2328188876086,-4.44959346906221,0.));
#31273=CARTESIAN_POINT('',(3.43168120543702,-4.29808842443363,0.));
#31274=CARTESIAN_POINT('Origin',(2.49694774856751,-4.90053588303602,0.));
#31275=CARTESIAN_POINT('',(2.2716741623057,-5.00894165471237,4.));
#31276=CARTESIAN_POINT('',(2.71706235187773,-4.78200503722117,4.));
#31277=CARTESIAN_POINT('Ctrl Pts',(2.2716741623057,-5.00894165471237,4.));
#31278=CARTESIAN_POINT('Ctrl Pts',(2.2716741623057,-5.00894165471237,4.02673063961774));
#31279=CARTESIAN_POINT('Ctrl Pts',(2.27120197207165,-5.00797975351207,4.05414638576013));
#31280=CARTESIAN_POINT('Ctrl Pts',(2.26647729398003,-4.99781176842886,4.19012241323847));
#31281=CARTESIAN_POINT('Ctrl Pts',(2.25572296087185,-4.97461171918823,4.2868635932903));
#31282=CARTESIAN_POINT('Ctrl Pts',(2.24645346308548,-4.91774574235116,4.42646405387431));
#31283=CARTESIAN_POINT('Ctrl Pts',(2.24536384179618,-4.89060159365315,4.47482705790041));
#31284=CARTESIAN_POINT('Ctrl Pts',(2.25323279770997,-4.84135408409934,4.54353143773206));
#31285=CARTESIAN_POINT('Ctrl Pts',(2.25911573958948,-4.81938307641841,4.56934838942209));
#31286=CARTESIAN_POINT('Ctrl Pts',(2.27711733609156,-4.78017782737533,4.60714056402291));
#31287=CARTESIAN_POINT('Ctrl Pts',(2.28676784170657,-4.76361222097947,4.62089194101728));
#31288=CARTESIAN_POINT('Ctrl Pts',(2.31264454836303,-4.73023941655982,4.6438839467319));
#31289=CARTESIAN_POINT('Ctrl Pts',(2.32890196075716,-4.71387192948318,4.65258978726599));
#31290=CARTESIAN_POINT('Ctrl Pts',(2.35442158163029,-4.69500243433731,4.65886310574997));
#31291=CARTESIAN_POINT('Ctrl Pts',(2.36078792899601,-4.69072603718764,4.65995935047192));
#31292=CARTESIAN_POINT('Ctrl Pts',(2.37132764623416,-4.68433981225308,4.661036848069));
#31293=CARTESIAN_POINT('Ctrl Pts',(2.3753367906882,-4.68205902479713,4.66128876278955));
#31294=CARTESIAN_POINT('Ctrl Pts',(2.38300808567094,-4.67797282241977,4.6614766362689));
#31295=CARTESIAN_POINT('Ctrl Pts',(2.38664868312759,-4.67614624141154,4.66144660123004));
#31296=CARTESIAN_POINT('Ctrl Pts',(2.39488417471663,-4.67226336996883,4.66111486035927));
#31297=CARTESIAN_POINT('Ctrl Pts',(2.39949155449074,-4.67025906099161,4.66075140483911));
#31298=CARTESIAN_POINT('Ctrl Pts',(2.41301151312425,-4.66485416988755,4.65917598249656));
#31299=CARTESIAN_POINT('Ctrl Pts',(2.4219856544196,-4.66185625464342,4.65750148702094));
#31300=CARTESIAN_POINT('Ctrl Pts',(2.45357495552503,-4.65321688300254,4.64948528566701));
#31301=CARTESIAN_POINT('Ctrl Pts',(2.4757204237655,-4.65056420905187,4.64009844156317));
#31302=CARTESIAN_POINT('Ctrl Pts',(2.51796285166657,-4.65050739017187,4.61539308723158));
#31303=CARTESIAN_POINT('Ctrl Pts',(2.53758279278176,-4.65319470210369,4.60019195379196));
#31304=CARTESIAN_POINT('Ctrl Pts',(2.57849725615389,-4.66300118219658,4.56080656181528));
#31305=CARTESIAN_POINT('Ctrl Pts',(2.59830410014803,-4.67122081666428,4.53533737515855));
#31306=CARTESIAN_POINT('Ctrl Pts',(2.63896730764288,-4.69300268100051,4.46952174021329));
#31307=CARTESIAN_POINT('Ctrl Pts',(2.65843306352477,-4.70846837986487,4.42457618200283));
#31308=CARTESIAN_POINT('Ctrl Pts',(2.7037729799155,-4.75380659926932,4.27073174534984));
#31309=CARTESIAN_POINT('Ctrl Pts',(2.71706235187771,-4.78200503722118,4.14407324412987));
#31310=CARTESIAN_POINT('Ctrl Pts',(2.71706235187771,-4.78200503722118,4.));
#31311=CARTESIAN_POINT('',(2.2716741623057,-5.00894165471237,0.));
#31312=CARTESIAN_POINT('',(2.2716741623057,-5.00894165471237,0.));
#31313=CARTESIAN_POINT('',(2.71706235187773,-4.78200503722117,0.));
#31314=CARTESIAN_POINT('Origin',(2.49694774856751,-4.90053588303602,0.));
#31315=CARTESIAN_POINT('',(2.71706235187773,-4.78200503722117,0.));
#31316=CARTESIAN_POINT('Origin',(1.69959346906221,-5.23081083962335,0.));
#31317=CARTESIAN_POINT('',(1.46013497556791,-5.30264140340673,4.));
#31318=CARTESIAN_POINT('',(1.93554040580225,-5.14817281542751,4.));
#31319=CARTESIAN_POINT('Ctrl Pts',(1.46013497556791,-5.30264140340673,4.));
#31320=CARTESIAN_POINT('Ctrl Pts',(1.46013497556791,-5.30264140340673,4.0267306396177));
#31321=CARTESIAN_POINT('Ctrl Pts',(1.45981907327888,-5.30161747797973,4.05414638576006));
#31322=CARTESIAN_POINT('Ctrl Pts',(1.45674318712176,-5.29083557517596,4.19012241323839));
#31323=CARTESIAN_POINT('Ctrl Pts',(1.4497505449918,-5.26623880869312,4.28686359329023));
#31324=CARTESIAN_POINT('Ctrl Pts',(1.44949096877051,-5.20862287746716,4.42646405387434));
#31325=CARTESIAN_POINT('Ctrl Pts',(1.45266104290796,-5.18164246395926,4.47482705790043));
#31326=CARTESIAN_POINT('Ctrl Pts',(1.46813712672827,-5.13423224887846,4.54353143773201));
#31327=CARTESIAN_POINT('Ctrl Pts',(1.47738466266402,-5.11345203562666,4.56934838942206));
#31328=CARTESIAN_POINT('Ctrl Pts',(1.50129768180205,-5.07754553837534,4.6071405640229));
#31329=CARTESIAN_POINT('Ctrl Pts',(1.51342080545345,-5.06269355376651,4.62089194101727));
#31330=CARTESIAN_POINT('Ctrl Pts',(1.54419958371731,-5.03377963271108,4.64388394673188));
#31331=CARTESIAN_POINT('Ctrl Pts',(1.56281727947213,-5.02015687617145,4.65258978726598));
#31332=CARTESIAN_POINT('Ctrl Pts',(1.59097455084368,-5.00551184406225,4.65886310574997));
#31333=CARTESIAN_POINT('Ctrl Pts',(1.59793149380938,-5.0022840126022,4.65995935047191));
#31334=CARTESIAN_POINT('Ctrl Pts',(1.6093404753199,-4.99762518772175,4.66103684806899));
#31335=CARTESIAN_POINT('Ctrl Pts',(1.61365705431846,-4.99599964891207,4.66128876278954));
#31336=CARTESIAN_POINT('Ctrl Pts',(1.62187312581315,-4.99316380939343,4.66147663626889));
#31337=CARTESIAN_POINT('Ctrl Pts',(1.62575464169675,-4.991929231544,4.66144660123003));
#31338=CARTESIAN_POINT('Ctrl Pts',(1.63449615563527,-4.98938247941308,4.66111486035926));
#31339=CARTESIAN_POINT('Ctrl Pts',(1.63936035392147,-4.98812359979554,4.6607514048391));
#31340=CARTESIAN_POINT('Ctrl Pts',(1.6535593706776,-4.98490023936606,4.65917598249655));
#31341=CARTESIAN_POINT('Ctrl Pts',(1.66289200266933,-4.98334309842607,4.65750148702093));
#31342=CARTESIAN_POINT('Ctrl Pts',(1.69544388253963,-4.97975174720573,4.64948528566701));
#31343=CARTESIAN_POINT('Ctrl Pts',(1.71773167294815,-4.98059604655052,4.64009844156316));
#31344=CARTESIAN_POINT('Ctrl Pts',(1.75946291489558,-4.98714809881592,4.61539308723158));
#31345=CARTESIAN_POINT('Ctrl Pts',(1.77842091377376,-4.992871560471,4.60019195379195));
#31346=CARTESIAN_POINT('Ctrl Pts',(1.81729758074086,-5.00895773871105,4.56080656181527));
#31347=CARTESIAN_POINT('Ctrl Pts',(1.83557473549708,-5.02017464888312,4.53533737515853));
#31348=CARTESIAN_POINT('Ctrl Pts',(1.87232987713586,-5.04804946943565,4.4695217402134));
#31349=CARTESIAN_POINT('Ctrl Pts',(1.88913660893297,-5.06636987499112,4.424576182003));
#31350=CARTESIAN_POINT('Ctrl Pts',(1.92682585561729,-5.11824263124585,4.27073174534984));
#31351=CARTESIAN_POINT('Ctrl Pts',(1.93554040580223,-5.14817281542752,4.14407324412987));
#31352=CARTESIAN_POINT('Ctrl Pts',(1.93554040580223,-5.14817281542752,4.));
#31353=CARTESIAN_POINT('',(1.46013497556791,-5.30264140340673,0.));
#31354=CARTESIAN_POINT('',(1.46013497556791,-5.30264140340673,0.));
#31355=CARTESIAN_POINT('',(1.93554040580225,-5.14817281542751,0.));
#31356=CARTESIAN_POINT('Origin',(1.69959346906221,-5.23081083962335,0.));
#31357=CARTESIAN_POINT('',(1.93554040580225,-5.14817281542751,0.));
#31358=CARTESIAN_POINT('Origin',(0.86038955772127,-5.43228587327326,0.));
#31359=CARTESIAN_POINT('',(0.612642419821478,-5.46577252229136,4.));
#31360=CARTESIAN_POINT('',(1.1063590312456,-5.38757549311203,4.));
#31361=CARTESIAN_POINT('Ctrl Pts',(0.612642419821478,-5.46577252229136,
4.));
#31362=CARTESIAN_POINT('Ctrl Pts',(0.612642419821478,-5.46577252229136,
4.02673063961775));
#31363=CARTESIAN_POINT('Ctrl Pts',(0.612490584040258,-5.46471178507988,
4.05414638576016));
#31364=CARTESIAN_POINT('Ctrl Pts',(0.611139228343089,-5.45358145078564,
4.19012241323849));
#31365=CARTESIAN_POINT('Ctrl Pts',(0.608080459247835,-5.42819362108337,
4.28686359329032));
#31366=CARTESIAN_POINT('Ctrl Pts',(0.616837196219715,-5.37124643091163,
4.42646405387443));
#31367=CARTESIAN_POINT('Ctrl Pts',(0.624188908037774,-5.34509409991728,
4.47482705790049));
#31368=CARTESIAN_POINT('Ctrl Pts',(0.646891047218772,-5.30068857615022,
4.54353143773205));
#31369=CARTESIAN_POINT('Ctrl Pts',(0.659275472185216,-5.28161083514339,
4.56934838942209));
#31370=CARTESIAN_POINT('Ctrl Pts',(0.688511096065256,-5.24988722681301,
4.60714056402291));
#31371=CARTESIAN_POINT('Ctrl Pts',(0.702808326214403,-5.2371145691432,4.62089194101728));
#31372=CARTESIAN_POINT('Ctrl Pts',(0.737731300415902,-5.21337148814816,
4.64388394673189));
#31373=CARTESIAN_POINT('Ctrl Pts',(0.758250850073328,-5.20282889962289,
4.65258978726599));
#31374=CARTESIAN_POINT('Ctrl Pts',(0.788352446473466,-5.19276893984501,
4.65886310574997));
#31375=CARTESIAN_POINT('Ctrl Pts',(0.795728682014572,-5.19066915399765,
4.65995935047192));
#31376=CARTESIAN_POINT('Ctrl Pts',(0.80772600080848,-5.18785244490161,4.661036848069));
#31377=CARTESIAN_POINT('Ctrl Pts',(0.812243725850711,-5.18692218089855,
4.66128876278954));
#31378=CARTESIAN_POINT('Ctrl Pts',(0.820802266909534,-5.1854065320192,4.6614766362689));
#31379=CARTESIAN_POINT('Ctrl Pts',(0.824829125417023,-5.18479435673255,
4.66144660123003));
#31380=CARTESIAN_POINT('Ctrl Pts',(0.833861416620451,-5.18364643340307,
4.66111486035927));
#31381=CARTESIAN_POINT('Ctrl Pts',(0.838862660713588,-5.18316398093936,
4.6607514048391));
#31382=CARTESIAN_POINT('Ctrl Pts',(0.85339110867596,-5.18220152101598,4.65917598249656));
#31383=CARTESIAN_POINT('Ctrl Pts',(0.862852430991196,-5.18212349635793,
4.65750148702093));
#31384=CARTESIAN_POINT('Ctrl Pts',(0.895565354310455,-5.18366859654418,
4.64948528566701));
#31385=CARTESIAN_POINT('Ctrl Pts',(0.917446667518246,-5.18798907973249,
4.64009844156317));
#31386=CARTESIAN_POINT('Ctrl Pts',(0.957639161837223,-5.2009886698715,4.61539308723158));
#31387=CARTESIAN_POINT('Ctrl Pts',(0.975468409628028,-5.20960735062881,
4.60019195379196));
#31388=CARTESIAN_POINT('Ctrl Pts',(1.01135000762511,-5.23157713192079,4.56080656181527));
#31389=CARTESIAN_POINT('Ctrl Pts',(1.02764742893491,-5.24551512024199,4.53533737515854));
#31390=CARTESIAN_POINT('Ctrl Pts',(1.05958947114721,-5.27879652641763,4.46952174021344));
#31391=CARTESIAN_POINT('Ctrl Pts',(1.07332334134435,-5.29952052947749,4.42457618200306));
#31392=CARTESIAN_POINT('Ctrl Pts',(1.1024338839854,-5.35665054316767,4.27073174534985));
#31393=CARTESIAN_POINT('Ctrl Pts',(1.10635903124558,-5.38757549311203,4.1440732441299));
#31394=CARTESIAN_POINT('Ctrl Pts',(1.10635903124558,-5.38757549311203,4.));
#31395=CARTESIAN_POINT('',(0.612642419821478,-5.46577252229136,0.));
#31396=CARTESIAN_POINT('',(0.612642419821478,-5.46577252229136,0.));
#31397=CARTESIAN_POINT('',(1.1063590312456,-5.38757549311203,0.));
#31398=CARTESIAN_POINT('Origin',(0.86038955772127,-5.43228587327326,0.));
#31399=CARTESIAN_POINT('',(1.1063590312456,-5.38757549311203,0.));
#31400=CARTESIAN_POINT('Origin',(0.,0.,0.));
#31401=CARTESIAN_POINT('Origin',(0.,0.,0.));
#31402=CARTESIAN_POINT('Origin',(0.,0.,0.));
#31403=CARTESIAN_POINT('Origin',(0.,0.,0.));
#31404=CARTESIAN_POINT('Origin',(0.,0.,0.));
#31405=CARTESIAN_POINT('Origin',(0.,0.,0.));
#31406=CARTESIAN_POINT('Origin',(0.,0.,0.));
#31407=CARTESIAN_POINT('Origin',(0.,0.,0.));
#31408=CARTESIAN_POINT('Origin',(0.,0.,0.));
#31409=CARTESIAN_POINT('Origin',(0.,0.,0.));
#31410=CARTESIAN_POINT('Origin',(0.,0.,0.));
#31411=CARTESIAN_POINT('Origin',(0.,0.,0.));
#31412=CARTESIAN_POINT('Origin',(0.,0.,0.));
#31413=CARTESIAN_POINT('Origin',(0.,0.,0.));
#31414=CARTESIAN_POINT('Origin',(0.,0.,0.));
#31415=CARTESIAN_POINT('Origin',(0.,0.,0.));
#31416=CARTESIAN_POINT('Origin',(0.,0.,0.));
#31417=CARTESIAN_POINT('Origin',(0.,0.,0.));
#31418=CARTESIAN_POINT('Origin',(0.,0.,0.));
#31419=CARTESIAN_POINT('Origin',(0.,0.,0.));
#31420=CARTESIAN_POINT('Origin',(0.,0.,0.));
#31421=CARTESIAN_POINT('Origin',(0.,0.,0.));
#31422=CARTESIAN_POINT('Origin',(0.,0.,0.));
#31423=CARTESIAN_POINT('Origin',(0.,0.,0.));
#31424=CARTESIAN_POINT('Origin',(0.,0.,0.));
#31425=CARTESIAN_POINT('Origin',(0.,0.,0.));
#31426=CARTESIAN_POINT('Origin',(0.,0.,0.));
#31427=CARTESIAN_POINT('Origin',(0.,0.,0.));
#31428=CARTESIAN_POINT('Origin',(0.,0.,0.));
#31429=CARTESIAN_POINT('Origin',(0.,0.,0.));
#31430=CARTESIAN_POINT('Origin',(0.,0.,0.));
#31431=CARTESIAN_POINT('Origin',(0.,0.,0.));
#31432=CARTESIAN_POINT('Origin',(0.,0.,0.));
#31433=CARTESIAN_POINT('Origin',(0.,0.,0.));
#31434=CARTESIAN_POINT('Origin',(0.,0.,0.));
#31435=CARTESIAN_POINT('Origin',(0.,0.,0.));
#31436=CARTESIAN_POINT('Origin',(0.,0.,0.));
#31437=CARTESIAN_POINT('Origin',(0.,0.,0.));
#31438=CARTESIAN_POINT('Origin',(0.,0.,0.));
#31439=CARTESIAN_POINT('',(0.249935425544577,-5.49431818181818,0.));
#31440=CARTESIAN_POINT('Origin',(0.,0.,0.));
#31441=CARTESIAN_POINT('',(-0.249935425544577,-5.49431818181818,0.));
#31442=CARTESIAN_POINT('Origin',(0.,-5.5,0.));
#31443=CARTESIAN_POINT('Origin',(0.,0.,0.));
#31444=CARTESIAN_POINT('Origin',(0.,0.,0.));
#31445=CARTESIAN_POINT('',(0.249935425544577,-5.49431818181818,4.));
#31446=CARTESIAN_POINT('Origin',(0.,0.,4.));
#31447=CARTESIAN_POINT('',(0.249935425544577,-5.49431818181818,0.));
#31448=CARTESIAN_POINT('Origin',(0.,0.,0.));
#31449=CARTESIAN_POINT('Origin',(0.,0.,4.));
#31450=CARTESIAN_POINT('Origin',(0.,0.,0.));
#31451=CARTESIAN_POINT('Origin',(0.,0.,4.));
#31452=CARTESIAN_POINT('Origin',(0.,0.,0.));
#31453=CARTESIAN_POINT('Origin',(0.,0.,4.));
#31454=CARTESIAN_POINT('Origin',(0.,0.,0.));
#31455=CARTESIAN_POINT('Origin',(0.,0.,4.));
#31456=CARTESIAN_POINT('Origin',(0.,0.,0.));
#31457=CARTESIAN_POINT('Origin',(0.,0.,4.));
#31458=CARTESIAN_POINT('Origin',(0.,0.,0.));
#31459=CARTESIAN_POINT('Origin',(0.,0.,4.));
#31460=CARTESIAN_POINT('Origin',(0.,0.,0.));
#31461=CARTESIAN_POINT('Origin',(0.,0.,4.));
#31462=CARTESIAN_POINT('Origin',(0.,0.,0.));
#31463=CARTESIAN_POINT('Origin',(0.,0.,4.));
#31464=CARTESIAN_POINT('Origin',(0.,0.,0.));
#31465=CARTESIAN_POINT('Origin',(0.,0.,4.));
#31466=CARTESIAN_POINT('Origin',(0.,0.,0.));
#31467=CARTESIAN_POINT('Origin',(0.,0.,4.));
#31468=CARTESIAN_POINT('Origin',(0.,0.,0.));
#31469=CARTESIAN_POINT('Origin',(0.,0.,4.));
#31470=CARTESIAN_POINT('Origin',(0.,0.,0.));
#31471=CARTESIAN_POINT('Origin',(0.,0.,4.));
#31472=CARTESIAN_POINT('Origin',(0.,0.,0.));
#31473=CARTESIAN_POINT('Origin',(0.,0.,4.));
#31474=CARTESIAN_POINT('Origin',(0.,0.,0.));
#31475=CARTESIAN_POINT('Origin',(0.,0.,4.));
#31476=CARTESIAN_POINT('Origin',(0.,0.,0.));
#31477=CARTESIAN_POINT('Origin',(0.,0.,4.));
#31478=CARTESIAN_POINT('Origin',(0.,0.,0.));
#31479=CARTESIAN_POINT('Origin',(0.,0.,4.));
#31480=CARTESIAN_POINT('Origin',(0.,0.,0.));
#31481=CARTESIAN_POINT('Origin',(0.,0.,4.));
#31482=CARTESIAN_POINT('Origin',(0.,0.,0.));
#31483=CARTESIAN_POINT('Origin',(0.,0.,4.));
#31484=CARTESIAN_POINT('Origin',(0.,0.,0.));
#31485=CARTESIAN_POINT('Origin',(0.,0.,4.));
#31486=CARTESIAN_POINT('Origin',(0.,0.,0.));
#31487=CARTESIAN_POINT('Origin',(0.,0.,4.));
#31488=CARTESIAN_POINT('Origin',(0.,0.,0.));
#31489=CARTESIAN_POINT('Origin',(0.,0.,4.));
#31490=CARTESIAN_POINT('Origin',(0.,0.,0.));
#31491=CARTESIAN_POINT('Origin',(0.,0.,4.));
#31492=CARTESIAN_POINT('Origin',(0.,0.,0.));
#31493=CARTESIAN_POINT('Origin',(0.,0.,4.));
#31494=CARTESIAN_POINT('Origin',(0.,0.,0.));
#31495=CARTESIAN_POINT('Origin',(0.,0.,4.));
#31496=CARTESIAN_POINT('Origin',(0.,0.,0.));
#31497=CARTESIAN_POINT('Origin',(0.,0.,4.));
#31498=CARTESIAN_POINT('Origin',(0.,0.,0.));
#31499=CARTESIAN_POINT('Origin',(0.,0.,4.));
#31500=CARTESIAN_POINT('Origin',(0.,0.,0.));
#31501=CARTESIAN_POINT('Origin',(0.,0.,4.));
#31502=CARTESIAN_POINT('Origin',(0.,0.,0.));
#31503=CARTESIAN_POINT('Origin',(0.,0.,4.));
#31504=CARTESIAN_POINT('Origin',(0.,0.,0.));
#31505=CARTESIAN_POINT('Origin',(0.,0.,4.));
#31506=CARTESIAN_POINT('Origin',(0.,0.,0.));
#31507=CARTESIAN_POINT('Origin',(0.,0.,4.));
#31508=CARTESIAN_POINT('Origin',(0.,0.,0.));
#31509=CARTESIAN_POINT('Origin',(0.,0.,4.));
#31510=CARTESIAN_POINT('Origin',(0.,0.,0.));
#31511=CARTESIAN_POINT('Origin',(0.,0.,4.));
#31512=CARTESIAN_POINT('Origin',(0.,0.,0.));
#31513=CARTESIAN_POINT('Origin',(0.,0.,4.));
#31514=CARTESIAN_POINT('Origin',(0.,0.,0.));
#31515=CARTESIAN_POINT('Origin',(0.,0.,4.));
#31516=CARTESIAN_POINT('Origin',(0.,0.,0.));
#31517=CARTESIAN_POINT('Origin',(0.,0.,4.));
#31518=CARTESIAN_POINT('Origin',(0.,0.,0.));
#31519=CARTESIAN_POINT('Origin',(0.,0.,4.));
#31520=CARTESIAN_POINT('Origin',(0.,0.,0.));
#31521=CARTESIAN_POINT('Origin',(0.,0.,4.));
#31522=CARTESIAN_POINT('Origin',(0.,0.,0.));
#31523=CARTESIAN_POINT('Origin',(0.,0.,4.));
#31524=CARTESIAN_POINT('Origin',(0.,0.,4.));
#31525=CARTESIAN_POINT('Origin',(-4.5,-5.51091059616309E-16,4.));
#31526=CARTESIAN_POINT('',(-0.249935425544577,-5.49431818181818,4.));
#31527=CARTESIAN_POINT('Origin',(0.,0.,4.));
#31528=CARTESIAN_POINT('Ctrl Pts',(-0.249935425544577,-5.49431818181818,
4.));
#31529=CARTESIAN_POINT('Ctrl Pts',(-0.249935425544577,-5.49431818181818,
4.02673063961773));
#31530=CARTESIAN_POINT('Ctrl Pts',(-0.249919456117148,-5.49324675169276,
4.05414638576012));
#31531=CARTESIAN_POINT('Ctrl Pts',(-0.249513006492199,-5.48204205167785,
4.19012241323843));
#31532=CARTESIAN_POINT('Ctrl Pts',(-0.24856258550615,-5.45648829138082,
4.28686359329027));
#31533=CARTESIAN_POINT('Ctrl Pts',(-0.231005155267322,-5.40161207108227,
4.42646405387428));
#31534=CARTESIAN_POINT('Ctrl Pts',(-0.219652829312575,-5.37693177978515,
4.4748270579004));
#31535=CARTESIAN_POINT('Ctrl Pts',(-0.190283636781574,-5.33662435870041,
4.54353143773204));
#31536=CARTESIAN_POINT('Ctrl Pts',(-0.175067268428665,-5.31971884723752,
4.56934838942208));
#31537=CARTESIAN_POINT('Ctrl Pts',(-0.141228917894015,-5.29295926834979,
4.6071405640229));
#31538=CARTESIAN_POINT('Ctrl Pts',(-0.125109626503179,-5.28258044284084,
4.62089194101728));
#31539=CARTESIAN_POINT('Ctrl Pts',(-0.0869023758915853,-5.26459283535906,
4.64388394673189));
#31540=CARTESIAN_POINT('Ctrl Pts',(-0.0649862317445936,-5.25739000836648,
4.65258978726599));
#31541=CARTESIAN_POINT('Ctrl Pts',(-0.0336815115207147,-5.25216283051672,
4.65886310574997));
#31542=CARTESIAN_POINT('Ctrl Pts',(-0.026067610803539,-5.25124279397843,
4.65995935047192));
#31543=CARTESIAN_POINT('Ctrl Pts',(-0.0137773685317613,-5.25033755739286,
4.661036848069));
#31544=CARTESIAN_POINT('Ctrl Pts',(-0.0091697388298722,-5.25012547438354,
4.66128876278955));
#31545=CARTESIAN_POINT('Ctrl Pts',(-0.000479467891947508,-5.24996733644903,
4.6614766362689));
#31546=CARTESIAN_POINT('Ctrl Pts',(0.00359357861859472,-5.24999263751242,
4.66144660123004));
#31547=CARTESIAN_POINT('Ctrl Pts',(0.0126942421010939,-5.25027180866649,
4.66111486035927));
#31548=CARTESIAN_POINT('Ctrl Pts',(0.0177093847734648,-5.25057766293745,
4.6607514048391));
#31549=CARTESIAN_POINT('Ctrl Pts',(0.0322095253359853,-5.25189980247768,
4.65917598249656));
#31550=CARTESIAN_POINT('Ctrl Pts',(0.0415665688189868,-5.2533028153276,
4.65750148702094));
#31551=CARTESIAN_POINT('Ctrl Pts',(0.0736350348471512,-5.25994632142597,
4.64948528566701));
#31552=CARTESIAN_POINT('Ctrl Pts',(0.0945710803031181,-5.26763660382283,
4.64009844156318));
#31553=CARTESIAN_POINT('Ctrl Pts',(0.132235154392271,-5.28676363878307,
4.61539308723159));
#31554=CARTESIAN_POINT('Ctrl Pts',(0.14849663584321,-5.2980653181186,4.60019195379196));
#31555=CARTESIAN_POINT('Ctrl Pts',(0.180499640843384,-5.32537773353357,
4.56080656181528));
#31556=CARTESIAN_POINT('Ctrl Pts',(0.194416032106083,-5.34169360047391,
4.53533737515855));
#31557=CARTESIAN_POINT('Ctrl Pts',(0.220758455803108,-5.379562093598,4.46952174021342));
#31558=CARTESIAN_POINT('Ctrl Pts',(0.231081290935903,-5.4021794004279,4.42457618200302));
#31559=CARTESIAN_POINT('Ctrl Pts',(0.250896331361498,-5.46315994101279,
4.27073174534988));
#31560=CARTESIAN_POINT('Ctrl Pts',(0.249935425544557,-5.49431818181818,
4.14407324412993));
#31561=CARTESIAN_POINT('Ctrl Pts',(0.249935425544557,-5.49431818181818,
4.));
#31562=CARTESIAN_POINT('Origin',(0.,-5.5,0.));
#31563=CARTESIAN_POINT('',(-0.249935425544577,-5.49431818181818,0.));
#31564=CARTESIAN_POINT('Origin',(0.,0.,0.));
#31565=CARTESIAN_POINT('Origin',(0.,0.,5.));
#31566=CARTESIAN_POINT('Origin',(0.,0.,35.));
#31567=CARTESIAN_POINT('',(0.,0.,0.));
#31568=CARTESIAN_POINT('Origin',(0.,0.,25.1187110682415));
#31569=CARTESIAN_POINT('',(-17.0820002071033,-2.09194168766635E-15,25.8287284513987));
#31570=CARTESIAN_POINT('Origin',(0.,-2.09194168766635E-15,25.8287284513987));
#31571=CARTESIAN_POINT('',(-14.8491923750145,-1.81850159119848E-15,24.2652995759965));
#31572=CARTESIAN_POINT('',(-16.067990296595,-1.96776128854558E-15,25.1187110682415));
#31573=CARTESIAN_POINT('Origin',(0.,0.,24.2652995759965));
#31574=CARTESIAN_POINT('Origin',(0.,0.,26.033516462471));
#31575=CARTESIAN_POINT('',(-16.7952119889278,-2.05682026032416E-15,26.2383044735432));
#31576=CARTESIAN_POINT('Origin',(0.,-2.05682026032416E-15,26.2383044735432));
#31577=CARTESIAN_POINT('Origin',(-16.9386060980155,-2.07438097399525E-15,
26.033516462471));
#31578=CARTESIAN_POINT('Origin',(0.,0.,25.5213339281044));
#31579=CARTESIAN_POINT('',(-14.542543867133,-1.78094797983444E-15,24.6609692735778));
#31580=CARTESIAN_POINT('Origin',(0.,0.,24.6609692735778));
#31581=CARTESIAN_POINT('',(-15.7712719335665,-1.93142376919247E-15,25.5213339281044));
#31582=CARTESIAN_POINT('Origin',(0.,0.,25.9634052319394));
#31583=CARTESIAN_POINT('',(12.2837868382051,0.,24.6609692735778));
#31584=CARTESIAN_POINT('',(-12.2837868382051,-1.50433002328163E-15,24.6609692735778));
#31585=CARTESIAN_POINT('Origin',(0.,0.,24.6609692735778));
#31586=CARTESIAN_POINT('Origin',(0.,0.,24.6609692735778));
#31587=CARTESIAN_POINT('Origin',(-13.4131653526691,-1.64263900155804E-15,
25.9634052319394));
#31588=CARTESIAN_POINT('Ctrl Pts',(0.999999999999995,0.,26.6733182859787));
#31589=CARTESIAN_POINT('Ctrl Pts',(0.999999999999995,0.999999999999995,
26.6733182859787));
#31590=CARTESIAN_POINT('Ctrl Pts',(0.,0.999999999999995,26.6733182859787));
#31591=CARTESIAN_POINT('Ctrl Pts',(-0.999999999999995,0.999999999999995,
26.6733182859787));
#31592=CARTESIAN_POINT('Ctrl Pts',(-0.999999999999995,0.,26.6733182859787));
#31593=CARTESIAN_POINT('Ctrl Pts',(-0.999999999999995,-0.999999999999995,
26.6733182859787));
#31594=CARTESIAN_POINT('Ctrl Pts',(0.,-0.999999999999995,26.6733182859787));
#31595=CARTESIAN_POINT('Ctrl Pts',(0.999999999999995,-0.999999999999995,
26.6733182859787));
#31596=CARTESIAN_POINT('Ctrl Pts',(0.999999999999995,0.,26.6733182859787));
#31597=CARTESIAN_POINT('Ctrl Pts',(1.5,0.,26.6149943453092));
#31598=CARTESIAN_POINT('Ctrl Pts',(1.5,1.5,26.6149943453092));
#31599=CARTESIAN_POINT('Ctrl Pts',(0.,1.5,26.6149943453092));
#31600=CARTESIAN_POINT('Ctrl Pts',(-1.5,1.5,26.6149943453092));
#31601=CARTESIAN_POINT('Ctrl Pts',(-1.5,0.,26.6149943453092));
#31602=CARTESIAN_POINT('Ctrl Pts',(-1.5,-1.5,26.6149943453092));
#31603=CARTESIAN_POINT('Ctrl Pts',(0.,-1.5,26.6149943453092));
#31604=CARTESIAN_POINT('Ctrl Pts',(1.5,-1.5,26.6149943453092));
#31605=CARTESIAN_POINT('Ctrl Pts',(1.5,0.,26.6149943453092));
#31606=CARTESIAN_POINT('Ctrl Pts',(2.,0.,26.5566704046396));
#31607=CARTESIAN_POINT('Ctrl Pts',(2.,2.,26.5566704046396));
#31608=CARTESIAN_POINT('Ctrl Pts',(0.,2.,26.5566704046396));
#31609=CARTESIAN_POINT('Ctrl Pts',(-2.,2.,26.5566704046396));
#31610=CARTESIAN_POINT('Ctrl Pts',(-2.,0.,26.5566704046396));
#31611=CARTESIAN_POINT('Ctrl Pts',(-2.,-2.,26.5566704046396));
#31612=CARTESIAN_POINT('Ctrl Pts',(0.,-2.,26.5566704046396));
#31613=CARTESIAN_POINT('Ctrl Pts',(2.,-2.,26.5566704046396));
#31614=CARTESIAN_POINT('Ctrl Pts',(2.,0.,26.5566704046396));
#31615=CARTESIAN_POINT('Ctrl Pts',(2.5,0.,26.4983464639701));
#31616=CARTESIAN_POINT('Ctrl Pts',(2.5,2.5,26.4983464639701));
#31617=CARTESIAN_POINT('Ctrl Pts',(0.,2.5,26.4983464639701));
#31618=CARTESIAN_POINT('Ctrl Pts',(-2.5,2.5,26.4983464639701));
#31619=CARTESIAN_POINT('Ctrl Pts',(-2.5,0.,26.4983464639701));
#31620=CARTESIAN_POINT('Ctrl Pts',(-2.5,-2.5,26.4983464639701));
#31621=CARTESIAN_POINT('Ctrl Pts',(0.,-2.5,26.4983464639701));
#31622=CARTESIAN_POINT('Ctrl Pts',(2.5,-2.5,26.4983464639701));
#31623=CARTESIAN_POINT('Ctrl Pts',(2.5,0.,26.4983464639701));
#31624=CARTESIAN_POINT('Ctrl Pts',(3.,0.,26.4400225233005));
#31625=CARTESIAN_POINT('Ctrl Pts',(3.,3.,26.4400225233005));
#31626=CARTESIAN_POINT('Ctrl Pts',(0.,3.,26.4400225233005));
#31627=CARTESIAN_POINT('Ctrl Pts',(-3.,3.,26.4400225233005));
#31628=CARTESIAN_POINT('Ctrl Pts',(-3.,0.,26.4400225233005));
#31629=CARTESIAN_POINT('Ctrl Pts',(-3.,-3.,26.4400225233005));
#31630=CARTESIAN_POINT('Ctrl Pts',(0.,-3.,26.4400225233005));
#31631=CARTESIAN_POINT('Ctrl Pts',(3.,-3.,26.4400225233005));
#31632=CARTESIAN_POINT('Ctrl Pts',(3.,0.,26.4400225233005));
#31633=CARTESIAN_POINT('Ctrl Pts',(3.5,0.,26.381698582631));
#31634=CARTESIAN_POINT('Ctrl Pts',(3.5,3.5,26.381698582631));
#31635=CARTESIAN_POINT('Ctrl Pts',(0.,3.5,26.381698582631));
#31636=CARTESIAN_POINT('Ctrl Pts',(-3.5,3.5,26.381698582631));
#31637=CARTESIAN_POINT('Ctrl Pts',(-3.5,0.,26.381698582631));
#31638=CARTESIAN_POINT('Ctrl Pts',(-3.5,-3.5,26.381698582631));
#31639=CARTESIAN_POINT('Ctrl Pts',(0.,-3.5,26.381698582631));
#31640=CARTESIAN_POINT('Ctrl Pts',(3.5,-3.5,26.381698582631));
#31641=CARTESIAN_POINT('Ctrl Pts',(3.5,0.,26.381698582631));
#31642=CARTESIAN_POINT('Ctrl Pts',(3.61098900507559,0.,26.368751950337));
#31643=CARTESIAN_POINT('Ctrl Pts',(3.61098900507559,3.61098900507559,26.368751950337));
#31644=CARTESIAN_POINT('Ctrl Pts',(0.,3.61098900507559,26.368751950337));
#31645=CARTESIAN_POINT('Ctrl Pts',(-3.61098900507559,3.61098900507559,26.368751950337));
#31646=CARTESIAN_POINT('Ctrl Pts',(-3.61098900507559,0.,26.368751950337));
#31647=CARTESIAN_POINT('Ctrl Pts',(-3.61098900507559,-3.61098900507559,
26.368751950337));
#31648=CARTESIAN_POINT('Ctrl Pts',(0.,-3.61098900507559,26.368751950337));
#31649=CARTESIAN_POINT('Ctrl Pts',(3.61098900507559,-3.61098900507559,26.368751950337));
#31650=CARTESIAN_POINT('Ctrl Pts',(3.61098900507559,0.,26.368751950337));
#31651=CARTESIAN_POINT('Ctrl Pts',(3.83416205501541,0.,26.3417018678852));
#31652=CARTESIAN_POINT('Ctrl Pts',(3.83416205501541,3.83416205501541,26.3417018678852));
#31653=CARTESIAN_POINT('Ctrl Pts',(0.,3.83416205501541,26.3417018678852));
#31654=CARTESIAN_POINT('Ctrl Pts',(-3.83416205501541,3.83416205501541,26.3417018678852));
#31655=CARTESIAN_POINT('Ctrl Pts',(-3.83416205501541,0.,26.3417018678852));
#31656=CARTESIAN_POINT('Ctrl Pts',(-3.83416205501541,-3.83416205501541,
26.3417018678852));
#31657=CARTESIAN_POINT('Ctrl Pts',(0.,-3.83416205501541,26.3417018678852));
#31658=CARTESIAN_POINT('Ctrl Pts',(3.83416205501541,-3.83416205501541,26.3417018678852));
#31659=CARTESIAN_POINT('Ctrl Pts',(3.83416205501541,0.,26.3417018678852));
#31660=CARTESIAN_POINT('Ctrl Pts',(4.17250673641263,0.,26.2976563050266));
#31661=CARTESIAN_POINT('Ctrl Pts',(4.17250673641263,4.17250673641263,26.2976563050266));
#31662=CARTESIAN_POINT('Ctrl Pts',(0.,4.17250673641263,26.2976563050266));
#31663=CARTESIAN_POINT('Ctrl Pts',(-4.17250673641263,4.17250673641263,26.2976563050266));
#31664=CARTESIAN_POINT('Ctrl Pts',(-4.17250673641263,0.,26.2976563050266));
#31665=CARTESIAN_POINT('Ctrl Pts',(-4.17250673641263,-4.17250673641263,
26.2976563050266));
#31666=CARTESIAN_POINT('Ctrl Pts',(0.,-4.17250673641263,26.2976563050266));
#31667=CARTESIAN_POINT('Ctrl Pts',(4.17250673641263,-4.17250673641263,26.2976563050266));
#31668=CARTESIAN_POINT('Ctrl Pts',(4.17250673641263,0.,26.2976563050266));
#31669=CARTESIAN_POINT('Ctrl Pts',(4.63085543889697,0.,26.2319374216757));
#31670=CARTESIAN_POINT('Ctrl Pts',(4.63085543889697,4.63085543889697,26.2319374216757));
#31671=CARTESIAN_POINT('Ctrl Pts',(0.,4.63085543889697,26.2319374216757));
#31672=CARTESIAN_POINT('Ctrl Pts',(-4.63085543889697,4.63085543889697,26.2319374216757));
#31673=CARTESIAN_POINT('Ctrl Pts',(-4.63085543889697,0.,26.2319374216757));
#31674=CARTESIAN_POINT('Ctrl Pts',(-4.63085543889697,-4.63085543889697,
26.2319374216757));
#31675=CARTESIAN_POINT('Ctrl Pts',(0.,-4.63085543889697,26.2319374216757));
#31676=CARTESIAN_POINT('Ctrl Pts',(4.63085543889697,-4.63085543889697,26.2319374216757));
#31677=CARTESIAN_POINT('Ctrl Pts',(4.63085543889697,0.,26.2319374216757));
#31678=CARTESIAN_POINT('Ctrl Pts',(5.21591518523417,0.,26.137974806988));
#31679=CARTESIAN_POINT('Ctrl Pts',(5.21591518523417,5.21591518523417,26.137974806988));
#31680=CARTESIAN_POINT('Ctrl Pts',(0.,5.21591518523417,26.137974806988));
#31681=CARTESIAN_POINT('Ctrl Pts',(-5.21591518523417,5.21591518523417,26.137974806988));
#31682=CARTESIAN_POINT('Ctrl Pts',(-5.21591518523417,0.,26.137974806988));
#31683=CARTESIAN_POINT('Ctrl Pts',(-5.21591518523417,-5.21591518523417,
26.137974806988));
#31684=CARTESIAN_POINT('Ctrl Pts',(0.,-5.21591518523417,26.137974806988));
#31685=CARTESIAN_POINT('Ctrl Pts',(5.21591518523417,-5.21591518523417,26.137974806988));
#31686=CARTESIAN_POINT('Ctrl Pts',(5.21591518523417,0.,26.137974806988));
#31687=CARTESIAN_POINT('Ctrl Pts',(5.81280340273043,0.,26.0322484636216));
#31688=CARTESIAN_POINT('Ctrl Pts',(5.81280340273043,5.81280340273043,26.0322484636216));
#31689=CARTESIAN_POINT('Ctrl Pts',(0.,5.81280340273043,26.0322484636216));
#31690=CARTESIAN_POINT('Ctrl Pts',(-5.81280340273043,5.81280340273043,26.0322484636216));
#31691=CARTESIAN_POINT('Ctrl Pts',(-5.81280340273043,0.,26.0322484636216));
#31692=CARTESIAN_POINT('Ctrl Pts',(-5.81280340273043,-5.81280340273043,
26.0322484636216));
#31693=CARTESIAN_POINT('Ctrl Pts',(0.,-5.81280340273043,26.0322484636216));
#31694=CARTESIAN_POINT('Ctrl Pts',(5.81280340273043,-5.81280340273043,26.0322484636216));
#31695=CARTESIAN_POINT('Ctrl Pts',(5.81280340273043,0.,26.0322484636216));
#31696=CARTESIAN_POINT('Ctrl Pts',(6.42047090449388,0.,25.9152983846727));
#31697=CARTESIAN_POINT('Ctrl Pts',(6.42047090449387,6.42047090449387,25.9152983846727));
#31698=CARTESIAN_POINT('Ctrl Pts',(0.,6.42047090449388,25.9152983846727));
#31699=CARTESIAN_POINT('Ctrl Pts',(-6.42047090449387,6.42047090449387,25.9152983846727));
#31700=CARTESIAN_POINT('Ctrl Pts',(-6.42047090449388,0.,25.9152983846727));
#31701=CARTESIAN_POINT('Ctrl Pts',(-6.42047090449387,-6.42047090449387,
25.9152983846727));
#31702=CARTESIAN_POINT('Ctrl Pts',(0.,-6.42047090449388,25.9152983846727));
#31703=CARTESIAN_POINT('Ctrl Pts',(6.42047090449387,-6.42047090449387,25.9152983846727));
#31704=CARTESIAN_POINT('Ctrl Pts',(6.42047090449388,0.,25.9152983846727));
#31705=CARTESIAN_POINT('Ctrl Pts',(7.0366882084607,0.,25.7884785969494));
#31706=CARTESIAN_POINT('Ctrl Pts',(7.0366882084607,7.0366882084607,25.7884785969494));
#31707=CARTESIAN_POINT('Ctrl Pts',(0.,7.0366882084607,25.7884785969494));
#31708=CARTESIAN_POINT('Ctrl Pts',(-7.0366882084607,7.0366882084607,25.7884785969494));
#31709=CARTESIAN_POINT('Ctrl Pts',(-7.0366882084607,0.,25.7884785969494));
#31710=CARTESIAN_POINT('Ctrl Pts',(-7.0366882084607,-7.0366882084607,25.7884785969494));
#31711=CARTESIAN_POINT('Ctrl Pts',(0.,-7.0366882084607,25.7884785969494));
#31712=CARTESIAN_POINT('Ctrl Pts',(7.0366882084607,-7.0366882084607,25.7884785969494));
#31713=CARTESIAN_POINT('Ctrl Pts',(7.0366882084607,0.,25.7884785969494));
#31714=CARTESIAN_POINT('Ctrl Pts',(7.65759263692165,0.,25.6543075008141));
#31715=CARTESIAN_POINT('Ctrl Pts',(7.65759263692165,7.65759263692165,25.6543075008141));
#31716=CARTESIAN_POINT('Ctrl Pts',(0.,7.65759263692165,25.6543075008141));
#31717=CARTESIAN_POINT('Ctrl Pts',(-7.65759263692165,7.65759263692165,25.6543075008141));
#31718=CARTESIAN_POINT('Ctrl Pts',(-7.65759263692165,0.,25.6543075008141));
#31719=CARTESIAN_POINT('Ctrl Pts',(-7.65759263692165,-7.65759263692165,
25.6543075008141));
#31720=CARTESIAN_POINT('Ctrl Pts',(0.,-7.65759263692165,25.6543075008141));
#31721=CARTESIAN_POINT('Ctrl Pts',(7.65759263692165,-7.65759263692165,25.6543075008141));
#31722=CARTESIAN_POINT('Ctrl Pts',(7.65759263692165,0.,25.6543075008141));
#31723=CARTESIAN_POINT('Ctrl Pts',(8.27837257578008,0.,25.5159837042088));
#31724=CARTESIAN_POINT('Ctrl Pts',(8.27837257578008,8.27837257578008,25.5159837042088));
#31725=CARTESIAN_POINT('Ctrl Pts',(0.,8.27837257578008,25.5159837042088));
#31726=CARTESIAN_POINT('Ctrl Pts',(-8.27837257578008,8.27837257578008,25.5159837042088));
#31727=CARTESIAN_POINT('Ctrl Pts',(-8.27837257578008,0.,25.5159837042088));
#31728=CARTESIAN_POINT('Ctrl Pts',(-8.27837257578008,-8.27837257578008,
25.5159837042088));
#31729=CARTESIAN_POINT('Ctrl Pts',(0.,-8.27837257578008,25.5159837042088));
#31730=CARTESIAN_POINT('Ctrl Pts',(8.27837257578008,-8.27837257578008,25.5159837042088));
#31731=CARTESIAN_POINT('Ctrl Pts',(8.27837257578008,0.,25.5159837042088));
#31732=CARTESIAN_POINT('Ctrl Pts',(8.89388282563607,0.,25.3769606320571));
#31733=CARTESIAN_POINT('Ctrl Pts',(8.89388282563607,8.89388282563607,25.3769606320571));
#31734=CARTESIAN_POINT('Ctrl Pts',(0.,8.89388282563607,25.3769606320571));
#31735=CARTESIAN_POINT('Ctrl Pts',(-8.89388282563607,8.89388282563607,25.3769606320571));
#31736=CARTESIAN_POINT('Ctrl Pts',(-8.89388282563607,0.,25.3769606320571));
#31737=CARTESIAN_POINT('Ctrl Pts',(-8.89388282563607,-8.89388282563607,
25.3769606320571));
#31738=CARTESIAN_POINT('Ctrl Pts',(0.,-8.89388282563607,25.3769606320571));
#31739=CARTESIAN_POINT('Ctrl Pts',(8.89388282563607,-8.89388282563607,25.3769606320571));
#31740=CARTESIAN_POINT('Ctrl Pts',(8.89388282563607,0.,25.3769606320571));
#31741=CARTESIAN_POINT('Ctrl Pts',(9.49928764562852,0.,25.2405145197409));
#31742=CARTESIAN_POINT('Ctrl Pts',(9.49928764562851,9.49928764562851,25.2405145197409));
#31743=CARTESIAN_POINT('Ctrl Pts',(0.,9.49928764562852,25.2405145197409));
#31744=CARTESIAN_POINT('Ctrl Pts',(-9.49928764562851,9.49928764562851,25.2405145197409));
#31745=CARTESIAN_POINT('Ctrl Pts',(-9.49928764562852,0.,25.2405145197409));
#31746=CARTESIAN_POINT('Ctrl Pts',(-9.49928764562851,-9.49928764562851,
25.2405145197409));
#31747=CARTESIAN_POINT('Ctrl Pts',(0.,-9.49928764562852,25.2405145197409));
#31748=CARTESIAN_POINT('Ctrl Pts',(9.49928764562851,-9.49928764562851,25.2405145197409));
#31749=CARTESIAN_POINT('Ctrl Pts',(9.49928764562852,0.,25.2405145197409));
#31750=CARTESIAN_POINT('Ctrl Pts',(10.0906614723548,0.,25.1093486541428));
#31751=CARTESIAN_POINT('Ctrl Pts',(10.0906614723548,10.0906614723548,25.1093486541428));
#31752=CARTESIAN_POINT('Ctrl Pts',(0.,10.0906614723548,25.1093486541428));
#31753=CARTESIAN_POINT('Ctrl Pts',(-10.0906614723548,10.0906614723548,25.1093486541428));
#31754=CARTESIAN_POINT('Ctrl Pts',(-10.0906614723548,0.,25.1093486541428));
#31755=CARTESIAN_POINT('Ctrl Pts',(-10.0906614723548,-10.0906614723548,
25.1093486541428));
#31756=CARTESIAN_POINT('Ctrl Pts',(0.,-10.0906614723548,25.1093486541428));
#31757=CARTESIAN_POINT('Ctrl Pts',(10.0906614723548,-10.0906614723548,25.1093486541428));
#31758=CARTESIAN_POINT('Ctrl Pts',(10.0906614723548,0.,25.1093486541428));
#31759=CARTESIAN_POINT('Ctrl Pts',(10.6657852303826,0.,24.9850866914374));
#31760=CARTESIAN_POINT('Ctrl Pts',(10.6657852303826,10.6657852303826,24.9850866914374));
#31761=CARTESIAN_POINT('Ctrl Pts',(0.,10.6657852303826,24.9850866914374));
#31762=CARTESIAN_POINT('Ctrl Pts',(-10.6657852303826,10.6657852303826,24.9850866914374));
#31763=CARTESIAN_POINT('Ctrl Pts',(-10.6657852303826,0.,24.9850866914374));
#31764=CARTESIAN_POINT('Ctrl Pts',(-10.6657852303826,-10.6657852303826,
24.9850866914374));
#31765=CARTESIAN_POINT('Ctrl Pts',(0.,-10.6657852303826,24.9850866914374));
#31766=CARTESIAN_POINT('Ctrl Pts',(10.6657852303826,-10.6657852303826,24.9850866914374));
#31767=CARTESIAN_POINT('Ctrl Pts',(10.6657852303826,0.,24.9850866914374));
#31768=CARTESIAN_POINT('Ctrl Pts',(11.2237519652345,0.,24.8684985935572));
#31769=CARTESIAN_POINT('Ctrl Pts',(11.2237519652345,11.2237519652345,24.8684985935572));
#31770=CARTESIAN_POINT('Ctrl Pts',(0.,11.2237519652345,24.8684985935572));
#31771=CARTESIAN_POINT('Ctrl Pts',(-11.2237519652345,11.2237519652345,24.8684985935572));
#31772=CARTESIAN_POINT('Ctrl Pts',(-11.2237519652345,0.,24.8684985935572));
#31773=CARTESIAN_POINT('Ctrl Pts',(-11.2237519652345,-11.2237519652345,
24.8684985935572));
#31774=CARTESIAN_POINT('Ctrl Pts',(0.,-11.2237519652345,24.8684985935572));
#31775=CARTESIAN_POINT('Ctrl Pts',(11.2237519652345,-11.2237519652345,24.8684985935572));
#31776=CARTESIAN_POINT('Ctrl Pts',(11.2237519652345,0.,24.8684985935572));
#31777=CARTESIAN_POINT('Ctrl Pts',(11.6562879503402,0.,24.7815592956469));
#31778=CARTESIAN_POINT('Ctrl Pts',(11.6562879503402,11.6562879503402,24.7815592956469));
#31779=CARTESIAN_POINT('Ctrl Pts',(0.,11.6562879503402,24.7815592956469));
#31780=CARTESIAN_POINT('Ctrl Pts',(-11.6562879503402,11.6562879503402,24.7815592956469));
#31781=CARTESIAN_POINT('Ctrl Pts',(-11.6562879503402,0.,24.7815592956469));
#31782=CARTESIAN_POINT('Ctrl Pts',(-11.6562879503402,-11.6562879503402,
24.7815592956469));
#31783=CARTESIAN_POINT('Ctrl Pts',(0.,-11.6562879503402,24.7815592956469));
#31784=CARTESIAN_POINT('Ctrl Pts',(11.6562879503402,-11.6562879503402,24.7815592956469));
#31785=CARTESIAN_POINT('Ctrl Pts',(11.6562879503402,0.,24.7815592956469));
#31786=CARTESIAN_POINT('Ctrl Pts',(11.97300464761,0.,24.7198967418176));
#31787=CARTESIAN_POINT('Ctrl Pts',(11.97300464761,11.97300464761,24.7198967418176));
#31788=CARTESIAN_POINT('Ctrl Pts',(0.,11.97300464761,24.7198967418176));
#31789=CARTESIAN_POINT('Ctrl Pts',(-11.97300464761,11.97300464761,24.7198967418176));
#31790=CARTESIAN_POINT('Ctrl Pts',(-11.97300464761,0.,24.7198967418176));
#31791=CARTESIAN_POINT('Ctrl Pts',(-11.97300464761,-11.97300464761,24.7198967418176));
#31792=CARTESIAN_POINT('Ctrl Pts',(0.,-11.97300464761,24.7198967418176));
#31793=CARTESIAN_POINT('Ctrl Pts',(11.97300464761,-11.97300464761,24.7198967418176));
#31794=CARTESIAN_POINT('Ctrl Pts',(11.97300464761,0.,24.7198967418176));
#31795=CARTESIAN_POINT('Ctrl Pts',(12.1807579618051,0.,24.6803512815114));
#31796=CARTESIAN_POINT('Ctrl Pts',(12.1807579618051,12.1807579618051,24.6803512815114));
#31797=CARTESIAN_POINT('Ctrl Pts',(0.,12.1807579618051,24.6803512815114));
#31798=CARTESIAN_POINT('Ctrl Pts',(-12.1807579618051,12.1807579618051,24.6803512815114));
#31799=CARTESIAN_POINT('Ctrl Pts',(-12.1807579618051,0.,24.6803512815114));
#31800=CARTESIAN_POINT('Ctrl Pts',(-12.1807579618051,-12.1807579618051,
24.6803512815114));
#31801=CARTESIAN_POINT('Ctrl Pts',(0.,-12.1807579618051,24.6803512815114));
#31802=CARTESIAN_POINT('Ctrl Pts',(12.1807579618051,-12.1807579618051,24.6803512815114));
#31803=CARTESIAN_POINT('Ctrl Pts',(12.1807579618051,0.,24.6803512815114));
#31804=CARTESIAN_POINT('Ctrl Pts',(12.2837868382051,0.,24.6609692735778));
#31805=CARTESIAN_POINT('Ctrl Pts',(12.2837868382051,12.2837868382051,24.6609692735778));
#31806=CARTESIAN_POINT('Ctrl Pts',(0.,12.2837868382051,24.6609692735778));
#31807=CARTESIAN_POINT('Ctrl Pts',(-12.2837868382051,12.2837868382051,24.6609692735778));
#31808=CARTESIAN_POINT('Ctrl Pts',(-12.2837868382051,0.,24.6609692735778));
#31809=CARTESIAN_POINT('Ctrl Pts',(-12.2837868382051,-12.2837868382051,
24.6609692735778));
#31810=CARTESIAN_POINT('Ctrl Pts',(0.,-12.2837868382051,24.6609692735778));
#31811=CARTESIAN_POINT('Ctrl Pts',(12.2837868382051,-12.2837868382051,24.6609692735778));
#31812=CARTESIAN_POINT('Ctrl Pts',(12.2837868382051,0.,24.6609692735778));
#31813=CARTESIAN_POINT('',(2.5,0.,26.4983464639701));
#31814=CARTESIAN_POINT('Ctrl Pts',(2.5,0.,26.4983464639701));
#31815=CARTESIAN_POINT('Ctrl Pts',(2.7,0.,26.4750168877023));
#31816=CARTESIAN_POINT('Ctrl Pts',(2.9,0.,26.4516873114344));
#31817=CARTESIAN_POINT('Ctrl Pts',(3.1,0.,26.4283577351666));
#31818=CARTESIAN_POINT('Ctrl Pts',(3.3,0.,26.4050281588988));
#31819=CARTESIAN_POINT('Ctrl Pts',(3.5,0.,26.381698582631));
#31820=CARTESIAN_POINT('Ctrl Pts',(3.61098900507559,0.,26.368751950337));
#31821=CARTESIAN_POINT('Ctrl Pts',(3.83416205501541,0.,26.3417018678852));
#31822=CARTESIAN_POINT('Ctrl Pts',(4.17250673641263,0.,26.2976563050266));
#31823=CARTESIAN_POINT('Ctrl Pts',(4.63085543889697,0.,26.2319374216757));
#31824=CARTESIAN_POINT('Ctrl Pts',(5.21591518523417,0.,26.137974806988));
#31825=CARTESIAN_POINT('Ctrl Pts',(5.81280340273043,0.,26.0322484636216));
#31826=CARTESIAN_POINT('Ctrl Pts',(6.42047090449388,0.,25.9152983846727));
#31827=CARTESIAN_POINT('Ctrl Pts',(7.0366882084607,0.,25.7884785969494));
#31828=CARTESIAN_POINT('Ctrl Pts',(7.65759263692165,0.,25.6543075008141));
#31829=CARTESIAN_POINT('Ctrl Pts',(8.27837257578008,0.,25.5159837042088));
#31830=CARTESIAN_POINT('Ctrl Pts',(8.89388282563607,0.,25.3769606320571));
#31831=CARTESIAN_POINT('Ctrl Pts',(9.49928764562852,0.,25.2405145197409));
#31832=CARTESIAN_POINT('Ctrl Pts',(10.0906614723548,0.,25.1093486541428));
#31833=CARTESIAN_POINT('Ctrl Pts',(10.6657852303826,0.,24.9850866914374));
#31834=CARTESIAN_POINT('Ctrl Pts',(11.2237519652345,0.,24.8684985935572));
#31835=CARTESIAN_POINT('Ctrl Pts',(11.6562879503402,0.,24.7815592956469));
#31836=CARTESIAN_POINT('Ctrl Pts',(11.97300464761,0.,24.7198967418176));
#31837=CARTESIAN_POINT('Ctrl Pts',(12.1807579618051,0.,24.6803512815114));
#31838=CARTESIAN_POINT('Ctrl Pts',(12.2837868382051,0.,24.6609692735778));
#31839=CARTESIAN_POINT('',(-2.5,-3.06161699786838E-16,26.4983464639701));
#31840=CARTESIAN_POINT('Ctrl Pts',(2.5,-1.47022104461875E-15,26.4983464639701));
#31841=CARTESIAN_POINT('Ctrl Pts',(2.5,-0.0371231848941886,26.4983464639701));
#31842=CARTESIAN_POINT('Ctrl Pts',(2.49917312973535,-0.0742778661173671,
26.4983464639701));
#31843=CARTESIAN_POINT('Ctrl Pts',(2.48367897424576,-0.421532049454881,
26.4983464639701));
#31844=CARTESIAN_POINT('Ctrl Pts',(2.41221020755754,-0.726355581229532,
26.4983464639701));
#31845=CARTESIAN_POINT('Ctrl Pts',(2.15665695254898,-1.30479846977776,26.4983464639701));
#31846=CARTESIAN_POINT('Ctrl Pts',(1.97086325139701,-1.57142174542834,26.4983464639701));
#31847=CARTESIAN_POINT('Ctrl Pts',(1.50189098051651,-2.02580771968822,26.4983464639701));
#31848=CARTESIAN_POINT('Ctrl Pts',(1.22075973154356,-2.20665337385529,26.4983464639701));
#31849=CARTESIAN_POINT('Ctrl Pts',(0.605012462119597,-2.44808145431904,
26.4983464639701));
#31850=CARTESIAN_POINT('Ctrl Pts',(0.276566066778983,-2.50652231129252,
26.4983464639701));
#31851=CARTESIAN_POINT('Ctrl Pts',(-0.363347686367218,-2.49276727488126,
26.4983464639701));
#31852=CARTESIAN_POINT('Ctrl Pts',(-0.669054826467963,-2.42863662722262,
26.4983464639701));
#31853=CARTESIAN_POINT('Ctrl Pts',(-1.25208783868412,-2.18756782255767,
26.4983464639701));
#31854=CARTESIAN_POINT('Ctrl Pts',(-1.52250913573239,-2.00876650352443,
26.4983464639701));
#31855=CARTESIAN_POINT('Ctrl Pts',(-1.99007168793019,-1.54959582229107,
26.4983464639701));
#31856=CARTESIAN_POINT('Ctrl Pts',(-2.17912399473894,-1.27005950691937,
26.4983464639701));
#31857=CARTESIAN_POINT('Ctrl Pts',(-2.4346209083192,-0.656952194285376,
26.4983464639701));
#31858=CARTESIAN_POINT('Ctrl Pts',(-2.5,-0.330098701605058,26.4983464639701));
#31859=CARTESIAN_POINT('Ctrl Pts',(-2.5,-3.7470027081099E-15,26.4983464639701));
#31860=CARTESIAN_POINT('Ctrl Pts',(-2.5,-4.09394740330526E-15,26.4983464639701));
#31861=CARTESIAN_POINT('Ctrl Pts',(-2.5,0.183500133578845,26.4983464639701));
#31862=CARTESIAN_POINT('Ctrl Pts',(-2.47979662058594,0.366443746779873,
26.4983464639701));
#31863=CARTESIAN_POINT('Ctrl Pts',(-2.39698708053327,0.736795527885604,
26.4983464639701));
#31864=CARTESIAN_POINT('Ctrl Pts',(-2.33187346931883,0.922377816972309,
26.4983464639701));
#31865=CARTESIAN_POINT('Ctrl Pts',(-2.10373946785474,1.38879610419602,26.4983464639701));
#31866=CARTESIAN_POINT('Ctrl Pts',(-1.90675062561358,1.64887125615131,26.4983464639701));
#31867=CARTESIAN_POINT('Ctrl Pts',(-1.41891687160025,2.08475912057876,26.4983464639701));
#31868=CARTESIAN_POINT('Ctrl Pts',(-1.13075556057171,2.25409350772863,26.4983464639701));
#31869=CARTESIAN_POINT('Ctrl Pts',(-0.502690476103072,2.47156637397813,
26.4983464639701));
#31870=CARTESIAN_POINT('Ctrl Pts',(-0.168693444061264,2.51652152338796,
26.4983464639701));
#31871=CARTESIAN_POINT('Ctrl Pts',(0.474641333693117,2.47416054609107,26.4983464639701));
#31872=CARTESIAN_POINT('Ctrl Pts',(0.778500559957078,2.395974056961,26.4983464639701));
#31873=CARTESIAN_POINT('Ctrl Pts',(1.3524250977243,2.12722071777005,26.4983464639701));
#31874=CARTESIAN_POINT('Ctrl Pts',(1.61541268207329,1.93508746408567,26.4983464639701));
#31875=CARTESIAN_POINT('Ctrl Pts',(2.05946515295737,1.45539068556724,26.4983464639701));
#31876=CARTESIAN_POINT('Ctrl Pts',(2.2338544798984,1.17023626952827,26.4983464639701));
#31877=CARTESIAN_POINT('Ctrl Pts',(2.44852353908425,0.583828854975951,26.4983464639701));
#31878=CARTESIAN_POINT('Ctrl Pts',(2.5,0.292894735647855,26.4983464639701));
#31879=CARTESIAN_POINT('Ctrl Pts',(2.5,-1.52655665885959E-15,26.4983464639701));
#31880=CARTESIAN_POINT('Origin',(0.,0.,26.1299753788797));
#31881=CARTESIAN_POINT('',(2.49999999999983,-1.916981435175E-33,25.9968387300725));
#31882=CARTESIAN_POINT('',(-2.5,-3.06161699786838E-16,25.9968387300726));
#31883=CARTESIAN_POINT('Ctrl Pts',(2.5,0.,25.9968387300726));
#31884=CARTESIAN_POINT('Ctrl Pts',(2.5,0.0371231848941868,25.9968387300726));
#31885=CARTESIAN_POINT('Ctrl Pts',(2.49917312973534,0.0742778661173646,
25.9968387300726));
#31886=CARTESIAN_POINT('Ctrl Pts',(2.48367897424575,0.421532049454879,25.9968387300726));
#31887=CARTESIAN_POINT('Ctrl Pts',(2.41221020755754,0.726355581229529,25.9968387300726));
#31888=CARTESIAN_POINT('Ctrl Pts',(2.15665695254898,1.30479846977776,25.9968387300726));
#31889=CARTESIAN_POINT('Ctrl Pts',(1.97086325139701,1.57142174542834,25.9968387300726));
#31890=CARTESIAN_POINT('Ctrl Pts',(1.5018909805165,2.02580771968822,25.9968387300726));
#31891=CARTESIAN_POINT('Ctrl Pts',(1.22075973154356,2.20665337385528,25.9968387300726));
#31892=CARTESIAN_POINT('Ctrl Pts',(0.605012462119595,2.44808145431903,25.9968387300726));
#31893=CARTESIAN_POINT('Ctrl Pts',(0.276566066778982,2.50652231129252,25.9968387300726));
#31894=CARTESIAN_POINT('Ctrl Pts',(-0.363347686367218,2.49276727488126,
25.9968387300726));
#31895=CARTESIAN_POINT('Ctrl Pts',(-0.669054826467963,2.42863662722262,
25.9968387300726));
#31896=CARTESIAN_POINT('Ctrl Pts',(-1.25208783868412,2.18756782255767,25.9968387300726));
#31897=CARTESIAN_POINT('Ctrl Pts',(-1.52250913573239,2.00876650352443,25.9968387300726));
#31898=CARTESIAN_POINT('Ctrl Pts',(-1.99007168793019,1.54959582229107,25.9968387300726));
#31899=CARTESIAN_POINT('Ctrl Pts',(-2.17912399473894,1.27005950691936,25.9968387300726));
#31900=CARTESIAN_POINT('Ctrl Pts',(-2.4346209083192,0.656952194285369,25.9968387300726));
#31901=CARTESIAN_POINT('Ctrl Pts',(-2.5,0.330098701605053,25.9968387300726));
#31902=CARTESIAN_POINT('Ctrl Pts',(-2.5,6.93889390390723E-17,25.9968387300726));
#31903=CARTESIAN_POINT('Ctrl Pts',(-2.5,0.,25.9968387300726));
#31904=CARTESIAN_POINT('Ctrl Pts',(-2.5,-0.183500133578844,25.9968387300726));
#31905=CARTESIAN_POINT('Ctrl Pts',(-2.47979662058593,-0.366443746779865,
25.9968387300726));
#31906=CARTESIAN_POINT('Ctrl Pts',(-2.39698708053326,-0.736795527885584,
25.9968387300726));
#31907=CARTESIAN_POINT('Ctrl Pts',(-2.33187346931882,-0.922377816972283,
25.9968387300726));
#31908=CARTESIAN_POINT('Ctrl Pts',(-2.10373946785474,-1.38879610419599,
25.9968387300726));
#31909=CARTESIAN_POINT('Ctrl Pts',(-1.90675062561359,-1.64887125615128,
25.9968387300726));
#31910=CARTESIAN_POINT('Ctrl Pts',(-1.41891687160026,-2.08475912057874,
25.9968387300726));
#31911=CARTESIAN_POINT('Ctrl Pts',(-1.13075556057172,-2.25409350772861,
25.9968387300726));
#31912=CARTESIAN_POINT('Ctrl Pts',(-0.502690476103086,-2.47156637397811,
25.9968387300726));
#31913=CARTESIAN_POINT('Ctrl Pts',(-0.168693444061279,-2.51652152338795,
25.9968387300726));
#31914=CARTESIAN_POINT('Ctrl Pts',(0.474641333693102,-2.47416054609106,
25.9968387300726));
#31915=CARTESIAN_POINT('Ctrl Pts',(0.778500559957062,-2.39597405696099,
25.9968387300726));
#31916=CARTESIAN_POINT('Ctrl Pts',(1.35242509772429,-2.12722071777005,25.9968387300726));
#31917=CARTESIAN_POINT('Ctrl Pts',(1.61541268207328,-1.93508746408567,25.9968387300726));
#31918=CARTESIAN_POINT('Ctrl Pts',(2.05946515295735,-1.45539068556724,25.9968387300726));
#31919=CARTESIAN_POINT('Ctrl Pts',(2.23385447989839,-1.17023626952827,25.9968387300726));
#31920=CARTESIAN_POINT('Ctrl Pts',(2.44852353908424,-0.583828854975953,
25.9968387300726));
#31921=CARTESIAN_POINT('Ctrl Pts',(2.5,-0.292894735647857,25.9968387300726));
#31922=CARTESIAN_POINT('Ctrl Pts',(2.5,0.,25.9968387300726));
#31923=CARTESIAN_POINT('',(-2.5,-3.06161699786838E-16,26.1299753788797));
#31924=CARTESIAN_POINT('Ctrl Pts',(12.0671767507335,0.,24.1930800891729));
#31925=CARTESIAN_POINT('Ctrl Pts',(12.0671767507335,12.0671767507335,24.1930800891729));
#31926=CARTESIAN_POINT('Ctrl Pts',(0.,12.0671767507335,24.1930800891729));
#31927=CARTESIAN_POINT('Ctrl Pts',(-12.0671767507335,12.0671767507335,24.1930800891729));
#31928=CARTESIAN_POINT('Ctrl Pts',(-12.0671767507335,0.,24.1930800891729));
#31929=CARTESIAN_POINT('Ctrl Pts',(-12.0671767507335,-12.0671767507335,
24.1930800891729));
#31930=CARTESIAN_POINT('Ctrl Pts',(0.,-12.0671767507335,24.1930800891729));
#31931=CARTESIAN_POINT('Ctrl Pts',(12.0671767507335,-12.0671767507335,24.1930800891729));
#31932=CARTESIAN_POINT('Ctrl Pts',(12.0671767507335,0.,24.1930800891729));
#31933=CARTESIAN_POINT('Ctrl Pts',(12.0383097771307,0.,24.1985718545699));
#31934=CARTESIAN_POINT('Ctrl Pts',(12.0383097771307,12.0383097771307,24.1985718545699));
#31935=CARTESIAN_POINT('Ctrl Pts',(0.,12.0383097771307,24.1985718545699));
#31936=CARTESIAN_POINT('Ctrl Pts',(-12.0383097771307,12.0383097771307,24.1985718545699));
#31937=CARTESIAN_POINT('Ctrl Pts',(-12.0383097771307,0.,24.1985718545699));
#31938=CARTESIAN_POINT('Ctrl Pts',(-12.0383097771307,-12.0383097771307,
24.1985718545699));
#31939=CARTESIAN_POINT('Ctrl Pts',(0.,-12.0383097771307,24.1985718545699));
#31940=CARTESIAN_POINT('Ctrl Pts',(12.0383097771307,-12.0383097771307,24.1985718545699));
#31941=CARTESIAN_POINT('Ctrl Pts',(12.0383097771307,0.,24.1985718545699));
#31942=CARTESIAN_POINT('Ctrl Pts',(12.0093666549873,0.,24.2040992260835));
#31943=CARTESIAN_POINT('Ctrl Pts',(12.0093666549873,12.0093666549873,24.2040992260835));
#31944=CARTESIAN_POINT('Ctrl Pts',(0.,12.0093666549873,24.2040992260835));
#31945=CARTESIAN_POINT('Ctrl Pts',(-12.0093666549873,12.0093666549873,24.2040992260835));
#31946=CARTESIAN_POINT('Ctrl Pts',(-12.0093666549873,0.,24.2040992260835));
#31947=CARTESIAN_POINT('Ctrl Pts',(-12.0093666549873,-12.0093666549873,
24.2040992260835));
#31948=CARTESIAN_POINT('Ctrl Pts',(0.,-12.0093666549873,24.2040992260835));
#31949=CARTESIAN_POINT('Ctrl Pts',(12.0093666549873,-12.0093666549873,24.2040992260835));
#31950=CARTESIAN_POINT('Ctrl Pts',(12.0093666549873,0.,24.2040992260835));
#31951=CARTESIAN_POINT('Ctrl Pts',(11.9803472472225,0.,24.2096622428817));
#31952=CARTESIAN_POINT('Ctrl Pts',(11.9803472472225,11.9803472472225,24.2096622428817));
#31953=CARTESIAN_POINT('Ctrl Pts',(0.,11.9803472472225,24.2096622428817));
#31954=CARTESIAN_POINT('Ctrl Pts',(-11.9803472472225,11.9803472472225,24.2096622428817));
#31955=CARTESIAN_POINT('Ctrl Pts',(-11.9803472472225,0.,24.2096622428817));
#31956=CARTESIAN_POINT('Ctrl Pts',(-11.9803472472225,-11.9803472472225,
24.2096622428817));
#31957=CARTESIAN_POINT('Ctrl Pts',(0.,-11.9803472472225,24.2096622428817));
#31958=CARTESIAN_POINT('Ctrl Pts',(11.9803472472225,-11.9803472472225,24.2096622428817));
#31959=CARTESIAN_POINT('Ctrl Pts',(11.9803472472225,0.,24.2096622428817));
#31960=CARTESIAN_POINT('Ctrl Pts',(10.7340225064793,0.,24.448582538048));
#31961=CARTESIAN_POINT('Ctrl Pts',(10.7340225064793,10.7340225064793,24.448582538048));
#31962=CARTESIAN_POINT('Ctrl Pts',(0.,10.7340225064793,24.448582538048));
#31963=CARTESIAN_POINT('Ctrl Pts',(-10.7340225064793,10.7340225064793,24.448582538048));
#31964=CARTESIAN_POINT('Ctrl Pts',(-10.7340225064793,0.,24.448582538048));
#31965=CARTESIAN_POINT('Ctrl Pts',(-10.7340225064793,-10.7340225064793,
24.448582538048));
#31966=CARTESIAN_POINT('Ctrl Pts',(0.,-10.7340225064793,24.448582538048));
#31967=CARTESIAN_POINT('Ctrl Pts',(10.7340225064793,-10.7340225064793,24.448582538048));
#31968=CARTESIAN_POINT('Ctrl Pts',(10.7340225064793,0.,24.448582538048));
#31969=CARTESIAN_POINT('Ctrl Pts',(9.31567463360365,0.,24.7734086800262));
#31970=CARTESIAN_POINT('Ctrl Pts',(9.31567463360365,9.31567463360365,24.7734086800262));
#31971=CARTESIAN_POINT('Ctrl Pts',(0.,9.31567463360365,24.7734086800262));
#31972=CARTESIAN_POINT('Ctrl Pts',(-9.31567463360365,9.31567463360365,24.7734086800262));
#31973=CARTESIAN_POINT('Ctrl Pts',(-9.31567463360365,0.,24.7734086800262));
#31974=CARTESIAN_POINT('Ctrl Pts',(-9.31567463360365,-9.31567463360365,
24.7734086800262));
#31975=CARTESIAN_POINT('Ctrl Pts',(0.,-9.31567463360365,24.7734086800262));
#31976=CARTESIAN_POINT('Ctrl Pts',(9.31567463360365,-9.31567463360365,24.7734086800262));
#31977=CARTESIAN_POINT('Ctrl Pts',(9.31567463360365,0.,24.7734086800262));
#31978=CARTESIAN_POINT('Ctrl Pts',(7.85305095226366,0.,25.0981096808978));
#31979=CARTESIAN_POINT('Ctrl Pts',(7.85305095226366,7.85305095226366,25.0981096808978));
#31980=CARTESIAN_POINT('Ctrl Pts',(0.,7.85305095226366,25.0981096808978));
#31981=CARTESIAN_POINT('Ctrl Pts',(-7.85305095226366,7.85305095226366,25.0981096808978));
#31982=CARTESIAN_POINT('Ctrl Pts',(-7.85305095226366,0.,25.0981096808978));
#31983=CARTESIAN_POINT('Ctrl Pts',(-7.85305095226366,-7.85305095226366,
25.0981096808978));
#31984=CARTESIAN_POINT('Ctrl Pts',(0.,-7.85305095226366,25.0981096808978));
#31985=CARTESIAN_POINT('Ctrl Pts',(7.85305095226366,-7.85305095226366,25.0981096808978));
#31986=CARTESIAN_POINT('Ctrl Pts',(7.85305095226366,0.,25.0981096808978));
#31987=CARTESIAN_POINT('Ctrl Pts',(6.33330197010078,0.,25.4354924416704));
#31988=CARTESIAN_POINT('Ctrl Pts',(6.33330197010078,6.33330197010078,25.4354924416704));
#31989=CARTESIAN_POINT('Ctrl Pts',(0.,6.33330197010078,25.4354924416704));
#31990=CARTESIAN_POINT('Ctrl Pts',(-6.33330197010078,6.33330197010078,25.4354924416704));
#31991=CARTESIAN_POINT('Ctrl Pts',(-6.33330197010078,0.,25.4354924416704));
#31992=CARTESIAN_POINT('Ctrl Pts',(-6.33330197010078,-6.33330197010078,
25.4354924416704));
#31993=CARTESIAN_POINT('Ctrl Pts',(0.,-6.33330197010078,25.4354924416704));
#31994=CARTESIAN_POINT('Ctrl Pts',(6.33330197010078,-6.33330197010078,25.4354924416704));
#31995=CARTESIAN_POINT('Ctrl Pts',(6.33330197010078,0.,25.4354924416704));
#31996=CARTESIAN_POINT('Ctrl Pts',(4.84782034806848,0.,25.7184188033672));
#31997=CARTESIAN_POINT('Ctrl Pts',(4.84782034806848,4.84782034806848,25.7184188033672));
#31998=CARTESIAN_POINT('Ctrl Pts',(0.,4.84782034806848,25.7184188033672));
#31999=CARTESIAN_POINT('Ctrl Pts',(-4.84782034806848,4.84782034806848,25.7184188033672));
#32000=CARTESIAN_POINT('Ctrl Pts',(-4.84782034806848,0.,25.7184188033672));
#32001=CARTESIAN_POINT('Ctrl Pts',(-4.84782034806848,-4.84782034806848,
25.7184188033672));
#32002=CARTESIAN_POINT('Ctrl Pts',(0.,-4.84782034806848,25.7184188033672));
#32003=CARTESIAN_POINT('Ctrl Pts',(4.84782034806848,-4.84782034806848,25.7184188033672));
#32004=CARTESIAN_POINT('Ctrl Pts',(4.84782034806848,0.,25.7184188033672));
#32005=CARTESIAN_POINT('Ctrl Pts',(3.50000000000662,0.,25.8782521751276));
#32006=CARTESIAN_POINT('Ctrl Pts',(3.50000000000662,3.50000000000662,25.8782521751276));
#32007=CARTESIAN_POINT('Ctrl Pts',(0.,3.50000000000662,25.8782521751276));
#32008=CARTESIAN_POINT('Ctrl Pts',(-3.50000000000662,3.50000000000662,25.8782521751276));
#32009=CARTESIAN_POINT('Ctrl Pts',(-3.50000000000662,0.,25.8782521751276));
#32010=CARTESIAN_POINT('Ctrl Pts',(-3.50000000000662,-3.50000000000662,
25.8782521751276));
#32011=CARTESIAN_POINT('Ctrl Pts',(0.,-3.50000000000662,25.8782521751276));
#32012=CARTESIAN_POINT('Ctrl Pts',(3.50000000000662,-3.50000000000662,25.8782521751276));
#32013=CARTESIAN_POINT('Ctrl Pts',(3.50000000000662,0.,25.8782521751276));
#32014=CARTESIAN_POINT('Ctrl Pts',(2.66666666667329,0.,25.9770743042478));
#32015=CARTESIAN_POINT('Ctrl Pts',(2.66666666667329,2.66666666667329,25.9770743042478));
#32016=CARTESIAN_POINT('Ctrl Pts',(0.,2.66666666667329,25.9770743042478));
#32017=CARTESIAN_POINT('Ctrl Pts',(-2.66666666667329,2.66666666667329,25.9770743042478));
#32018=CARTESIAN_POINT('Ctrl Pts',(-2.66666666667329,0.,25.9770743042478));
#32019=CARTESIAN_POINT('Ctrl Pts',(-2.66666666667329,-2.66666666667329,
25.9770743042478));
#32020=CARTESIAN_POINT('Ctrl Pts',(0.,-2.66666666667329,25.9770743042478));
#32021=CARTESIAN_POINT('Ctrl Pts',(2.66666666667329,-2.66666666667329,25.9770743042478));
#32022=CARTESIAN_POINT('Ctrl Pts',(2.66666666667329,0.,25.9770743042478));
#32023=CARTESIAN_POINT('Ctrl Pts',(1.83333333333995,0.,26.075896433368));
#32024=CARTESIAN_POINT('Ctrl Pts',(1.83333333333995,1.83333333333995,26.075896433368));
#32025=CARTESIAN_POINT('Ctrl Pts',(0.,1.83333333333995,26.075896433368));
#32026=CARTESIAN_POINT('Ctrl Pts',(-1.83333333333995,1.83333333333995,26.075896433368));
#32027=CARTESIAN_POINT('Ctrl Pts',(-1.83333333333995,0.,26.075896433368));
#32028=CARTESIAN_POINT('Ctrl Pts',(-1.83333333333995,-1.83333333333995,
26.075896433368));
#32029=CARTESIAN_POINT('Ctrl Pts',(0.,-1.83333333333995,26.075896433368));
#32030=CARTESIAN_POINT('Ctrl Pts',(1.83333333333995,-1.83333333333995,26.075896433368));
#32031=CARTESIAN_POINT('Ctrl Pts',(1.83333333333995,0.,26.075896433368));
#32032=CARTESIAN_POINT('Ctrl Pts',(1.00000000000662,0.,26.1747185624882));
#32033=CARTESIAN_POINT('Ctrl Pts',(1.00000000000662,1.00000000000662,26.1747185624882));
#32034=CARTESIAN_POINT('Ctrl Pts',(0.,1.00000000000662,26.1747185624882));
#32035=CARTESIAN_POINT('Ctrl Pts',(-1.00000000000662,1.00000000000662,26.1747185624882));
#32036=CARTESIAN_POINT('Ctrl Pts',(-1.00000000000662,0.,26.1747185624882));
#32037=CARTESIAN_POINT('Ctrl Pts',(-1.00000000000662,-1.00000000000662,
26.1747185624882));
#32038=CARTESIAN_POINT('Ctrl Pts',(0.,-1.00000000000662,26.1747185624882));
#32039=CARTESIAN_POINT('Ctrl Pts',(1.00000000000662,-1.00000000000662,26.1747185624882));
#32040=CARTESIAN_POINT('Ctrl Pts',(1.00000000000662,0.,26.1747185624882));
#32041=CARTESIAN_POINT('',(12.0671767507335,0.,24.193080089173));
#32042=CARTESIAN_POINT('Ctrl Pts',(2.49999999999985,0.,25.9968387300726));
#32043=CARTESIAN_POINT('Ctrl Pts',(2.83333333333544,9.12848302465822E-34,
25.9573098784243));
#32044=CARTESIAN_POINT('Ctrl Pts',(3.16666666667103,-1.27798762345465E-33,
25.917781026776));
#32045=CARTESIAN_POINT('Ctrl Pts',(3.50000000000662,0.,25.8782521751276));
#32046=CARTESIAN_POINT('Ctrl Pts',(4.84782034806848,5.16749317035517E-33,
25.7184188033672));
#32047=CARTESIAN_POINT('Ctrl Pts',(6.33330197010078,-1.15944534749134E-32,
25.4354924416704));
#32048=CARTESIAN_POINT('Ctrl Pts',(7.85305095226366,0.,25.0981096808978));
#32049=CARTESIAN_POINT('Ctrl Pts',(9.31567463360365,5.24203637506798E-32,
24.7734086800262));
#32050=CARTESIAN_POINT('Ctrl Pts',(10.7340225064793,-1.70232317954933E-32,
24.448582538048));
#32051=CARTESIAN_POINT('Ctrl Pts',(11.9803472472225,0.,24.2096622428817));
#32052=CARTESIAN_POINT('Ctrl Pts',(12.0093666549873,1.04782613555734E-31,
24.2040992260835));
#32053=CARTESIAN_POINT('Ctrl Pts',(12.0383097771307,-3.99241436278348E-34,
24.1985718545699));
#32054=CARTESIAN_POINT('Ctrl Pts',(12.0671767507335,0.,24.1930800891729));
#32055=CARTESIAN_POINT('',(-12.0671767507335,-1.47780293825311E-15,24.193080089173));
#32056=CARTESIAN_POINT('Origin',(0.,0.,24.193080089173));
#32057=CARTESIAN_POINT('Origin',(0.,0.,24.193080089173));
#32058=CARTESIAN_POINT('Origin',(0.,0.,25.9634052319394));
#32059=CARTESIAN_POINT('Origin',(-13.4131653526691,-1.64263900155804E-15,
25.9634052319394));
#32060=CARTESIAN_POINT('',(0.,0.,0.));
#32061=CARTESIAN_POINT('Origin',(-2.74091738510701E-15,0.,22.3812889317585));
#32062=CARTESIAN_POINT('',(17.0820002071033,-2.09194168766635E-15,21.6712715486013));
#32063=CARTESIAN_POINT('Origin',(-2.65396533354477E-15,-2.09194168766635E-15,
21.6712715486013));
#32064=CARTESIAN_POINT('',(14.8491923750145,-1.81850159119848E-15,23.2347004240035));
#32065=CARTESIAN_POINT('',(16.067990296595,-1.96776128854558E-15,22.3812889317585));
#32066=CARTESIAN_POINT('Origin',(-2.84543015034035E-15,0.,23.2347004240035));
#32067=CARTESIAN_POINT('Origin',(-2.62888603531843E-15,0.,21.466483537529));
#32068=CARTESIAN_POINT('',(16.7952119889278,-2.05682026032416E-15,21.2616955264568));
#32069=CARTESIAN_POINT('Origin',(-2.60380673709209E-15,-2.05682026032416E-15,
21.2616955264568));
#32070=CARTESIAN_POINT('Origin',(16.9386060980155,-2.07438097399525E-15,
21.466483537529));
#32071=CARTESIAN_POINT('Origin',(-2.69161030544755E-15,0.,21.9786660718956));
#32072=CARTESIAN_POINT('',(14.542543867133,-1.78094797983444E-15,22.8390307264222));
#32073=CARTESIAN_POINT('Origin',(-2.79697458747409E-15,0.,22.8390307264222));
#32074=CARTESIAN_POINT('',(15.7712719335665,-1.93142376919247E-15,21.9786660718956));
#32075=CARTESIAN_POINT('Origin',(-2.6374721847239E-15,0.,21.5365947680606));
#32076=CARTESIAN_POINT('',(-12.2837868382052,0.,22.8390307264222));
#32077=CARTESIAN_POINT('',(12.2837868382051,-1.50433002328163E-15,22.8390307264222));
#32078=CARTESIAN_POINT('Origin',(-2.79697458747409E-15,0.,22.8390307264222));
#32079=CARTESIAN_POINT('Origin',(-2.79697458747409E-15,0.,22.8390307264222));
#32080=CARTESIAN_POINT('Origin',(13.4131653526691,-1.64263900155804E-15,
21.5365947680606));
#32081=CARTESIAN_POINT('Ctrl Pts',(-0.999999999999995,0.,20.8266817140213));
#32082=CARTESIAN_POINT('Ctrl Pts',(-0.999999999999995,0.999999999999995,
20.8266817140213));
#32083=CARTESIAN_POINT('Ctrl Pts',(-2.55053290979387E-15,0.999999999999995,
20.8266817140213));
#32084=CARTESIAN_POINT('Ctrl Pts',(0.999999999999995,0.999999999999995,
20.8266817140213));
#32085=CARTESIAN_POINT('Ctrl Pts',(0.999999999999995,0.,20.8266817140213));
#32086=CARTESIAN_POINT('Ctrl Pts',(0.999999999999995,-0.999999999999995,
20.8266817140213));
#32087=CARTESIAN_POINT('Ctrl Pts',(-2.55053290979387E-15,-0.999999999999995,
20.8266817140213));
#32088=CARTESIAN_POINT('Ctrl Pts',(-0.999999999999995,-0.999999999999995,
20.8266817140213));
#32089=CARTESIAN_POINT('Ctrl Pts',(-0.999999999999995,0.,20.8266817140213));
#32090=CARTESIAN_POINT('Ctrl Pts',(-1.5,0.,20.8850056546908));
#32091=CARTESIAN_POINT('Ctrl Pts',(-1.5,1.5,20.8850056546908));
#32092=CARTESIAN_POINT('Ctrl Pts',(-2.5576755325193E-15,1.5,20.8850056546908));
#32093=CARTESIAN_POINT('Ctrl Pts',(1.5,1.5,20.8850056546908));
#32094=CARTESIAN_POINT('Ctrl Pts',(1.5,0.,20.8850056546908));
#32095=CARTESIAN_POINT('Ctrl Pts',(1.5,-1.5,20.8850056546908));
#32096=CARTESIAN_POINT('Ctrl Pts',(-2.5576755325193E-15,-1.5,20.8850056546908));
#32097=CARTESIAN_POINT('Ctrl Pts',(-1.5,-1.5,20.8850056546908));
#32098=CARTESIAN_POINT('Ctrl Pts',(-1.5,0.,20.8850056546908));
#32099=CARTESIAN_POINT('Ctrl Pts',(-2.,0.,20.9433295953604));
#32100=CARTESIAN_POINT('Ctrl Pts',(-2.,2.,20.9433295953604));
#32101=CARTESIAN_POINT('Ctrl Pts',(-2.56481815524472E-15,2.,20.9433295953604));
#32102=CARTESIAN_POINT('Ctrl Pts',(2.,2.,20.9433295953604));
#32103=CARTESIAN_POINT('Ctrl Pts',(2.,0.,20.9433295953604));
#32104=CARTESIAN_POINT('Ctrl Pts',(2.,-2.,20.9433295953604));
#32105=CARTESIAN_POINT('Ctrl Pts',(-2.56481815524472E-15,-2.,20.9433295953604));
#32106=CARTESIAN_POINT('Ctrl Pts',(-2.,-2.,20.9433295953604));
#32107=CARTESIAN_POINT('Ctrl Pts',(-2.,0.,20.9433295953604));
#32108=CARTESIAN_POINT('Ctrl Pts',(-2.5,0.,21.0016535360299));
#32109=CARTESIAN_POINT('Ctrl Pts',(-2.5,2.5,21.0016535360299));
#32110=CARTESIAN_POINT('Ctrl Pts',(-2.57196077797015E-15,2.5,21.0016535360299));
#32111=CARTESIAN_POINT('Ctrl Pts',(2.5,2.5,21.0016535360299));
#32112=CARTESIAN_POINT('Ctrl Pts',(2.5,0.,21.0016535360299));
#32113=CARTESIAN_POINT('Ctrl Pts',(2.5,-2.5,21.0016535360299));
#32114=CARTESIAN_POINT('Ctrl Pts',(-2.57196077797015E-15,-2.5,21.0016535360299));
#32115=CARTESIAN_POINT('Ctrl Pts',(-2.5,-2.5,21.0016535360299));
#32116=CARTESIAN_POINT('Ctrl Pts',(-2.5,0.,21.0016535360299));
#32117=CARTESIAN_POINT('Ctrl Pts',(-3.,0.,21.0599774766995));
#32118=CARTESIAN_POINT('Ctrl Pts',(-3.,3.,21.0599774766995));
#32119=CARTESIAN_POINT('Ctrl Pts',(-2.57910340069557E-15,3.,21.0599774766995));
#32120=CARTESIAN_POINT('Ctrl Pts',(3.,3.,21.0599774766995));
#32121=CARTESIAN_POINT('Ctrl Pts',(3.,0.,21.0599774766995));
#32122=CARTESIAN_POINT('Ctrl Pts',(3.,-3.,21.0599774766995));
#32123=CARTESIAN_POINT('Ctrl Pts',(-2.57910340069557E-15,-3.,21.0599774766995));
#32124=CARTESIAN_POINT('Ctrl Pts',(-3.,-3.,21.0599774766995));
#32125=CARTESIAN_POINT('Ctrl Pts',(-3.,0.,21.0599774766995));
#32126=CARTESIAN_POINT('Ctrl Pts',(-3.5,0.,21.118301417369));
#32127=CARTESIAN_POINT('Ctrl Pts',(-3.5,3.5,21.118301417369));
#32128=CARTESIAN_POINT('Ctrl Pts',(-2.586246023421E-15,3.5,21.118301417369));
#32129=CARTESIAN_POINT('Ctrl Pts',(3.5,3.5,21.118301417369));
#32130=CARTESIAN_POINT('Ctrl Pts',(3.5,0.,21.118301417369));
#32131=CARTESIAN_POINT('Ctrl Pts',(3.5,-3.5,21.118301417369));
#32132=CARTESIAN_POINT('Ctrl Pts',(-2.586246023421E-15,-3.5,21.118301417369));
#32133=CARTESIAN_POINT('Ctrl Pts',(-3.5,-3.5,21.118301417369));
#32134=CARTESIAN_POINT('Ctrl Pts',(-3.5,0.,21.118301417369));
#32135=CARTESIAN_POINT('Ctrl Pts',(-3.61098900507559,0.,21.131248049663));
#32136=CARTESIAN_POINT('Ctrl Pts',(-3.61098900507559,3.61098900507559,21.131248049663));
#32137=CARTESIAN_POINT('Ctrl Pts',(-2.58783152860085E-15,3.61098900507559,
21.131248049663));
#32138=CARTESIAN_POINT('Ctrl Pts',(3.61098900507559,3.61098900507559,21.131248049663));
#32139=CARTESIAN_POINT('Ctrl Pts',(3.61098900507559,0.,21.131248049663));
#32140=CARTESIAN_POINT('Ctrl Pts',(3.61098900507559,-3.61098900507559,21.131248049663));
#32141=CARTESIAN_POINT('Ctrl Pts',(-2.58783152860085E-15,-3.61098900507559,
21.131248049663));
#32142=CARTESIAN_POINT('Ctrl Pts',(-3.61098900507559,-3.61098900507559,
21.131248049663));
#32143=CARTESIAN_POINT('Ctrl Pts',(-3.61098900507559,0.,21.131248049663));
#32144=CARTESIAN_POINT('Ctrl Pts',(-3.83416205501541,0.,21.1582981321148));
#32145=CARTESIAN_POINT('Ctrl Pts',(-3.83416205501541,3.83416205501541,21.1582981321148));
#32146=CARTESIAN_POINT('Ctrl Pts',(-2.59114420828998E-15,3.83416205501541,
21.1582981321148));
#32147=CARTESIAN_POINT('Ctrl Pts',(3.83416205501541,3.83416205501541,21.1582981321148));
#32148=CARTESIAN_POINT('Ctrl Pts',(3.83416205501541,0.,21.1582981321148));
#32149=CARTESIAN_POINT('Ctrl Pts',(3.83416205501541,-3.83416205501541,21.1582981321148));
#32150=CARTESIAN_POINT('Ctrl Pts',(-2.59114420828998E-15,-3.83416205501541,
21.1582981321148));
#32151=CARTESIAN_POINT('Ctrl Pts',(-3.83416205501541,-3.83416205501541,
21.1582981321148));
#32152=CARTESIAN_POINT('Ctrl Pts',(-3.83416205501541,0.,21.1582981321148));
#32153=CARTESIAN_POINT('Ctrl Pts',(-4.17250673641264,0.,21.2023436949734));
#32154=CARTESIAN_POINT('Ctrl Pts',(-4.17250673641264,4.17250673641263,21.2023436949734));
#32155=CARTESIAN_POINT('Ctrl Pts',(-2.59653823404712E-15,4.17250673641263,
21.2023436949734));
#32156=CARTESIAN_POINT('Ctrl Pts',(4.17250673641263,4.17250673641263,21.2023436949734));
#32157=CARTESIAN_POINT('Ctrl Pts',(4.17250673641263,0.,21.2023436949734));
#32158=CARTESIAN_POINT('Ctrl Pts',(4.17250673641263,-4.17250673641263,21.2023436949734));
#32159=CARTESIAN_POINT('Ctrl Pts',(-2.59653823404712E-15,-4.17250673641263,
21.2023436949734));
#32160=CARTESIAN_POINT('Ctrl Pts',(-4.17250673641264,-4.17250673641263,
21.2023436949734));
#32161=CARTESIAN_POINT('Ctrl Pts',(-4.17250673641264,0.,21.2023436949734));
#32162=CARTESIAN_POINT('Ctrl Pts',(-4.63085543889698,0.,21.2680625783243));
#32163=CARTESIAN_POINT('Ctrl Pts',(-4.63085543889698,4.63085543889697,21.2680625783243));
#32164=CARTESIAN_POINT('Ctrl Pts',(-2.60458647606104E-15,4.63085543889697,
21.2680625783243));
#32165=CARTESIAN_POINT('Ctrl Pts',(4.63085543889697,4.63085543889697,21.2680625783243));
#32166=CARTESIAN_POINT('Ctrl Pts',(4.63085543889697,0.,21.2680625783243));
#32167=CARTESIAN_POINT('Ctrl Pts',(4.63085543889697,-4.63085543889697,21.2680625783243));
#32168=CARTESIAN_POINT('Ctrl Pts',(-2.60458647606104E-15,-4.63085543889697,
21.2680625783243));
#32169=CARTESIAN_POINT('Ctrl Pts',(-4.63085543889698,-4.63085543889697,
21.2680625783243));
#32170=CARTESIAN_POINT('Ctrl Pts',(-4.63085543889698,0.,21.2680625783243));
#32171=CARTESIAN_POINT('Ctrl Pts',(-5.21591518523417,0.,21.362025193012));
#32172=CARTESIAN_POINT('Ctrl Pts',(-5.21591518523417,5.21591518523417,21.362025193012));
#32173=CARTESIAN_POINT('Ctrl Pts',(-2.61609357759272E-15,5.21591518523417,
21.362025193012));
#32174=CARTESIAN_POINT('Ctrl Pts',(5.21591518523417,5.21591518523417,21.362025193012));
#32175=CARTESIAN_POINT('Ctrl Pts',(5.21591518523417,0.,21.362025193012));
#32176=CARTESIAN_POINT('Ctrl Pts',(5.21591518523417,-5.21591518523417,21.362025193012));
#32177=CARTESIAN_POINT('Ctrl Pts',(-2.61609357759272E-15,-5.21591518523417,
21.362025193012));
#32178=CARTESIAN_POINT('Ctrl Pts',(-5.21591518523417,-5.21591518523417,
21.362025193012));
#32179=CARTESIAN_POINT('Ctrl Pts',(-5.21591518523417,0.,21.362025193012));
#32180=CARTESIAN_POINT('Ctrl Pts',(-5.81280340273043,0.,21.4677515363784));
#32181=CARTESIAN_POINT('Ctrl Pts',(-5.81280340273043,5.81280340273043,21.4677515363784));
#32182=CARTESIAN_POINT('Ctrl Pts',(-2.62904132039165E-15,5.81280340273043,
21.4677515363784));
#32183=CARTESIAN_POINT('Ctrl Pts',(5.81280340273042,5.81280340273043,21.4677515363784));
#32184=CARTESIAN_POINT('Ctrl Pts',(5.81280340273042,0.,21.4677515363784));
#32185=CARTESIAN_POINT('Ctrl Pts',(5.81280340273042,-5.81280340273043,21.4677515363784));
#32186=CARTESIAN_POINT('Ctrl Pts',(-2.62904132039165E-15,-5.81280340273043,
21.4677515363784));
#32187=CARTESIAN_POINT('Ctrl Pts',(-5.81280340273043,-5.81280340273043,
21.4677515363784));
#32188=CARTESIAN_POINT('Ctrl Pts',(-5.81280340273043,0.,21.4677515363784));
#32189=CARTESIAN_POINT('Ctrl Pts',(-6.42047090449388,0.,21.5847016153273));
#32190=CARTESIAN_POINT('Ctrl Pts',(-6.42047090449388,6.42047090449387,21.5847016153273));
#32191=CARTESIAN_POINT('Ctrl Pts',(-2.64336357437613E-15,6.42047090449388,
21.5847016153273));
#32192=CARTESIAN_POINT('Ctrl Pts',(6.42047090449387,6.42047090449387,21.5847016153273));
#32193=CARTESIAN_POINT('Ctrl Pts',(6.42047090449387,0.,21.5847016153273));
#32194=CARTESIAN_POINT('Ctrl Pts',(6.42047090449387,-6.42047090449387,21.5847016153273));
#32195=CARTESIAN_POINT('Ctrl Pts',(-2.64336357437613E-15,-6.42047090449388,
21.5847016153273));
#32196=CARTESIAN_POINT('Ctrl Pts',(-6.42047090449388,-6.42047090449387,
21.5847016153273));
#32197=CARTESIAN_POINT('Ctrl Pts',(-6.42047090449388,0.,21.5847016153273));
#32198=CARTESIAN_POINT('Ctrl Pts',(-7.0366882084607,0.,21.7115214030506));
#32199=CARTESIAN_POINT('Ctrl Pts',(-7.0366882084607,7.0366882084607,21.7115214030506));
#32200=CARTESIAN_POINT('Ctrl Pts',(-2.65889451908651E-15,7.0366882084607,
21.7115214030506));
#32201=CARTESIAN_POINT('Ctrl Pts',(7.0366882084607,7.0366882084607,21.7115214030506));
#32202=CARTESIAN_POINT('Ctrl Pts',(7.0366882084607,0.,21.7115214030506));
#32203=CARTESIAN_POINT('Ctrl Pts',(7.0366882084607,-7.0366882084607,21.7115214030506));
#32204=CARTESIAN_POINT('Ctrl Pts',(-2.65889451908651E-15,-7.0366882084607,
21.7115214030506));
#32205=CARTESIAN_POINT('Ctrl Pts',(-7.0366882084607,-7.0366882084607,21.7115214030506));
#32206=CARTESIAN_POINT('Ctrl Pts',(-7.0366882084607,0.,21.7115214030506));
#32207=CARTESIAN_POINT('Ctrl Pts',(-7.65759263692165,0.,21.8456924991859));
#32208=CARTESIAN_POINT('Ctrl Pts',(-7.65759263692165,7.65759263692165,21.8456924991859));
#32209=CARTESIAN_POINT('Ctrl Pts',(-2.67532573942854E-15,7.65759263692165,
21.8456924991859));
#32210=CARTESIAN_POINT('Ctrl Pts',(7.65759263692165,7.65759263692165,21.8456924991859));
#32211=CARTESIAN_POINT('Ctrl Pts',(7.65759263692165,0.,21.8456924991859));
#32212=CARTESIAN_POINT('Ctrl Pts',(7.65759263692165,-7.65759263692165,21.8456924991859));
#32213=CARTESIAN_POINT('Ctrl Pts',(-2.67532573942854E-15,-7.65759263692165,
21.8456924991859));
#32214=CARTESIAN_POINT('Ctrl Pts',(-7.65759263692165,-7.65759263692165,
21.8456924991859));
#32215=CARTESIAN_POINT('Ctrl Pts',(-7.65759263692165,0.,21.8456924991859));
#32216=CARTESIAN_POINT('Ctrl Pts',(-8.27837257578008,0.,21.9840162957912));
#32217=CARTESIAN_POINT('Ctrl Pts',(-8.27837257578008,8.27837257578008,21.9840162957912));
#32218=CARTESIAN_POINT('Ctrl Pts',(-2.69226551890439E-15,8.27837257578008,
21.9840162957912));
#32219=CARTESIAN_POINT('Ctrl Pts',(8.27837257578007,8.27837257578008,21.9840162957912));
#32220=CARTESIAN_POINT('Ctrl Pts',(8.27837257578008,0.,21.9840162957912));
#32221=CARTESIAN_POINT('Ctrl Pts',(8.27837257578007,-8.27837257578008,21.9840162957912));
#32222=CARTESIAN_POINT('Ctrl Pts',(-2.69226551890439E-15,-8.27837257578008,
21.9840162957912));
#32223=CARTESIAN_POINT('Ctrl Pts',(-8.27837257578008,-8.27837257578008,
21.9840162957912));
#32224=CARTESIAN_POINT('Ctrl Pts',(-8.27837257578008,0.,21.9840162957912));
#32225=CARTESIAN_POINT('Ctrl Pts',(-8.89388282563607,0.,22.1230393679429));
#32226=CARTESIAN_POINT('Ctrl Pts',(-8.89388282563607,8.89388282563607,22.1230393679429));
#32227=CARTESIAN_POINT('Ctrl Pts',(-2.70929093493621E-15,8.89388282563607,
22.1230393679429));
#32228=CARTESIAN_POINT('Ctrl Pts',(8.89388282563606,8.89388282563607,22.1230393679429));
#32229=CARTESIAN_POINT('Ctrl Pts',(8.89388282563607,0.,22.1230393679429));
#32230=CARTESIAN_POINT('Ctrl Pts',(8.89388282563606,-8.89388282563607,22.1230393679429));
#32231=CARTESIAN_POINT('Ctrl Pts',(-2.70929093493621E-15,-8.89388282563607,
22.1230393679429));
#32232=CARTESIAN_POINT('Ctrl Pts',(-8.89388282563607,-8.89388282563607,
22.1230393679429));
#32233=CARTESIAN_POINT('Ctrl Pts',(-8.89388282563607,0.,22.1230393679429));
#32234=CARTESIAN_POINT('Ctrl Pts',(-9.49928764562852,0.,22.2594854802591));
#32235=CARTESIAN_POINT('Ctrl Pts',(-9.49928764562852,9.49928764562851,22.2594854802591));
#32236=CARTESIAN_POINT('Ctrl Pts',(-2.72600076440663E-15,9.49928764562852,
22.2594854802591));
#32237=CARTESIAN_POINT('Ctrl Pts',(9.49928764562851,9.49928764562851,22.2594854802591));
#32238=CARTESIAN_POINT('Ctrl Pts',(9.49928764562851,0.,22.2594854802591));
#32239=CARTESIAN_POINT('Ctrl Pts',(9.49928764562851,-9.49928764562851,22.2594854802591));
#32240=CARTESIAN_POINT('Ctrl Pts',(-2.72600076440663E-15,-9.49928764562852,
22.2594854802591));
#32241=CARTESIAN_POINT('Ctrl Pts',(-9.49928764562852,-9.49928764562851,
22.2594854802591));
#32242=CARTESIAN_POINT('Ctrl Pts',(-9.49928764562852,0.,22.2594854802591));
#32243=CARTESIAN_POINT('Ctrl Pts',(-10.0906614723548,0.,22.3906513458572));
#32244=CARTESIAN_POINT('Ctrl Pts',(-10.0906614723548,10.0906614723548,22.3906513458572));
#32245=CARTESIAN_POINT('Ctrl Pts',(-2.74206395015284E-15,10.0906614723548,
22.3906513458572));
#32246=CARTESIAN_POINT('Ctrl Pts',(10.0906614723548,10.0906614723548,22.3906513458572));
#32247=CARTESIAN_POINT('Ctrl Pts',(10.0906614723548,0.,22.3906513458572));
#32248=CARTESIAN_POINT('Ctrl Pts',(10.0906614723548,-10.0906614723548,22.3906513458572));
#32249=CARTESIAN_POINT('Ctrl Pts',(-2.74206395015284E-15,-10.0906614723548,
22.3906513458572));
#32250=CARTESIAN_POINT('Ctrl Pts',(-10.0906614723548,-10.0906614723548,
22.3906513458572));
#32251=CARTESIAN_POINT('Ctrl Pts',(-10.0906614723548,0.,22.3906513458572));
#32252=CARTESIAN_POINT('Ctrl Pts',(-10.6657852303826,0.,22.5149133085626));
#32253=CARTESIAN_POINT('Ctrl Pts',(-10.6657852303826,10.6657852303826,22.5149133085626));
#32254=CARTESIAN_POINT('Ctrl Pts',(-2.75728165164113E-15,10.6657852303826,
22.5149133085626));
#32255=CARTESIAN_POINT('Ctrl Pts',(10.6657852303826,10.6657852303826,22.5149133085626));
#32256=CARTESIAN_POINT('Ctrl Pts',(10.6657852303826,0.,22.5149133085626));
#32257=CARTESIAN_POINT('Ctrl Pts',(10.6657852303826,-10.6657852303826,22.5149133085626));
#32258=CARTESIAN_POINT('Ctrl Pts',(-2.75728165164113E-15,-10.6657852303826,
22.5149133085626));
#32259=CARTESIAN_POINT('Ctrl Pts',(-10.6657852303826,-10.6657852303826,
22.5149133085626));
#32260=CARTESIAN_POINT('Ctrl Pts',(-10.6657852303826,0.,22.5149133085626));
#32261=CARTESIAN_POINT('Ctrl Pts',(-11.2237519652345,0.,22.6315014064428));
#32262=CARTESIAN_POINT('Ctrl Pts',(-11.2237519652345,11.2237519652345,22.6315014064428));
#32263=CARTESIAN_POINT('Ctrl Pts',(-2.7715595757299E-15,11.2237519652345,
22.6315014064428));
#32264=CARTESIAN_POINT('Ctrl Pts',(11.2237519652345,11.2237519652345,22.6315014064428));
#32265=CARTESIAN_POINT('Ctrl Pts',(11.2237519652345,0.,22.6315014064428));
#32266=CARTESIAN_POINT('Ctrl Pts',(11.2237519652345,-11.2237519652345,22.6315014064428));
#32267=CARTESIAN_POINT('Ctrl Pts',(-2.7715595757299E-15,-11.2237519652345,
22.6315014064428));
#32268=CARTESIAN_POINT('Ctrl Pts',(-11.2237519652345,-11.2237519652345,
22.6315014064428));
#32269=CARTESIAN_POINT('Ctrl Pts',(-11.2237519652345,0.,22.6315014064428));
#32270=CARTESIAN_POINT('Ctrl Pts',(-11.6562879503402,0.,22.7184407043531));
#32271=CARTESIAN_POINT('Ctrl Pts',(-11.6562879503402,11.6562879503402,22.7184407043531));
#32272=CARTESIAN_POINT('Ctrl Pts',(-2.7822065690205E-15,11.6562879503402,
22.7184407043531));
#32273=CARTESIAN_POINT('Ctrl Pts',(11.6562879503402,11.6562879503402,22.7184407043531));
#32274=CARTESIAN_POINT('Ctrl Pts',(11.6562879503402,0.,22.7184407043531));
#32275=CARTESIAN_POINT('Ctrl Pts',(11.6562879503402,-11.6562879503402,22.7184407043531));
#32276=CARTESIAN_POINT('Ctrl Pts',(-2.7822065690205E-15,-11.6562879503402,
22.7184407043531));
#32277=CARTESIAN_POINT('Ctrl Pts',(-11.6562879503402,-11.6562879503402,
22.7184407043531));
#32278=CARTESIAN_POINT('Ctrl Pts',(-11.6562879503402,0.,22.7184407043531));
#32279=CARTESIAN_POINT('Ctrl Pts',(-11.97300464761,0.,22.7801032581824));
#32280=CARTESIAN_POINT('Ctrl Pts',(-11.97300464761,11.97300464761,22.7801032581824));
#32281=CARTESIAN_POINT('Ctrl Pts',(-2.78975805393792E-15,11.97300464761,
22.7801032581824));
#32282=CARTESIAN_POINT('Ctrl Pts',(11.97300464761,11.97300464761,22.7801032581824));
#32283=CARTESIAN_POINT('Ctrl Pts',(11.97300464761,0.,22.7801032581824));
#32284=CARTESIAN_POINT('Ctrl Pts',(11.97300464761,-11.97300464761,22.7801032581824));
#32285=CARTESIAN_POINT('Ctrl Pts',(-2.78975805393792E-15,-11.97300464761,
22.7801032581824));
#32286=CARTESIAN_POINT('Ctrl Pts',(-11.97300464761,-11.97300464761,22.7801032581824));
#32287=CARTESIAN_POINT('Ctrl Pts',(-11.97300464761,0.,22.7801032581824));
#32288=CARTESIAN_POINT('Ctrl Pts',(-12.1807579618051,0.,22.8196487184886));
#32289=CARTESIAN_POINT('Ctrl Pts',(-12.1807579618051,12.1807579618051,22.8196487184886));
#32290=CARTESIAN_POINT('Ctrl Pts',(-2.79460097607641E-15,12.1807579618051,
22.8196487184886));
#32291=CARTESIAN_POINT('Ctrl Pts',(12.1807579618051,12.1807579618051,22.8196487184886));
#32292=CARTESIAN_POINT('Ctrl Pts',(12.1807579618051,0.,22.8196487184886));
#32293=CARTESIAN_POINT('Ctrl Pts',(12.1807579618051,-12.1807579618051,22.8196487184886));
#32294=CARTESIAN_POINT('Ctrl Pts',(-2.79460097607641E-15,-12.1807579618051,
22.8196487184886));
#32295=CARTESIAN_POINT('Ctrl Pts',(-12.1807579618051,-12.1807579618051,
22.8196487184886));
#32296=CARTESIAN_POINT('Ctrl Pts',(-12.1807579618051,0.,22.8196487184886));
#32297=CARTESIAN_POINT('Ctrl Pts',(-12.2837868382052,0.,22.8390307264222));
#32298=CARTESIAN_POINT('Ctrl Pts',(-12.2837868382052,12.2837868382051,22.8390307264222));
#32299=CARTESIAN_POINT('Ctrl Pts',(-2.79697458747409E-15,12.2837868382051,
22.8390307264222));
#32300=CARTESIAN_POINT('Ctrl Pts',(12.2837868382051,12.2837868382051,22.8390307264222));
#32301=CARTESIAN_POINT('Ctrl Pts',(12.2837868382051,0.,22.8390307264222));
#32302=CARTESIAN_POINT('Ctrl Pts',(12.2837868382051,-12.2837868382051,22.8390307264222));
#32303=CARTESIAN_POINT('Ctrl Pts',(-2.79697458747409E-15,-12.2837868382051,
22.8390307264222));
#32304=CARTESIAN_POINT('Ctrl Pts',(-12.2837868382052,-12.2837868382051,
22.8390307264222));
#32305=CARTESIAN_POINT('Ctrl Pts',(-12.2837868382052,0.,22.8390307264222));
#32306=CARTESIAN_POINT('',(-2.5,0.,21.0016535360299));
#32307=CARTESIAN_POINT('Ctrl Pts',(-2.5,0.,21.0016535360299));
#32308=CARTESIAN_POINT('Ctrl Pts',(-2.7,0.,21.0249831122978));
#32309=CARTESIAN_POINT('Ctrl Pts',(-2.9,0.,21.0483126885656));
#32310=CARTESIAN_POINT('Ctrl Pts',(-3.1,0.,21.0716422648334));
#32311=CARTESIAN_POINT('Ctrl Pts',(-3.3,0.,21.0949718411012));
#32312=CARTESIAN_POINT('Ctrl Pts',(-3.5,0.,21.118301417369));
#32313=CARTESIAN_POINT('Ctrl Pts',(-3.61098900507559,0.,21.131248049663));
#32314=CARTESIAN_POINT('Ctrl Pts',(-3.83416205501541,0.,21.1582981321148));
#32315=CARTESIAN_POINT('Ctrl Pts',(-4.17250673641264,0.,21.2023436949734));
#32316=CARTESIAN_POINT('Ctrl Pts',(-4.63085543889698,0.,21.2680625783243));
#32317=CARTESIAN_POINT('Ctrl Pts',(-5.21591518523417,0.,21.362025193012));
#32318=CARTESIAN_POINT('Ctrl Pts',(-5.81280340273043,0.,21.4677515363784));
#32319=CARTESIAN_POINT('Ctrl Pts',(-6.42047090449388,0.,21.5847016153273));
#32320=CARTESIAN_POINT('Ctrl Pts',(-7.0366882084607,0.,21.7115214030506));
#32321=CARTESIAN_POINT('Ctrl Pts',(-7.65759263692165,0.,21.8456924991859));
#32322=CARTESIAN_POINT('Ctrl Pts',(-8.27837257578008,0.,21.9840162957912));
#32323=CARTESIAN_POINT('Ctrl Pts',(-8.89388282563607,0.,22.1230393679429));
#32324=CARTESIAN_POINT('Ctrl Pts',(-9.49928764562852,0.,22.2594854802591));
#32325=CARTESIAN_POINT('Ctrl Pts',(-10.0906614723548,0.,22.3906513458572));
#32326=CARTESIAN_POINT('Ctrl Pts',(-10.6657852303826,0.,22.5149133085626));
#32327=CARTESIAN_POINT('Ctrl Pts',(-11.2237519652345,0.,22.6315014064428));
#32328=CARTESIAN_POINT('Ctrl Pts',(-11.6562879503402,0.,22.7184407043531));
#32329=CARTESIAN_POINT('Ctrl Pts',(-11.97300464761,0.,22.7801032581824));
#32330=CARTESIAN_POINT('Ctrl Pts',(-12.1807579618051,0.,22.8196487184886));
#32331=CARTESIAN_POINT('Ctrl Pts',(-12.2837868382052,0.,22.8390307264222));
#32332=CARTESIAN_POINT('',(2.5,-3.06161699786838E-16,21.0016535360299));
#32333=CARTESIAN_POINT('Ctrl Pts',(-2.5,-1.47022104461876E-15,21.0016535360299));
#32334=CARTESIAN_POINT('Ctrl Pts',(-2.5,-0.0371231848941886,21.0016535360299));
#32335=CARTESIAN_POINT('Ctrl Pts',(-2.49917312973535,-0.0742778661173672,
21.0016535360299));
#32336=CARTESIAN_POINT('Ctrl Pts',(-2.48367897424576,-0.421532049454882,
21.0016535360299));
#32337=CARTESIAN_POINT('Ctrl Pts',(-2.41221020755755,-0.726355581229533,
21.0016535360299));
#32338=CARTESIAN_POINT('Ctrl Pts',(-2.15665695254898,-1.30479846977776,
21.0016535360299));
#32339=CARTESIAN_POINT('Ctrl Pts',(-1.97086325139701,-1.57142174542834,
21.0016535360299));
#32340=CARTESIAN_POINT('Ctrl Pts',(-1.50189098051651,-2.02580771968822,
21.0016535360299));
#32341=CARTESIAN_POINT('Ctrl Pts',(-1.22075973154356,-2.20665337385529,
21.0016535360299));
#32342=CARTESIAN_POINT('Ctrl Pts',(-0.605012462119601,-2.44808145431904,
21.0016535360299));
#32343=CARTESIAN_POINT('Ctrl Pts',(-0.276566066778985,-2.50652231129252,
21.0016535360299));
#32344=CARTESIAN_POINT('Ctrl Pts',(0.363347686367216,-2.49276727488126,
21.0016535360299));
#32345=CARTESIAN_POINT('Ctrl Pts',(0.669054826467961,-2.42863662722262,
21.0016535360299));
#32346=CARTESIAN_POINT('Ctrl Pts',(1.25208783868412,-2.18756782255767,21.0016535360299));
#32347=CARTESIAN_POINT('Ctrl Pts',(1.52250913573239,-2.00876650352443,21.0016535360299));
#32348=CARTESIAN_POINT('Ctrl Pts',(1.99007168793019,-1.54959582229107,21.0016535360299));
#32349=CARTESIAN_POINT('Ctrl Pts',(2.17912399473894,-1.27005950691937,21.0016535360299));
#32350=CARTESIAN_POINT('Ctrl Pts',(2.43462090831919,-0.656952194285372,
21.0016535360299));
#32351=CARTESIAN_POINT('Ctrl Pts',(2.5,-0.330098701605055,21.0016535360299));
#32352=CARTESIAN_POINT('Ctrl Pts',(2.5,-1.45716771982052E-15,21.0016535360299));
#32353=CARTESIAN_POINT('Ctrl Pts',(2.5,-1.42247325030098E-15,21.0016535360299));
#32354=CARTESIAN_POINT('Ctrl Pts',(2.5,0.183500133578845,21.0016535360299));
#32355=CARTESIAN_POINT('Ctrl Pts',(2.47979662058594,0.36644374677987,21.0016535360299));
#32356=CARTESIAN_POINT('Ctrl Pts',(2.39698708053327,0.736795527885595,21.0016535360299));
#32357=CARTESIAN_POINT('Ctrl Pts',(2.33187346931883,0.922377816972297,21.0016535360299));
#32358=CARTESIAN_POINT('Ctrl Pts',(2.10373946785474,1.38879610419601,21.0016535360299));
#32359=CARTESIAN_POINT('Ctrl Pts',(1.90675062561359,1.6488712561513,21.0016535360299));
#32360=CARTESIAN_POINT('Ctrl Pts',(1.41891687160026,2.08475912057876,21.0016535360299));
#32361=CARTESIAN_POINT('Ctrl Pts',(1.13075556057171,2.25409350772862,21.0016535360299));
#32362=CARTESIAN_POINT('Ctrl Pts',(0.502690476103074,2.47156637397813,21.0016535360299));
#32363=CARTESIAN_POINT('Ctrl Pts',(0.168693444061263,2.51652152338796,21.0016535360299));
#32364=CARTESIAN_POINT('Ctrl Pts',(-0.474641333693119,2.47416054609107,
21.0016535360299));
#32365=CARTESIAN_POINT('Ctrl Pts',(-0.77850055995708,2.395974056961,21.0016535360299));
#32366=CARTESIAN_POINT('Ctrl Pts',(-1.35242509772431,2.12722071777005,21.0016535360299));
#32367=CARTESIAN_POINT('Ctrl Pts',(-1.61541268207329,1.93508746408567,21.0016535360299));
#32368=CARTESIAN_POINT('Ctrl Pts',(-2.05946515295737,1.45539068556724,21.0016535360299));
#32369=CARTESIAN_POINT('Ctrl Pts',(-2.23385447989841,1.17023626952827,21.0016535360299));
#32370=CARTESIAN_POINT('Ctrl Pts',(-2.44852353908426,0.583828854975952,
21.0016535360299));
#32371=CARTESIAN_POINT('Ctrl Pts',(-2.5,0.292894735647856,21.0016535360299));
#32372=CARTESIAN_POINT('Ctrl Pts',(-2.5,-1.52655665885959E-15,21.0016535360299));
#32373=CARTESIAN_POINT('Origin',(-2.61707322499551E-15,0.,21.3700246211203));
#32374=CARTESIAN_POINT('',(-2.49999999999983,4.22182696387148E-32,21.5031612699275));
#32375=CARTESIAN_POINT('',(2.5,-3.06161699786838E-16,21.5031612699274));
#32376=CARTESIAN_POINT('Ctrl Pts',(-2.5,-2.09528118263808E-15,21.5031612699274));
#32377=CARTESIAN_POINT('Ctrl Pts',(-2.5,0.0371231848941853,21.5031612699274));
#32378=CARTESIAN_POINT('Ctrl Pts',(-2.49917312973534,0.0742778661173668,
21.5031612699274));
#32379=CARTESIAN_POINT('Ctrl Pts',(-2.48367897424575,0.421532049454881,
21.5031612699274));
#32380=CARTESIAN_POINT('Ctrl Pts',(-2.41221020755754,0.726355581229531,
21.5031612699274));
#32381=CARTESIAN_POINT('Ctrl Pts',(-2.15665695254898,1.30479846977776,21.5031612699274));
#32382=CARTESIAN_POINT('Ctrl Pts',(-1.97086325139701,1.57142174542834,21.5031612699274));
#32383=CARTESIAN_POINT('Ctrl Pts',(-1.50189098051651,2.02580771968822,21.5031612699274));
#32384=CARTESIAN_POINT('Ctrl Pts',(-1.22075973154356,2.20665337385528,21.5031612699274));
#32385=CARTESIAN_POINT('Ctrl Pts',(-0.605012462119599,2.44808145431903,
21.5031612699274));
#32386=CARTESIAN_POINT('Ctrl Pts',(-0.276566066778986,2.50652231129252,
21.5031612699274));
#32387=CARTESIAN_POINT('Ctrl Pts',(0.363347686367214,2.49276727488126,21.5031612699274));
#32388=CARTESIAN_POINT('Ctrl Pts',(0.669054826467959,2.42863662722262,21.5031612699274));
#32389=CARTESIAN_POINT('Ctrl Pts',(1.25208783868411,2.18756782255767,21.5031612699274));
#32390=CARTESIAN_POINT('Ctrl Pts',(1.52250913573239,2.00876650352443,21.5031612699274));
#32391=CARTESIAN_POINT('Ctrl Pts',(1.99007168793019,1.54959582229107,21.5031612699274));
#32392=CARTESIAN_POINT('Ctrl Pts',(2.17912399473894,1.27005950691937,21.5031612699274));
#32393=CARTESIAN_POINT('Ctrl Pts',(2.43462090831919,0.65695219428537,21.5031612699274));
#32394=CARTESIAN_POINT('Ctrl Pts',(2.5,0.330098701605054,21.5031612699274));
#32395=CARTESIAN_POINT('Ctrl Pts',(2.5,-6.93889390390723E-17,21.5031612699274));
#32396=CARTESIAN_POINT('Ctrl Pts',(2.5,-2.42861286636753E-16,21.5031612699274));
#32397=CARTESIAN_POINT('Ctrl Pts',(2.5,-0.183500133578842,21.5031612699274));
#32398=CARTESIAN_POINT('Ctrl Pts',(2.47979662058591,-0.366443746779858,
21.5031612699274));
#32399=CARTESIAN_POINT('Ctrl Pts',(2.39698708053325,-0.736795527885571,
21.5031612699274));
#32400=CARTESIAN_POINT('Ctrl Pts',(2.33187346931882,-0.922377816972267,
21.5031612699274));
#32401=CARTESIAN_POINT('Ctrl Pts',(2.10373946785474,-1.38879610419597,21.5031612699274));
#32402=CARTESIAN_POINT('Ctrl Pts',(1.90675062561359,-1.64887125615127,21.5031612699274));
#32403=CARTESIAN_POINT('Ctrl Pts',(1.41891687160027,-2.08475912057872,21.5031612699274));
#32404=CARTESIAN_POINT('Ctrl Pts',(1.13075556057173,-2.25409350772859,21.5031612699274));
#32405=CARTESIAN_POINT('Ctrl Pts',(0.502690476103094,-2.4715663739781,21.5031612699274));
#32406=CARTESIAN_POINT('Ctrl Pts',(0.168693444061285,-2.51652152338794,
21.5031612699274));
#32407=CARTESIAN_POINT('Ctrl Pts',(-0.4746413336931,-2.47416054609105,21.5031612699274));
#32408=CARTESIAN_POINT('Ctrl Pts',(-0.778500559957059,-2.39597405696099,
21.5031612699274));
#32409=CARTESIAN_POINT('Ctrl Pts',(-1.35242509772429,-2.12722071777004,
21.5031612699274));
#32410=CARTESIAN_POINT('Ctrl Pts',(-1.61541268207327,-1.93508746408566,
21.5031612699274));
#32411=CARTESIAN_POINT('Ctrl Pts',(-2.05946515295735,-1.45539068556723,
21.5031612699274));
#32412=CARTESIAN_POINT('Ctrl Pts',(-2.23385447989839,-1.17023626952826,
21.5031612699274));
#32413=CARTESIAN_POINT('Ctrl Pts',(-2.44852353908424,-0.583828854975948,
21.5031612699274));
#32414=CARTESIAN_POINT('Ctrl Pts',(-2.5,-0.292894735647858,21.5031612699274));
#32415=CARTESIAN_POINT('Ctrl Pts',(-2.5,-2.28983498828939E-15,21.5031612699274));
#32416=CARTESIAN_POINT('',(2.5,-3.06161699786838E-16,21.3700246211203));
#32417=CARTESIAN_POINT('Ctrl Pts',(-12.0671767507335,0.,23.3069199108271));
#32418=CARTESIAN_POINT('Ctrl Pts',(-12.0671767507335,12.0671767507335,23.3069199108271));
#32419=CARTESIAN_POINT('Ctrl Pts',(-2.85427448667781E-15,12.0671767507335,
23.3069199108271));
#32420=CARTESIAN_POINT('Ctrl Pts',(12.0671767507335,12.0671767507335,23.3069199108271));
#32421=CARTESIAN_POINT('Ctrl Pts',(12.0671767507335,0.,23.3069199108271));
#32422=CARTESIAN_POINT('Ctrl Pts',(12.0671767507335,-12.0671767507335,23.3069199108271));
#32423=CARTESIAN_POINT('Ctrl Pts',(-2.85427448667781E-15,-12.0671767507335,
23.3069199108271));
#32424=CARTESIAN_POINT('Ctrl Pts',(-12.0671767507335,-12.0671767507335,
23.3069199108271));
#32425=CARTESIAN_POINT('Ctrl Pts',(-12.0671767507335,0.,23.3069199108271));
#32426=CARTESIAN_POINT('Ctrl Pts',(-12.0383097771307,0.,23.3014281454301));
#32427=CARTESIAN_POINT('Ctrl Pts',(-12.0383097771307,12.0383097771307,23.3014281454301));
#32428=CARTESIAN_POINT('Ctrl Pts',(-2.85360193938631E-15,12.0383097771307,
23.3014281454301));
#32429=CARTESIAN_POINT('Ctrl Pts',(12.0383097771306,12.0383097771307,23.3014281454301));
#32430=CARTESIAN_POINT('Ctrl Pts',(12.0383097771307,0.,23.3014281454301));
#32431=CARTESIAN_POINT('Ctrl Pts',(12.0383097771306,-12.0383097771307,23.3014281454301));
#32432=CARTESIAN_POINT('Ctrl Pts',(-2.85360193938631E-15,-12.0383097771307,
23.3014281454301));
#32433=CARTESIAN_POINT('Ctrl Pts',(-12.0383097771307,-12.0383097771307,
23.3014281454301));
#32434=CARTESIAN_POINT('Ctrl Pts',(-12.0383097771307,0.,23.3014281454301));
#32435=CARTESIAN_POINT('Ctrl Pts',(-12.0093666549873,0.,23.2959007739165));
#32436=CARTESIAN_POINT('Ctrl Pts',(-12.0093666549873,12.0093666549873,23.2959007739165));
#32437=CARTESIAN_POINT('Ctrl Pts',(-2.85292503160311E-15,12.0093666549873,
23.2959007739165));
#32438=CARTESIAN_POINT('Ctrl Pts',(12.0093666549873,12.0093666549873,23.2959007739165));
#32439=CARTESIAN_POINT('Ctrl Pts',(12.0093666549873,0.,23.2959007739165));
#32440=CARTESIAN_POINT('Ctrl Pts',(12.0093666549873,-12.0093666549873,23.2959007739165));
#32441=CARTESIAN_POINT('Ctrl Pts',(-2.85292503160311E-15,-12.0093666549873,
23.2959007739165));
#32442=CARTESIAN_POINT('Ctrl Pts',(-12.0093666549873,-12.0093666549873,
23.2959007739165));
#32443=CARTESIAN_POINT('Ctrl Pts',(-12.0093666549873,0.,23.2959007739165));
#32444=CARTESIAN_POINT('Ctrl Pts',(-11.9803472472225,0.,23.2903377571183));
#32445=CARTESIAN_POINT('Ctrl Pts',(-11.9803472472225,11.9803472472225,23.2903377571183));
#32446=CARTESIAN_POINT('Ctrl Pts',(-2.85224375853157E-15,11.9803472472225,
23.2903377571183));
#32447=CARTESIAN_POINT('Ctrl Pts',(11.9803472472225,11.9803472472225,23.2903377571183));
#32448=CARTESIAN_POINT('Ctrl Pts',(11.9803472472225,0.,23.2903377571183));
#32449=CARTESIAN_POINT('Ctrl Pts',(11.9803472472225,-11.9803472472225,23.2903377571183));
#32450=CARTESIAN_POINT('Ctrl Pts',(-2.85224375853157E-15,-11.9803472472225,
23.2903377571183));
#32451=CARTESIAN_POINT('Ctrl Pts',(-11.9803472472225,-11.9803472472225,
23.2903377571183));
#32452=CARTESIAN_POINT('Ctrl Pts',(-11.9803472472225,0.,23.2903377571183));
#32453=CARTESIAN_POINT('Ctrl Pts',(-10.7340225064793,0.,23.051417461952));
#32454=CARTESIAN_POINT('Ctrl Pts',(-10.7340225064793,10.7340225064793,23.051417461952));
#32455=CARTESIAN_POINT('Ctrl Pts',(-2.82298446105889E-15,10.7340225064793,
23.051417461952));
#32456=CARTESIAN_POINT('Ctrl Pts',(10.7340225064793,10.7340225064793,23.051417461952));
#32457=CARTESIAN_POINT('Ctrl Pts',(10.7340225064793,0.,23.051417461952));
#32458=CARTESIAN_POINT('Ctrl Pts',(10.7340225064793,-10.7340225064793,23.051417461952));
#32459=CARTESIAN_POINT('Ctrl Pts',(-2.82298446105889E-15,-10.7340225064793,
23.051417461952));
#32460=CARTESIAN_POINT('Ctrl Pts',(-10.7340225064793,-10.7340225064793,
23.051417461952));
#32461=CARTESIAN_POINT('Ctrl Pts',(-10.7340225064793,0.,23.051417461952));
#32462=CARTESIAN_POINT('Ctrl Pts',(-9.31567463360365,0.,22.7265913199738));
#32463=CARTESIAN_POINT('Ctrl Pts',(-9.31567463360365,9.31567463360365,22.7265913199738));
#32464=CARTESIAN_POINT('Ctrl Pts',(-2.78320473155359E-15,9.31567463360365,
22.7265913199738));
#32465=CARTESIAN_POINT('Ctrl Pts',(9.31567463360364,9.31567463360365,22.7265913199738));
#32466=CARTESIAN_POINT('Ctrl Pts',(9.31567463360365,0.,22.7265913199738));
#32467=CARTESIAN_POINT('Ctrl Pts',(9.31567463360364,-9.31567463360365,22.7265913199738));
#32468=CARTESIAN_POINT('Ctrl Pts',(-2.78320473155359E-15,-9.31567463360365,
22.7265913199738));
#32469=CARTESIAN_POINT('Ctrl Pts',(-9.31567463360365,-9.31567463360365,
22.7265913199738));
#32470=CARTESIAN_POINT('Ctrl Pts',(-9.31567463360365,0.,22.7265913199738));
#32471=CARTESIAN_POINT('Ctrl Pts',(-7.85305095226366,0.,22.4018903191022));
#32472=CARTESIAN_POINT('Ctrl Pts',(-7.85305095226366,7.85305095226366,22.4018903191022));
#32473=CARTESIAN_POINT('Ctrl Pts',(-2.74344032741386E-15,7.85305095226366,
22.4018903191022));
#32474=CARTESIAN_POINT('Ctrl Pts',(7.85305095226366,7.85305095226366,22.4018903191022));
#32475=CARTESIAN_POINT('Ctrl Pts',(7.85305095226366,0.,22.4018903191022));
#32476=CARTESIAN_POINT('Ctrl Pts',(7.85305095226366,-7.85305095226366,22.4018903191022));
#32477=CARTESIAN_POINT('Ctrl Pts',(-2.74344032741386E-15,-7.85305095226366,
22.4018903191022));
#32478=CARTESIAN_POINT('Ctrl Pts',(-7.85305095226366,-7.85305095226366,
22.4018903191022));
#32479=CARTESIAN_POINT('Ctrl Pts',(-7.85305095226366,0.,22.4018903191022));
#32480=CARTESIAN_POINT('Ctrl Pts',(-6.33330197010078,0.,22.0645075583296));
#32481=CARTESIAN_POINT('Ctrl Pts',(-6.33330197010078,6.33330197010078,22.0645075583296));
#32482=CARTESIAN_POINT('Ctrl Pts',(-2.70212285560709E-15,6.33330197010078,
22.0645075583296));
#32483=CARTESIAN_POINT('Ctrl Pts',(6.33330197010078,6.33330197010078,22.0645075583296));
#32484=CARTESIAN_POINT('Ctrl Pts',(6.33330197010078,0.,22.0645075583296));
#32485=CARTESIAN_POINT('Ctrl Pts',(6.33330197010078,-6.33330197010078,22.0645075583296));
#32486=CARTESIAN_POINT('Ctrl Pts',(-2.70212285560709E-15,-6.33330197010078,
22.0645075583296));
#32487=CARTESIAN_POINT('Ctrl Pts',(-6.33330197010078,-6.33330197010078,
22.0645075583296));
#32488=CARTESIAN_POINT('Ctrl Pts',(-6.33330197010078,0.,22.0645075583296));
#32489=CARTESIAN_POINT('Ctrl Pts',(-4.84782034806848,0.,21.7815811966328));
#32490=CARTESIAN_POINT('Ctrl Pts',(-4.84782034806848,4.84782034806848,21.7815811966328));
#32491=CARTESIAN_POINT('Ctrl Pts',(-2.66747436928245E-15,4.84782034806848,
21.7815811966328));
#32492=CARTESIAN_POINT('Ctrl Pts',(4.84782034806847,4.84782034806848,21.7815811966328));
#32493=CARTESIAN_POINT('Ctrl Pts',(4.84782034806847,0.,21.7815811966328));
#32494=CARTESIAN_POINT('Ctrl Pts',(4.84782034806847,-4.84782034806848,21.7815811966328));
#32495=CARTESIAN_POINT('Ctrl Pts',(-2.66747436928245E-15,-4.84782034806848,
21.7815811966328));
#32496=CARTESIAN_POINT('Ctrl Pts',(-4.84782034806848,-4.84782034806848,
21.7815811966328));
#32497=CARTESIAN_POINT('Ctrl Pts',(-4.84782034806848,0.,21.7815811966328));
#32498=CARTESIAN_POINT('Ctrl Pts',(-3.50000000000663,0.,21.6217478248724));
#32499=CARTESIAN_POINT('Ctrl Pts',(-3.50000000000662,3.50000000000662,21.6217478248724));
#32500=CARTESIAN_POINT('Ctrl Pts',(-2.64790042657012E-15,3.50000000000662,
21.6217478248724));
#32501=CARTESIAN_POINT('Ctrl Pts',(3.50000000000662,3.50000000000662,21.6217478248724));
#32502=CARTESIAN_POINT('Ctrl Pts',(3.50000000000662,0.,21.6217478248724));
#32503=CARTESIAN_POINT('Ctrl Pts',(3.50000000000662,-3.50000000000662,21.6217478248724));
#32504=CARTESIAN_POINT('Ctrl Pts',(-2.64790042657012E-15,-3.50000000000662,
21.6217478248724));
#32505=CARTESIAN_POINT('Ctrl Pts',(-3.50000000000662,-3.50000000000662,
21.6217478248724));
#32506=CARTESIAN_POINT('Ctrl Pts',(-3.50000000000663,0.,21.6217478248724));
#32507=CARTESIAN_POINT('Ctrl Pts',(-2.6666666666733,0.,21.5229256957522));
#32508=CARTESIAN_POINT('Ctrl Pts',(-2.66666666667328,2.66666666667328,21.5229256957522));
#32509=CARTESIAN_POINT('Ctrl Pts',(-2.63579820615892E-15,2.66666666667328,
21.5229256957522));
#32510=CARTESIAN_POINT('Ctrl Pts',(2.66666666667329,2.66666666667328,21.5229256957522));
#32511=CARTESIAN_POINT('Ctrl Pts',(2.66666666667329,0.,21.5229256957522));
#32512=CARTESIAN_POINT('Ctrl Pts',(2.66666666667329,-2.66666666667328,21.5229256957522));
#32513=CARTESIAN_POINT('Ctrl Pts',(-2.63579820615892E-15,-2.66666666667328,
21.5229256957522));
#32514=CARTESIAN_POINT('Ctrl Pts',(-2.66666666667328,-2.66666666667328,
21.5229256957522));
#32515=CARTESIAN_POINT('Ctrl Pts',(-2.6666666666733,0.,21.5229256957522));
#32516=CARTESIAN_POINT('Ctrl Pts',(-1.83333333333996,0.,21.424103566632));
#32517=CARTESIAN_POINT('Ctrl Pts',(-1.83333333333994,1.83333333333994,21.424103566632));
#32518=CARTESIAN_POINT('Ctrl Pts',(-2.62369598574772E-15,1.83333333333994,
21.424103566632));
#32519=CARTESIAN_POINT('Ctrl Pts',(1.83333333333995,1.83333333333994,21.424103566632));
#32520=CARTESIAN_POINT('Ctrl Pts',(1.83333333333995,0.,21.424103566632));
#32521=CARTESIAN_POINT('Ctrl Pts',(1.83333333333995,-1.83333333333994,21.424103566632));
#32522=CARTESIAN_POINT('Ctrl Pts',(-2.62369598574772E-15,-1.83333333333994,
21.424103566632));
#32523=CARTESIAN_POINT('Ctrl Pts',(-1.83333333333994,-1.83333333333994,
21.424103566632));
#32524=CARTESIAN_POINT('Ctrl Pts',(-1.83333333333996,0.,21.424103566632));
#32525=CARTESIAN_POINT('Ctrl Pts',(-1.00000000000663,0.,21.3252814375118));
#32526=CARTESIAN_POINT('Ctrl Pts',(-1.0000000000066,1.0000000000066,21.3252814375118));
#32527=CARTESIAN_POINT('Ctrl Pts',(-2.61159376533653E-15,1.0000000000066,
21.3252814375118));
#32528=CARTESIAN_POINT('Ctrl Pts',(1.00000000000662,1.0000000000066,21.3252814375118));
#32529=CARTESIAN_POINT('Ctrl Pts',(1.00000000000662,0.,21.3252814375118));
#32530=CARTESIAN_POINT('Ctrl Pts',(1.00000000000662,-1.0000000000066,21.3252814375118));
#32531=CARTESIAN_POINT('Ctrl Pts',(-2.61159376533653E-15,-1.0000000000066,
21.3252814375118));
#32532=CARTESIAN_POINT('Ctrl Pts',(-1.0000000000066,-1.0000000000066,21.3252814375118));
#32533=CARTESIAN_POINT('Ctrl Pts',(-1.00000000000663,0.,21.3252814375118));
#32534=CARTESIAN_POINT('',(-12.0671767507335,0.,23.306919910827));
#32535=CARTESIAN_POINT('Ctrl Pts',(-2.49999999999985,0.,21.5031612699274));
#32536=CARTESIAN_POINT('Ctrl Pts',(-2.83333333333544,3.69612852901595E-47,
21.5426901215757));
#32537=CARTESIAN_POINT('Ctrl Pts',(-3.16666666667104,-5.17457994063246E-47,
21.5822189732241));
#32538=CARTESIAN_POINT('Ctrl Pts',(-3.50000000000663,0.,21.6217478248724));
#32539=CARTESIAN_POINT('Ctrl Pts',(-4.84782034806848,1.63733269291844E-31,
21.7815811966328));
#32540=CARTESIAN_POINT('Ctrl Pts',(-6.33330197010078,-4.7731456426033E-46,
22.0645075583296));
#32541=CARTESIAN_POINT('Ctrl Pts',(-7.85305095226366,0.,22.4018903191022));
#32542=CARTESIAN_POINT('Ctrl Pts',(-9.31567463360365,3.14633330838416E-31,
22.7265913199738));
#32543=CARTESIAN_POINT('Ctrl Pts',(-10.7340225064793,-6.85272008724022E-46,
23.051417461952));
#32544=CARTESIAN_POINT('Ctrl Pts',(-11.9803472472225,0.,23.2903377571183));
#32545=CARTESIAN_POINT('Ctrl Pts',(-12.0093666549873,4.05611743704363E-31,
23.2959007739165));
#32546=CARTESIAN_POINT('Ctrl Pts',(-12.0383097771307,-1.61138616161747E-47,
23.3014281454301));
#32547=CARTESIAN_POINT('Ctrl Pts',(-12.0671767507335,0.,23.3069199108271));
#32548=CARTESIAN_POINT('',(12.0671767507335,-1.47780293825311E-15,23.306919910827));
#32549=CARTESIAN_POINT('Origin',(-2.85427448667781E-15,0.,23.306919910827));
#32550=CARTESIAN_POINT('Origin',(-2.85427448667781E-15,0.,23.306919910827));
#32551=CARTESIAN_POINT('Origin',(-2.6374721847239E-15,0.,21.5365947680606));
#32552=CARTESIAN_POINT('Origin',(13.4131653526691,-1.64263900155804E-15,
21.5365947680606));
#32553=CARTESIAN_POINT('',(0.,0.,0.));
#32554=CARTESIAN_POINT('Ctrl Pts',(-4.,0.,5.));
#32555=CARTESIAN_POINT('Ctrl Pts',(-4.05262307141051,-0.654498469497874,
5.09114583333333));
#32556=CARTESIAN_POINT('Ctrl Pts',(-3.83031081101585,-2.0164870728516,5.2734375));
#32557=CARTESIAN_POINT('Ctrl Pts',(-2.51852354898032,-3.7208214715467,5.546875));
#32558=CARTESIAN_POINT('Ctrl Pts',(-0.483385262891241,-4.63216118014149,
5.82031249999999));
#32559=CARTESIAN_POINT('Ctrl Pts',(1.8202315402997,-4.46495458019068,6.09375000000001));
#32560=CARTESIAN_POINT('Ctrl Pts',(3.83708110788313,-3.18392684763,6.36718749999999));
#32561=CARTESIAN_POINT('Ctrl Pts',(5.04610371647275,-1.03126017046504,6.640625));
#32562=CARTESIAN_POINT('Ctrl Pts',(5.09366526266359,1.51694087528755,6.9140625));
#32563=CARTESIAN_POINT('Ctrl Pts',(3.89334793428042,3.85517018194508,7.1875));
#32564=CARTESIAN_POINT('Ctrl Pts',(1.66401832874098,5.39254335225655,7.4609375));
#32565=CARTESIAN_POINT('Ctrl Pts',(-1.10655649717025,5.70140348716183,7.73437499999999));
#32566=CARTESIAN_POINT('Ctrl Pts',(-3.76778215269101,4.63360702978987,8.0078125));
#32567=CARTESIAN_POINT('Ctrl Pts',(-5.65899445677288,2.37325046891981,8.28125));
#32568=CARTESIAN_POINT('Ctrl Pts',(-6.27308950292314,-0.59072056165688,
8.5546875));
#32569=CARTESIAN_POINT('Ctrl Pts',(-5.39055984190282,-3.56939135267172,
8.828125));
#32570=CARTESIAN_POINT('Ctrl Pts',(-3.14892433147632,-5.83395881494245,
9.10156249999999));
#32571=CARTESIAN_POINT('Ctrl Pts',(-0.0269941651234124,-6.79383570767807,
9.375));
#32572=CARTESIAN_POINT('Ctrl Pts',(3.25625963494257,-6.14929751664737,9.64843749999999));
#32573=CARTESIAN_POINT('Ctrl Pts',(5.90717602022873,-3.9795144383767,9.921875));
#32574=CARTESIAN_POINT('Ctrl Pts',(7.24915357717334,-0.741104090144106,
10.1953125));
#32575=CARTESIAN_POINT('Ctrl Pts',(6.89437699385751,2.82652617704715,10.46875));
#32576=CARTESIAN_POINT('Ctrl Pts',(4.85214544364602,5.8698051725334,10.7421875));
#32577=CARTESIAN_POINT('Ctrl Pts',(1.54426647303593,7.62518428271038,11.015625));
#32578=CARTESIAN_POINT('Ctrl Pts',(-2.28027404042269,7.61004816114384,11.2890625));
#32579=CARTESIAN_POINT('Ctrl Pts',(-5.71458753487403,5.75276305414747,11.5625));
#32580=CARTESIAN_POINT('Ctrl Pts',(-7.90892381685067,2.42735464211985,11.8359375));
#32581=CARTESIAN_POINT('Ctrl Pts',(-8.280487904502,-1.61956843656331,12.109375));
#32582=CARTESIAN_POINT('Ctrl Pts',(-6.66632390115336,-5.43598980597183,
12.3828125));
#32583=CARTESIAN_POINT('Ctrl Pts',(-3.37955924042675,-8.08843859127204,
12.65625));
#32584=CARTESIAN_POINT('Ctrl Pts',(0.848467586061227,-8.89003850095873,
12.9296875));
#32585=CARTESIAN_POINT('Ctrl Pts',(5.03032510682704,-7.57700176269046,13.203125));
#32586=CARTESIAN_POINT('Ctrl Pts',(8.15306896806033,-4.38851452128152,13.4765625));
#32587=CARTESIAN_POINT('Ctrl Pts',(9.42344702515047,-0.0269941685586242,
13.75));
#32588=CARTESIAN_POINT('Ctrl Pts',(8.46840766181913,4.49584983333495,14.0234375));
#32589=CARTESIAN_POINT('Ctrl Pts',(5.44044821239548,8.09361792642082,14.296875));
#32590=CARTESIAN_POINT('Ctrl Pts',(0.998851072840637,9.86610260310719,14.5703125));
#32591=CARTESIAN_POINT('Ctrl Pts',(-3.83283486415787,9.32382107321317,14.84375));
#32592=CARTESIAN_POINT('Ctrl Pts',(-7.90252221315964,6.52035320687432,15.1171875));
#32593=CARTESIAN_POINT('Ctrl Pts',(-10.2042683613299,2.05727819272983,15.390625));
#32594=CARTESIAN_POINT('Ctrl Pts',(-10.1264293031967,-3.04360991455306,
15.6640625));
#32595=CARTESIAN_POINT('Ctrl Pts',(-7.61217905231046,-7.57400353305939,
15.9375));
#32596=CARTESIAN_POINT('Ctrl Pts',(-3.19069051639217,-10.4253049589896,
16.2109375));
#32597=CARTESIAN_POINT('Ctrl Pts',(2.13258015658974,-10.859571982884,16.484375));
#32598=CARTESIAN_POINT('Ctrl Pts',(7.10419756851087,-8.69904094228735,16.7578125));
#32599=CARTESIAN_POINT('Ctrl Pts',(10.5178826720182,-4.38586792650576,17.03125));
#32600=CARTESIAN_POINT('Ctrl Pts',(11.506987524106,1.10621456668648,17.3046875));
#32601=CARTESIAN_POINT('Ctrl Pts',(9.76344367445795,6.49125888499182,17.578125));
#32602=CARTESIAN_POINT('Ctrl Pts',(5.62810470852332,10.4721791049393,17.8515625));
#32603=CARTESIAN_POINT('Ctrl Pts',(0.0269941874218459,12.0530583592068,
18.125));
#32604=CARTESIAN_POINT('Ctrl Pts',(-5.73544006773032,10.7875177817739,18.3984375));
#32605=CARTESIAN_POINT('Ctrl Pts',(-10.2800597580419,6.90138203286673,18.671875));
#32606=CARTESIAN_POINT('Ctrl Pts',(-12.4830517794477,1.25659796463401,18.9453125));
#32607=CARTESIAN_POINT('Ctrl Pts',(-11.7532648511587,-4.83914337048452,
19.21875));
#32608=CARTESIAN_POINT('Ctrl Pts',(-8.18856157315,-9.93523961480004,19.4921875));
#32609=CARTESIAN_POINT('Ctrl Pts',(-2.57028870635813,-12.7833517182835,
19.765625));
#32610=CARTESIAN_POINT('Ctrl Pts',(3.80694337685198,-12.6428118882295,20.0390625));
#32611=CARTESIAN_POINT('Ctrl Pts',(9.43342435418766,-9.47159216503061,20.3125));
#32612=CARTESIAN_POINT('Ctrl Pts',(12.9416764567355,-3.95403216061098,20.5859375));
#32613=CARTESIAN_POINT('Ctrl Pts',(13.4386753471291,2.64560341469982,20.859375));
#32614=CARTESIAN_POINT('Ctrl Pts',(10.731719416327,8.77238225818101,21.1328125));
#32615=CARTESIAN_POINT('Ctrl Pts',(5.39225375379758,12.9473728958347,21.40625));
#32616=CARTESIAN_POINT('Ctrl Pts',(-1.36411605698682,14.1238442145743,21.6796875));
#32617=CARTESIAN_POINT('Ctrl Pts',(-7.95188025078462,11.9500710288293,21.953125));
#32618=CARTESIAN_POINT('Ctrl Pts',(-12.791953880403,6.86731330268108,22.2265625));
#32619=CARTESIAN_POINT('Ctrl Pts',(-14.0510066394079,2.30770101502388,22.4088541666667));
#32620=CARTESIAN_POINT('Ctrl Pts',(-14.1036297108185,1.72719649817133E-14,
22.5));
#32621=CARTESIAN_POINT('Ctrl Pts',(-4.,0.,4.85040034982906));
#32622=CARTESIAN_POINT('Ctrl Pts',(-4.05262307141051,-0.654721101939438,
4.94154618316239));
#32623=CARTESIAN_POINT('Ctrl Pts',(-3.83034220978403,-2.01636569876658,
5.12383784982906));
#32624=CARTESIAN_POINT('Ctrl Pts',(-2.51853054589473,-3.72090195887707,
5.39727534982905));
#32625=CARTESIAN_POINT('Ctrl Pts',(-0.483390156018607,-4.63215288184746,
5.67071284982907));
#32626=CARTESIAN_POINT('Ctrl Pts',(1.82024146317888,-4.46499056561057,5.94415034982905));
#32627=CARTESIAN_POINT('Ctrl Pts',(3.83709775979154,-3.18393342683724,6.21758784982906));
#32628=CARTESIAN_POINT('Ctrl Pts',(5.0461260345829,-1.0312683628151,6.49102534982905));
#32629=CARTESIAN_POINT('Ctrl Pts',(5.09368654153737,1.51694929147494,6.76446284982906));
#32630=CARTESIAN_POINT('Ctrl Pts',(3.89336386627578,3.85518507450177,7.03790034982906));
#32631=CARTESIAN_POINT('Ctrl Pts',(1.66402479258124,5.39256527713564,7.31133784982906));
#32632=CARTESIAN_POINT('Ctrl Pts',(-1.10656084853258,5.70142522984817,7.58477534982906));
#32633=CARTESIAN_POINT('Ctrl Pts',(-3.76779638138169,4.63362447414178,7.85821284982905));
#32634=CARTESIAN_POINT('Ctrl Pts',(-5.65901515770697,2.37325898596484,8.13165034982906));
#32635=CARTESIAN_POINT('Ctrl Pts',(-6.27311180986061,-0.590722728563154,
8.40508784982905));
#32636=CARTESIAN_POINT('Ctrl Pts',(-5.39057847567184,-3.56940381917799,
8.67852534982906));
#32637=CARTESIAN_POINT('Ctrl Pts',(-3.14893489718495,-5.83397857329016,
8.95196284982906));
#32638=CARTESIAN_POINT('Ctrl Pts',(-0.0269941647942543,-6.79385812364079,
9.22540034982906));
#32639=CARTESIAN_POINT('Ctrl Pts',(3.25627019982838,-6.14931728059803,9.49883784982906));
#32640=CARTESIAN_POINT('Ctrl Pts',(5.90719465539629,-3.97952689087694,9.77227534982905));
#32641=CARTESIAN_POINT('Ctrl Pts',(7.24917588143762,-0.741106286459191,
10.0457128498291));
#32642=CARTESIAN_POINT('Ctrl Pts',(6.89439770007539,2.82653475360122,10.3191503498291));
#32643=CARTESIAN_POINT('Ctrl Pts',(4.85215966180167,5.86982249753558,10.5925878498291));
#32644=CARTESIAN_POINT('Ctrl Pts',(1.54427084544956,7.62520626423373,10.8660253498291));
#32645=CARTESIAN_POINT('Ctrl Pts',(-2.28028054635119,7.61006960833658,11.1394628498291));
#32646=CARTESIAN_POINT('Ctrl Pts',(-5.71460338271004,5.75277890197015,11.4129003498291));
#32647=CARTESIAN_POINT('Ctrl Pts',(-7.90894526401481,2.42736114805309,11.6863378498291));
#32648=CARTESIAN_POINT('Ctrl Pts',(-8.28050988608349,-1.61957280897544,
11.9597753498291));
#32649=CARTESIAN_POINT('Ctrl Pts',(-6.66634122603885,-5.43600402413594,
12.2332128498291));
#32650=CARTESIAN_POINT('Ctrl Pts',(-3.37956781721442,-8.08845929747025,
12.5066503498291));
#32651=CARTESIAN_POINT('Ctrl Pts',(0.848469782843532,-8.89006080526373,
12.7800878498291));
#32652=CARTESIAN_POINT('Ctrl Pts',(5.03033755839293,-7.57702039777591,13.0535253498291));
#32653=CARTESIAN_POINT('Ctrl Pts',(8.15308873387941,-4.38852508633184,13.3269628498291));
#32654=CARTESIAN_POINT('Ctrl Pts',(9.42346943737693,-0.0269941685586252,
13.6004003498291));
#32655=CARTESIAN_POINT('Ctrl Pts',(8.4684274276382,4.49586039838528,13.8738378498291));
#32656=CARTESIAN_POINT('Ctrl Pts',(5.44046066396137,8.09363656150627,14.1472753498291));
#32657=CARTESIAN_POINT('Ctrl Pts',(0.998853269622947,9.86612490741219,14.4207128498291));
#32658=CARTESIAN_POINT('Ctrl Pts',(-3.83284344094555,9.32384177941138,14.6941503498291));
#32659=CARTESIAN_POINT('Ctrl Pts',(-7.90253953804511,6.52036742503844,14.9675878498291));
#32660=CARTESIAN_POINT('Ctrl Pts',(-10.2042903429114,2.05728256514196,15.2410253498291));
#32661=CARTESIAN_POINT('Ctrl Pts',(-10.1264507503608,-3.04361642048629,
15.5144628498291));
#32662=CARTESIAN_POINT('Ctrl Pts',(-7.61219490014649,-7.57401938088208,
15.7879003498291));
#32663=CARTESIAN_POINT('Ctrl Pts',(-3.19069702232067,-10.4253264061823,
16.0613378498291));
#32664=CARTESIAN_POINT('Ctrl Pts',(2.13258452900337,-10.8595939644074,16.3347753498291));
#32665=CARTESIAN_POINT('Ctrl Pts',(7.10421178666652,-8.69905826728953,16.6082128498291));
#32666=CARTESIAN_POINT('Ctrl Pts',(10.5179033782361,-4.38587650305984,16.881650349829));
#32667=CARTESIAN_POINT('Ctrl Pts',(11.5070098283703,1.10621676300158,17.1550878498291));
#32668=CARTESIAN_POINT('Ctrl Pts',(9.76346230962549,6.49127133749205,17.428525349829));
#32669=CARTESIAN_POINT('Ctrl Pts',(5.62811527340914,10.47219886889,17.7019628498291));
#32670=CARTESIAN_POINT('Ctrl Pts',(0.0269941877509962,12.0530807751695,
17.975400349829));
#32671=CARTESIAN_POINT('Ctrl Pts',(-5.73545063343893,10.7875375401217,18.2488378498291));
#32672=CARTESIAN_POINT('Ctrl Pts',(-10.280078391811,6.901394499373,18.5222753498291));
#32673=CARTESIAN_POINT('Ctrl Pts',(-12.4830740863852,1.25660013154028,18.795712849829));
#32674=CARTESIAN_POINT('Ctrl Pts',(-11.7532855520928,-4.83915188752954,
19.0691503498291));
#32675=CARTESIAN_POINT('Ctrl Pts',(-8.18857580184066,-9.93525705915197,
19.342587849829));
#32676=CARTESIAN_POINT('Ctrl Pts',(-2.57029305772047,-12.7833734609698,
19.6160253498291));
#32677=CARTESIAN_POINT('Ctrl Pts',(3.80694984069224,-12.6428338131086,19.889462849829));
#32678=CARTESIAN_POINT('Ctrl Pts',(9.43344028618301,-9.4716070575873,20.1629003498291));
#32679=CARTESIAN_POINT('Ctrl Pts',(12.9416977356093,-3.95404057679838,20.4363378498291));
#32680=CARTESIAN_POINT('Ctrl Pts',(13.4386976652392,2.64561160704987,20.7097753498291));
#32681=CARTESIAN_POINT('Ctrl Pts',(10.7317360682354,8.77238883738826,20.9832128498291));
#32682=CARTESIAN_POINT('Ctrl Pts',(5.39226367667676,12.9474088812546,21.2566503498291));
#32683=CARTESIAN_POINT('Ctrl Pts',(-1.36412095011418,14.1238359162802,21.5300878498291));
#32684=CARTESIAN_POINT('Ctrl Pts',(-7.95188724769903,11.9501515161596,21.8035253498291));
#32685=CARTESIAN_POINT('Ctrl Pts',(-12.7919852791712,6.86719192859605,22.0769628498291));
#32686=CARTESIAN_POINT('Ctrl Pts',(-14.0510066394079,2.30792364746544,22.2592545164957));
#32687=CARTESIAN_POINT('Ctrl Pts',(-14.1036297108185,1.72719649817133E-14,
22.3504003498291));
#32688=CARTESIAN_POINT('Ctrl Pts',(-3.85687988625421,0.,4.552272366273));
#32689=CARTESIAN_POINT('Ctrl Pts',(-3.90950295766472,-0.631009216832047,
4.64341819960633));
#32690=CARTESIAN_POINT('Ctrl Pts',(-3.69889172862669,-1.94629413136597,
4.825709866273));
#32691=CARTESIAN_POINT('Ctrl Pts',(-2.43574645059125,-3.59690784386268,
5.099147366273));
#32692=CARTESIAN_POINT('Ctrl Pts',(-0.468778083864464,-4.48388629988577,
5.372584866273));
#32693=CARTESIAN_POINT('Ctrl Pts',(1.76320931622579,-4.32728810641048,5.646022366273));
#32694=CARTESIAN_POINT('Ctrl Pts',(3.72190061988142,-3.08940290516982,5.91945986627299));
#32695=CARTESIAN_POINT('Ctrl Pts',(4.89996324172001,-1.00218972289062,6.19289736627299));
#32696=CARTESIAN_POINT('Ctrl Pts',(4.95107819396225,1.47368683855714,6.466334866273));
#32697=CARTESIAN_POINT('Ctrl Pts',(3.78798665921667,3.7498093182653,6.73977236627299));
#32698=CARTESIAN_POINT('Ctrl Pts',(1.62076500665406,5.24995596983545,7.013209866273));
#32699=CARTESIAN_POINT('Ctrl Pts',(-1.07748742465841,5.55526338525199,7.28664736627299));
#32700=CARTESIAN_POINT('Ctrl Pts',(-3.67325548745206,4.51842592346714,7.560084866273));
#32701=CARTESIAN_POINT('Ctrl Pts',(-5.52133341543936,2.31622941794741,7.833522366273));
#32702=CARTESIAN_POINT('Ctrl Pts',(-6.12480374971085,-0.576115700560577,
8.10695986627299));
#32703=CARTESIAN_POINT('Ctrl Pts',(-5.26666817492343,-3.48660958131966,
8.380397366273));
#32704=CARTESIAN_POINT('Ctrl Pts',(-3.07868468871711,-5.70254968975686,
8.65383486627299));
#32705=CARTESIAN_POINT('Ctrl Pts',(-0.0269941654050771,-6.64483246405232,
8.92727236627299));
#32706=CARTESIAN_POINT('Ctrl Pts',(3.18601999288746,-6.0178883894713,9.20070986627299));
#32707=CARTESIAN_POINT('Ctrl Pts',(5.7832843520526,-3.89673267200036,9.47414736627299));
#32708=CARTESIAN_POINT('Ctrl Pts',(7.10086782624852,-0.726499218600172,
9.74758486627298));
#32709=CARTESIAN_POINT('Ctrl Pts',(6.75671594800256,2.76950510493386,10.021022366273));
#32710=CARTESIAN_POINT('Ctrl Pts',(4.7576187874221,5.75462410861027,10.294459866273));
#32711=CARTESIAN_POINT('Ctrl Pts',(1.51519738251008,7.47904409595247,10.567897366273));
#32712=CARTESIAN_POINT('Ctrl Pts',(-2.23702068232002,7.46746094842322,10.841334866273));
#32713=CARTESIAN_POINT('Ctrl Pts',(-5.60922633182713,5.64740185110466,11.114772366273));
#32714=CARTESIAN_POINT('Ctrl Pts',(-7.76633660413988,2.38410128401679,11.388209866273));
#32715=CARTESIAN_POINT('Ctrl Pts',(-8.13434771772362,-1.59049934604057,
11.661647366273));
#32716=CARTESIAN_POINT('Ctrl Pts',(-6.5511428372716,-5.34146314973975,11.935084866273));
#32717=CARTESIAN_POINT('Ctrl Pts',(-3.32253816823053,-7.95077754543437,
12.208522366273));
#32718=CARTESIAN_POINT('Ctrl Pts',(0.833862714351334,-8.74175274999886,
12.481959866273));
#32719=CARTESIAN_POINT('Ctrl Pts',(4.94754334078261,-7.45311009458468,12.755397366273));
#32720=CARTESIAN_POINT('Ctrl Pts',(8.0216598402205,-4.31827487908557,13.028834866273));
#32721=CARTESIAN_POINT('Ctrl Pts',(9.27444378285203,-0.0269941685586267,
13.302272366273));
#32722=CARTESIAN_POINT('Ctrl Pts',(8.3369985339793,4.42561019113901,13.575709866273));
#32723=CARTESIAN_POINT('Ctrl Pts',(5.35766644635105,7.96972625831503,13.849147366273));
#32724=CARTESIAN_POINT('Ctrl Pts',(0.98424620113075,9.71781685214733,14.122584866273));
#32725=CARTESIAN_POINT('Ctrl Pts',(-3.77581379196166,9.1861600273755,14.396022366273));
#32726=CARTESIAN_POINT('Ctrl Pts',(-7.78734114927787,6.42582655064225,14.669459866273));
#32727=CARTESIAN_POINT('Ctrl Pts',(-10.0581281745515,2.02820910220709,14.942897366273));
#32728=CARTESIAN_POINT('Ctrl Pts',(-9.98384209048586,-3.00035655645,15.216334866273));
#32729=CARTESIAN_POINT('Ctrl Pts',(-7.50681784926357,-7.46864233001658,
15.489772366273));
#32730=CARTESIAN_POINT('Ctrl Pts',(-3.1474371582895,-10.282717746269,15.763209866273));
#32731=CARTESIAN_POINT('Ctrl Pts',(2.10351106606389,-10.7134317961261,16.036647366273));
#32732=CARTESIAN_POINT('Ctrl Pts',(7.00967091228695,-8.58385987836422,16.310084866273));
#32733=CARTESIAN_POINT('Ctrl Pts',(10.3802216261632,-4.32884685439248,16.583522366273));
#32734=CARTESIAN_POINT('Ctrl Pts',(11.3587017731812,1.09160969514256,16.856959866273));
#32735=CARTESIAN_POINT('Ctrl Pts',(9.63955200628181,6.40847711861546,17.130397366273));
#32736=CARTESIAN_POINT('Ctrl Pts',(5.55786506646821,10.3407699777633,17.403834866273));
#32737=CARTESIAN_POINT('Ctrl Pts',(0.0269941871401723,11.904055115581,17.677272366273));
#32738=CARTESIAN_POINT('Ctrl Pts',(-5.66520042497109,10.6561086565884,17.950709866273));
#32739=CARTESIAN_POINT('Ctrl Pts',(-10.1561680910626,6.81860026151465,18.224147366273));
#32740=CARTESIAN_POINT('Ctrl Pts',(-12.3347660262354,1.24199310353771,18.497584866273));
#32741=CARTESIAN_POINT('Ctrl Pts',(-11.6156038098252,-4.78212231951214,
18.771022366273));
#32742=CARTESIAN_POINT('Ctrl Pts',(-8.09403490791103,-9.82005850847731,
19.044459866273));
#32743=CARTESIAN_POINT('Ctrl Pts',(-2.5412196338463,-12.6372116163736,19.317897366273));
#32744=CARTESIAN_POINT('Ctrl Pts',(3.76369005476507,-12.5002245058084,19.591334866273));
#32745=CARTESIAN_POINT('Ctrl Pts',(9.3280630791239,-9.36623130135084,19.864772366273));
#32746=CARTESIAN_POINT('Ctrl Pts',(12.7990893880342,-3.91077812388057,20.138209866273));
#32747=CARTESIAN_POINT('Ctrl Pts',(13.2925348723763,2.6165329671254,20.411647366273));
#32748=CARTESIAN_POINT('Ctrl Pts',(10.6165389283253,8.67785831572082,20.685084866273));
#32749=CARTESIAN_POINT('Ctrl Pts',(5.33523152972366,12.8097064220545,20.958522366273));
#32750=CARTESIAN_POINT('Ctrl Pts',(-1.34950887796003,13.9755693343185,21.231959866273));
#32751=CARTESIAN_POINT('Ctrl Pts',(-7.86910315239555,11.8261574011453,21.505397366273));
#32752=CARTESIAN_POINT('Ctrl Pts',(-12.6605347980139,6.79712036119543,21.778834866273));
#32753=CARTESIAN_POINT('Ctrl Pts',(-13.9078865256621,2.28421176235806,21.9611265329396));
#32754=CARTESIAN_POINT('Ctrl Pts',(-13.9605095970727,1.70966933925209E-14,
22.052272366273));
#32755=CARTESIAN_POINT('Ctrl Pts',(-3.37285122334358,0.,4.44236151564151));
#32756=CARTESIAN_POINT('Ctrl Pts',(-3.42547429475409,-0.551880177973973,
4.53350734897485));
#32757=CARTESIAN_POINT('Ctrl Pts',(-3.25447952827565,-1.70873378422384,
4.71579901564151));
#32758=CARTESIAN_POINT('Ctrl Pts',(-2.15580613893563,-3.17794748381105,
4.98923651564151));
#32759=CARTESIAN_POINT('Ctrl Pts',(-0.419383803872583,-3.98241275177538,
5.26267401564151));
#32760=CARTESIAN_POINT('Ctrl Pts',(1.57037543627681,-3.86175379164219,5.53611151564151));
#32761=CARTESIAN_POINT('Ctrl Pts',(3.33238633949545,-2.76973447564646,5.80954901564151));
#32762=CARTESIAN_POINT('Ctrl Pts',(4.40575097261005,-0.903885637798203,
6.08298651564152));
#32763=CARTESIAN_POINT('Ctrl Pts',(4.46888200381864,1.32741452063332,6.35642401564151));
#32764=CARTESIAN_POINT('Ctrl Pts',(3.43167970686377,3.39350230505294,6.62986151564152));
#32765=CARTESIAN_POINT('Ctrl Pts',(1.47449237810634,4.76775962120238,6.90329901564151));
#32766=CARTESIAN_POINT('Ctrl Pts',(-0.979182623933988,5.06105157319051,
7.17673651564152));
#32767=CARTESIAN_POINT('Ctrl Pts',(-3.35358853628449,4.12891065901958,7.45017401564151));
#32768=CARTESIAN_POINT('Ctrl Pts',(-5.05579611984973,2.12339754137519,7.72361151564152));
#32769=CARTESIAN_POINT('Ctrl Pts',(-5.62333618663063,-0.52672545107936,
7.99704901564151));
#32770=CARTESIAN_POINT('Ctrl Pts',(-4.84769567278908,-3.20666110712353,
8.27048651564151));
#32771=CARTESIAN_POINT('Ctrl Pts',(-2.84115072577757,-5.25815490214821,
8.54392401564152));
#32772=CARTESIAN_POINT('Ctrl Pts',(-0.026994165897813,-6.14093851856364,
8.81736151564151));
#32773=CARTESIAN_POINT('Ctrl Pts',(2.94848603117964,-5.57349360295854,9.09079901564151));
#32774=CARTESIAN_POINT('Ctrl Pts',(5.36431184782471,-3.6167841950648,9.36423651564152));
#32775=CARTESIAN_POINT('Ctrl Pts',(6.59940026716997,-0.677108974870978,
9.63767401564151));
#32776=CARTESIAN_POINT('Ctrl Pts',(6.29117864450327,2.57667324000092,9.91111151564152));
#32777=CARTESIAN_POINT('Ctrl Pts',(4.43795185202518,5.36510882081929,10.1845490156415));
#32778=CARTESIAN_POINT('Ctrl Pts',(1.41689255027245,6.98483233060473,10.4579865156415));
#32779=CARTESIAN_POINT('Ctrl Pts',(-2.09074799076738,6.98526450636028,10.7314240156415));
#32780=CARTESIAN_POINT('Ctrl Pts',(-5.25291950545845,5.29109502473119,11.0048615156415));
#32781=CARTESIAN_POINT('Ctrl Pts',(-7.28414016207024,2.23782859246943,11.2782990156415));
#32782=CARTESIAN_POINT('Ctrl Pts',(-7.64013595238779,-1.49219451381135,
11.5517365156415));
#32783=CARTESIAN_POINT('Ctrl Pts',(-6.16162754945752,-5.02179621432706,
11.8251740156415));
#32784=CARTESIAN_POINT('Ctrl Pts',(-3.12970630334341,-7.48524024196608,
12.0986115156415));
#32785=CARTESIAN_POINT('Ctrl Pts',(0.784472470713589,-8.2402851908586,12.3720490156415));
#32786=CARTESIAN_POINT('Ctrl Pts',(4.66759486366428,-7.03413759048006,12.6454865156415));
#32787=CARTESIAN_POINT('Ctrl Pts',(7.57726505407319,-4.08074091713133,12.9189240156415));
#32788=CARTESIAN_POINT('Ctrl Pts',(8.77054983663259,-0.0269941685586301,
13.1923615156415));
#32789=CARTESIAN_POINT('Ctrl Pts',(7.89260374783199,4.18807622918479,13.4657990156415));
#32790=CARTESIAN_POINT('Ctrl Pts',(5.07771796923272,7.55075375421039,13.7392365156415));
#32791=CARTESIAN_POINT('Ctrl Pts',(0.934855957493001,9.21634929300708,14.0126740156415));
#32792=CARTESIAN_POINT('Ctrl Pts',(-3.58298192707453,8.72062272390719,14.2861115156415));
#32793=CARTESIAN_POINT('Ctrl Pts',(-7.3978258614638,6.10615961522957,14.5595490156415));
#32794=CARTESIAN_POINT('Ctrl Pts',(-9.5639164092157,1.92990426997787,14.8329865156415));
#32795=CARTESIAN_POINT('Ctrl Pts',(-9.50164564841623,-2.85408386490263,
15.1064240156415));
#32796=CARTESIAN_POINT('Ctrl Pts',(-7.15051102289489,-7.11233550364311,
15.3798615156415));
#32797=CARTESIAN_POINT('Ctrl Pts',(-3.00116446673686,-9.800521304206,15.6532990156415));
#32798=CARTESIAN_POINT('Ctrl Pts',(2.00520623382626,-10.2192200307783,15.9267365156415));
#32799=CARTESIAN_POINT('Ctrl Pts',(6.69000397689003,-8.19434459057323,16.2001740156415));
#32800=CARTESIAN_POINT('Ctrl Pts',(9.91468432266393,-4.13601498945954,16.4736115156415));
#32801=CARTESIAN_POINT('Ctrl Pts',(10.8572342141026,1.04221945141336,16.7470490156415));
#32802=CARTESIAN_POINT('Ctrl Pts',(9.22057950205391,6.12852864167992,17.0204865156415));
#32803=CARTESIAN_POINT('Ctrl Pts',(5.3203311047604,9.8963751912505,17.2939240156415));
#32804=CARTESIAN_POINT('Ctrl Pts',(0.0269941866474298,11.4001611700923,
17.5673615156415));
#32805=CARTESIAN_POINT('Ctrl Pts',(-5.42766646203154,10.2117138689797,17.8407990156415));
#32806=CARTESIAN_POINT('Ctrl Pts',(-9.73719558892825,6.53865178731853,18.1142365156415));
#32807=CARTESIAN_POINT('Ctrl Pts',(-11.8332984631552,1.19260285405648,18.3876740156415));
#32808=CARTESIAN_POINT('Ctrl Pts',(-11.1500665142356,-4.5892904429399,18.6611115156415));
#32809=CARTESIAN_POINT('Ctrl Pts',(-7.77436795674347,-9.43054324402977,
18.9345490156415));
#32810=CARTESIAN_POINT('Ctrl Pts',(-2.44291483312187,-12.1429998043121,
19.2079865156415));
#32811=CARTESIAN_POINT('Ctrl Pts',(3.61741742621734,-12.0180281571754,19.4814240156415));
#32812=CARTESIAN_POINT('Ctrl Pts',(8.97175612677101,-9.00992428813846,19.7548615156415));
#32813=CARTESIAN_POINT('Ctrl Pts',(12.3168931978906,-3.76450580595676,20.0282990156415));
#32814=CARTESIAN_POINT('Ctrl Pts',(12.7983226032663,2.51822888203298,20.3017365156415));
#32815=CARTESIAN_POINT('Ctrl Pts',(10.2270246479393,8.35818988619747,20.5751740156415));
#32816=CARTESIAN_POINT('Ctrl Pts',(5.14239764977468,12.3441721072862,20.8486115156415));
#32817=CARTESIAN_POINT('Ctrl Pts',(-1.30011459796815,13.4740957862082,21.1220490156415));
#32818=CARTESIAN_POINT('Ctrl Pts',(-7.58916284073994,11.4071970410936,21.3954865156415));
#32819=CARTESIAN_POINT('Ctrl Pts',(-12.2161225976628,6.55956001405331,21.6689240156415));
#32820=CARTESIAN_POINT('Ctrl Pts',(-13.4238578627515,2.20508272349997,21.8512156823082));
#32821=CARTESIAN_POINT('Ctrl Pts',(-13.476480934162,1.65039292397919E-14,
21.9423615156415));
#32822=CARTESIAN_POINT('Ctrl Pts',(-2.98371143764262,0.,4.75150716662327));
#32823=CARTESIAN_POINT('Ctrl Pts',(-3.03633450905313,-0.488281981545911,
4.84265299995661));
#32824=CARTESIAN_POINT('Ctrl Pts',(-2.89719239750444,-1.51773468502555,
5.02494466662328));
#32825=CARTESIAN_POINT('Ctrl Pts',(-1.93074584541099,-2.84112667747553,
5.29838216662328));
#32826=CARTESIAN_POINT('Ctrl Pts',(-0.37967317259002,-3.57924728657917,
5.57181966662327));
#32827=CARTESIAN_POINT('Ctrl Pts',(1.415345489773,-3.48748570044128,5.84525716662328));
#32828=CARTESIAN_POINT('Ctrl Pts',(3.0192337330702,-2.51273432159306,6.11869466662327));
#32829=CARTESIAN_POINT('Ctrl Pts',(4.0084258174915,-0.824853742020043,6.39213216662327));
#32830=CARTESIAN_POINT('Ctrl Pts',(4.0812172121738,1.20981809279467,6.66556966662328));
#32831=CARTESIAN_POINT('Ctrl Pts',(3.14522441136627,3.10704687470915,6.93900716662327));
#32832=CARTESIAN_POINT('Ctrl Pts',(1.35689553916174,4.38009475553567,7.21244466662328));
#32833=CARTESIAN_POINT('Ctrl Pts',(-0.900149835328617,4.66372673795749,
7.48588216662327));
#32834=CARTESIAN_POINT('Ctrl Pts',(-3.09659020305971,3.81575732694958,7.75931966662327));
#32835=CARTESIAN_POINT('Ctrl Pts',(-4.68152436880527,1.96836908930344,8.03275716662328));
#32836=CARTESIAN_POINT('Ctrl Pts',(-5.22017806292132,-0.487017834823588,
8.30619466662326));
#32837=CARTESIAN_POINT('Ctrl Pts',(-4.51085999202353,-2.98159470334547,
8.57963216662328));
#32838=CARTESIAN_POINT('Ctrl Pts',(-2.65018374428007,-4.90088080835761,
8.85306966662327));
#32839=CARTESIAN_POINT('Ctrl Pts',(-0.0269941662667494,-5.73582968895438,
9.12650716662328));
#32840=CARTESIAN_POINT('Ctrl Pts',(2.7575190506044,-5.2162195105121,9.39994466662327));
#32841=CARTESIAN_POINT('Ctrl Pts',(5.02747616549161,-3.39171778792666,9.67338216662326));
#32842=CARTESIAN_POINT('Ctrl Pts',(6.19624214645689,-0.637401365670468,
9.94681966662328));
#32843=CARTESIAN_POINT('Ctrl Pts',(5.91690688753647,2.42164480220557,10.2202571666233));
#32844=CARTESIAN_POINT('Ctrl Pts',(4.18095353060857,5.05195546011693,10.4936946666233));
#32845=CARTESIAN_POINT('Ctrl Pts',(1.33785973807176,6.58750755266943,10.7671321666233));
#32846=CARTESIAN_POINT('Ctrl Pts',(-1.97315110464824,6.59759952609516,11.0405696666233));
#32847=CARTESIAN_POINT('Ctrl Pts',(-4.96646430429082,5.00463982355861,11.3140071666233));
#32848=CARTESIAN_POINT('Ctrl Pts',(-6.89647518179741,2.12023170635493,11.5874446666233));
#32849=CARTESIAN_POINT('Ctrl Pts',(-7.24281117446687,-1.41316170161731,
11.8608821666233));
#32850=CARTESIAN_POINT('Ctrl Pts',(-5.84847418872696,-4.76479789289847,
12.1343196666233));
#32851=CARTESIAN_POINT('Ctrl Pts',(-2.9746778656042,-7.11096848502258,12.4077571666233));
#32852=CARTESIAN_POINT('Ctrl Pts',(0.744764861625225,-7.83712707009927,
12.6811946666233));
#32853=CARTESIAN_POINT('Ctrl Pts',(4.44252845630195,-6.69730190823927,12.9546321666233));
#32854=CARTESIAN_POINT('Ctrl Pts',(7.21999096207501,-3.88977393637157,13.2280696666233));
#32855=CARTESIAN_POINT('Ctrl Pts',(8.36544100612696,-0.0269941685586301,
13.5015071666233));
#32856=CARTESIAN_POINT('Ctrl Pts',(7.53532965583381,3.99710924842502,13.7749446666233));
#32857=CARTESIAN_POINT('Ctrl Pts',(4.85265156187039,7.21391807196961,14.0483821666233));
#32858=CARTESIAN_POINT('Ctrl Pts',(0.895148348404636,8.81319117224774,14.3218196666233));
#32859=CARTESIAN_POINT('Ctrl Pts',(-3.42795348933533,8.34635096696369,14.5952571666233));
#32860=CARTESIAN_POINT('Ctrl Pts',(-7.08467250073323,5.84916129380098,14.8686946666232));
#32861=CARTESIAN_POINT('Ctrl Pts',(-9.16659163129478,1.85087145778383,15.1421321666233));
#32862=CARTESIAN_POINT('Ctrl Pts',(-9.11398066814341,-2.73648697878813,
15.4155696666233));
#32863=CARTESIAN_POINT('Ctrl Pts',(-6.86405582172724,-6.82588030247055,
15.6890071666233));
#32864=CARTESIAN_POINT('Ctrl Pts',(-2.88356758061773,-9.41285632394088,
15.9624446666233));
#32865=CARTESIAN_POINT('Ctrl Pts',(1.92617342162557,-9.82189525284306,16.2358821666233));
#32866=CARTESIAN_POINT('Ctrl Pts',(6.43300565547342,-7.88119122987088,16.5093196666233));
#32867=CARTESIAN_POINT('Ctrl Pts',(9.54041256569715,-3.98098655166418,16.7827571666233));
#32868=CARTESIAN_POINT('Ctrl Pts',(10.4540760933895,1.00251184221285,17.0561946666233));
#32869=CARTESIAN_POINT('Ctrl Pts',(8.88374381972081,5.90346223454177,17.3296321666233));
#32870=CARTESIAN_POINT('Ctrl Pts',(5.12936412418515,9.53910109880408,17.6030696666233));
#32871=CARTESIAN_POINT('Ctrl Pts',(0.0269941862784956,10.9950523404831,
17.8765071666233));
#32872=CARTESIAN_POINT('Ctrl Pts',(-5.23669948053405,9.85443977518913,18.1499446666233));
#32873=CARTESIAN_POINT('Ctrl Pts',(-9.40035990816268,6.31358538354047,18.4233821666233));
#32874=CARTESIAN_POINT('Ctrl Pts',(-11.4301403394459,1.15289523780071,18.6968196666233));
#32875=CARTESIAN_POINT('Ctrl Pts',(-10.7757947631911,-4.43426199086815,
18.9702571666232));
#32876=CARTESIAN_POINT('Ctrl Pts',(-7.51736962351869,-9.11738991195976,
19.2436946666233));
#32877=CARTESIAN_POINT('Ctrl Pts',(-2.3638820445165,-11.7456749690791,19.5171321666233));
#32878=CARTESIAN_POINT('Ctrl Pts',(3.49982058727274,-11.6303632915086,19.7905696666233));
#32879=CARTESIAN_POINT('Ctrl Pts',(8.68530083127351,-8.72346885779468,20.0640071666233));
#32880=CARTESIAN_POINT('Ctrl Pts',(11.9292284062458,-3.64690937811811,20.3374446666233));
#32881=CARTESIAN_POINT('Ctrl Pts',(12.4009974481478,2.43919698625482,20.6108821666233));
#32882=CARTESIAN_POINT('Ctrl Pts',(9.91387204151406,8.10118973214408,20.8843196666233));
#32883=CARTESIAN_POINT('Ctrl Pts',(4.98736770327087,11.9699040160853,21.1577571666233));
#32884=CARTESIAN_POINT('Ctrl Pts',(-1.26040396668559,13.070930321012,21.4311946666233));
#32885=CARTESIAN_POINT('Ctrl Pts',(-7.36410254721529,11.0703762347581,21.7046321666233));
#32886=CARTESIAN_POINT('Ctrl Pts',(-11.8588354668916,6.36856091485502,21.9780696666233));
#32887=CARTESIAN_POINT('Ctrl Pts',(-13.0347180770506,2.14148452707192,22.1603613332899));
#32888=CARTESIAN_POINT('Ctrl Pts',(-13.0873411484611,1.60273704468123E-14,
22.2515071666233));
#32889=CARTESIAN_POINT('Ctrl Pts',(-2.98483377249807,0.,5.2480277325673));
#32890=CARTESIAN_POINT('Ctrl Pts',(-3.03745684390858,-0.488306844967222,
5.33917356590063));
#32891=CARTESIAN_POINT('Ctrl Pts',(-2.89820050196772,-1.51837199860867,
5.5214652325673));
#32892=CARTESIAN_POINT('Ctrl Pts',(-1.93138996818963,-2.84204079236029,
5.7949027325673));
#32893=CARTESIAN_POINT('Ctrl Pts',(-0.379784218761552,-3.58041598369861,
6.0683402325673));
#32894=CARTESIAN_POINT('Ctrl Pts',(1.41578555107907,-3.48853951372869,6.3417777325673));
#32895=CARTESIAN_POINT('Ctrl Pts',(3.02012505022879,-2.51347086100097,6.6152152325673));
#32896=CARTESIAN_POINT('Ctrl Pts',(4.00955586475944,-0.825075846581511,
6.88865273256729));
#32897=CARTESIAN_POINT('Ctrl Pts',(4.08232013773346,1.21015126356688,7.1620902325673));
#32898=CARTESIAN_POINT('Ctrl Pts',(3.14603924239308,3.10786244643203,7.43552773256729));
#32899=CARTESIAN_POINT('Ctrl Pts',(1.35723010161685,4.38119722121209,7.7089652325673));
#32900=CARTESIAN_POINT('Ctrl Pts',(-0.900374678086592,4.66485719413016,
7.9824027325673));
#32901=CARTESIAN_POINT('Ctrl Pts',(-3.09732128911458,3.81664808180835,8.2558402325673));
#32902=CARTESIAN_POINT('Ctrl Pts',(-4.68258907853753,1.96881014756007,8.52927773256729));
#32903=CARTESIAN_POINT('Ctrl Pts',(-5.22132494126317,-0.487130813963699,
8.8027152325673));
#32904=CARTESIAN_POINT('Ctrl Pts',(-4.511818203042,-2.98223494820395,9.0761527325673));
#32905=CARTESIAN_POINT('Ctrl Pts',(-2.65072699530537,-4.90189716574,9.3495902325673));
#32906=CARTESIAN_POINT('Ctrl Pts',(-0.0269941665001183,-5.73698211576155,
9.6230277325673));
#32907=CARTESIAN_POINT('Ctrl Pts',(2.75806230221306,-5.21723586390009,9.89646523256729));
#32908=CARTESIAN_POINT('Ctrl Pts',(5.02843437551854,-3.39235804277017,10.1699027325673));
#32909=CARTESIAN_POINT('Ctrl Pts',(6.19738902669399,-0.63751432384474,10.4433402325673));
#32910=CARTESIAN_POINT('Ctrl Pts',(5.91797159352262,2.4220858180376,10.7167777325673));
#32911=CARTESIAN_POINT('Ctrl Pts',(4.18168462413262,5.05284630006133,10.9902152325673));
#32912=CARTESIAN_POINT('Ctrl Pts',(1.33808456590467,6.58863783857275,11.2636527325673));
#32913=CARTESIAN_POINT('Ctrl Pts',(-1.97348563726341,6.59870233231904,11.5370902325673));
#32914=CARTESIAN_POINT('Ctrl Pts',(-4.96727919498537,5.00545471426267,11.8105277325673));
#32915=CARTESIAN_POINT('Ctrl Pts',(-6.89757798804165,2.12056623896671,12.0839652325673));
#32916=CARTESIAN_POINT('Ctrl Pts',(-7.24394146032877,-1.41338652945127,
12.3574027325673));
#32917=CARTESIAN_POINT('Ctrl Pts',(-5.84936502875454,-4.76552898641652,
12.6308402325673));
#32918=CARTESIAN_POINT('Ctrl Pts',(-2.97511888126971,-7.11203319102266,
12.9042777325673));
#32919=CARTESIAN_POINT('Ctrl Pts',(0.744877819466415,-7.83827395030751,
13.1777152325673));
#32920=CARTESIAN_POINT('Ctrl Pts',(4.44316871181156,-6.6982601183244,13.4511527325673));
#32921=CARTESIAN_POINT('Ctrl Pts',(7.22100731413099,-3.8903171878636,13.7245902325673));
#32922=CARTESIAN_POINT('Ctrl Pts',(8.36659343559775,-0.0269941685586248,
13.9980277325673));
#32923=CARTESIAN_POINT('Ctrl Pts',(7.53634600788979,3.99765249991704,14.2714652325673));
#32924=CARTESIAN_POINT('Ctrl Pts',(4.85329181738001,7.21487628205475,14.5449027325673));
#32925=CARTESIAN_POINT('Ctrl Pts',(0.895261306245823,8.81433805245597,14.8183402325673));
#32926=CARTESIAN_POINT('Ctrl Pts',(-3.42839450500082,8.34741567296378,15.0917777325673));
#32927=CARTESIAN_POINT('Ctrl Pts',(-7.08556334076082,5.84989238731903,15.3652152325673));
#32928=CARTESIAN_POINT('Ctrl Pts',(-9.16772191715667,1.85109628561778,15.6386527325673));
#32929=CARTESIAN_POINT('Ctrl Pts',(-9.11508347438764,-2.73682151139992,
15.9120902325673));
#32930=CARTESIAN_POINT('Ctrl Pts',(-6.8648707124218,-6.8266951931746,16.1855277325673));
#32931=CARTESIAN_POINT('Ctrl Pts',(-2.88390211323289,-9.41395913016475,
16.4589652325673));
#32932=CARTESIAN_POINT('Ctrl Pts',(1.92639824945848,-9.82302553874637,16.7324027325673));
#32933=CARTESIAN_POINT('Ctrl Pts',(6.43373674899746,-7.88208206981527,17.0058402325673));
#32934=CARTESIAN_POINT('Ctrl Pts',(9.54147727168329,-3.98142756749621,17.2792777325673));
#32935=CARTESIAN_POINT('Ctrl Pts',(10.4552229736266,1.00262480038713,17.5527152325673));
#32936=CARTESIAN_POINT('Ctrl Pts',(8.88470202974774,5.90410248938528,17.8261527325673));
#32937=CARTESIAN_POINT('Ctrl Pts',(5.12990737579382,9.54011745219205,18.0995902325673));
#32938=CARTESIAN_POINT('Ctrl Pts',(0.0269941860451295,10.9962047672903,
18.3730277325673));
#32939=CARTESIAN_POINT('Ctrl Pts',(-5.23724273155935,9.8554561325715,18.6464652325673));
#32940=CARTESIAN_POINT('Ctrl Pts',(-9.40131811918114,6.31422562839895,18.9199027325673));
#32941=CARTESIAN_POINT('Ctrl Pts',(-11.4312872177877,1.15300821694082,19.1933402325673));
#32942=CARTESIAN_POINT('Ctrl Pts',(-10.7768594729234,-4.43470304912478,
19.4667777325673));
#32943=CARTESIAN_POINT('Ctrl Pts',(-7.51810070957355,-9.11828066681853,
19.7402152325673));
#32944=CARTESIAN_POINT('Ctrl Pts',(-2.36410688727448,-11.7468054252518,
20.0136527325673));
#32945=CARTESIAN_POINT('Ctrl Pts',(3.50015514972786,-11.631465757185,20.2870902325673));
#32946=CARTESIAN_POINT('Ctrl Pts',(8.6861156623003,-8.72428442951756,20.5605277325673));
#32947=CARTESIAN_POINT('Ctrl Pts',(11.9303313318055,-3.64724254889032,20.8339652325673));
#32948=CARTESIAN_POINT('Ctrl Pts',(12.4021274954157,2.43941909081629,21.1074027325673));
#32949=CARTESIAN_POINT('Ctrl Pts',(9.91476335867265,8.10192627155198,21.3808402325673));
#32950=CARTESIAN_POINT('Ctrl Pts',(4.98780776457694,11.9709578293727,21.6542777325673));
#32951=CARTESIAN_POINT('Ctrl Pts',(-1.26051501285712,13.0720990181314,21.9277152325673));
#32952=CARTESIAN_POINT('Ctrl Pts',(-7.36474666999395,11.0712903496429,22.2011527325673));
#32953=CARTESIAN_POINT('Ctrl Pts',(-11.8598435713549,6.36919822843813,22.4745902325673));
#32954=CARTESIAN_POINT('Ctrl Pts',(-13.035840411906,2.14150939049322,22.656881899234));
#32955=CARTESIAN_POINT('Ctrl Pts',(-13.0884634833165,1.60287449106006E-14,
22.7480277325673));
#32956=CARTESIAN_POINT('Ctrl Pts',(-3.37236445914593,0.,5.55880118622959));
#32957=CARTESIAN_POINT('Ctrl Pts',(-3.42498753055644,-0.551891116017674,
5.64994701956293));
#32958=CARTESIAN_POINT('Ctrl Pts',(-3.25404537003884,-1.70844553497412,
5.83223868622959));
#32959=CARTESIAN_POINT('Ctrl Pts',(-2.15552746120626,-3.17755887888968,
6.10567618622959));
#32960=CARTESIAN_POINT('Ctrl Pts',(-0.419336119804426,-3.98190507031525,
6.37911368622959));
#32961=CARTESIAN_POINT('Ctrl Pts',(1.57018554686087,-3.86130025668376,6.65255118622959));
#32962=CARTESIAN_POINT('Ctrl Pts',(3.33200139390039,-2.76941567544733,6.92598868622959));
#32963=CARTESIAN_POINT('Ctrl Pts',(4.40526304098788,-0.903790108850918,
7.19942618622959));
#32964=CARTESIAN_POINT('Ctrl Pts',(4.46840573366961,1.32727084336026,7.47286368622959));
#32965=CARTESIAN_POINT('Ctrl Pts',(3.43132786358059,3.39315003911043,7.74630118622959));
#32966=CARTESIAN_POINT('Ctrl Pts',(1.47434790676726,4.76728361353632,8.01973868622959));
#32967=CARTESIAN_POINT('Ctrl Pts',(-0.979085532660522,5.06056340808148,
8.29317618622959));
#32968=CARTESIAN_POINT('Ctrl Pts',(-3.353272847575,4.12852603461372,8.56661368622959));
#32969=CARTESIAN_POINT('Ctrl Pts',(-5.05533636777526,2.1232070824127,8.84005118622959));
#32970=CARTESIAN_POINT('Ctrl Pts',(-5.62284095416809,-0.526676662681731,
9.11348868622958));
#32971=CARTESIAN_POINT('Ctrl Pts',(-4.84728190823904,-3.20638464492345,
9.3869261862296));
#32972=CARTESIAN_POINT('Ctrl Pts',(-2.84091614500297,-5.25771602884916,
9.66036368622959));
#32973=CARTESIAN_POINT('Ctrl Pts',(-0.026994165764487,-6.14044089033148,
9.93380118622959));
#32974=CARTESIAN_POINT('Ctrl Pts',(2.94825145007176,-5.57305473193853,10.2072386862296));
#32975=CARTESIAN_POINT('Ctrl Pts',(5.36389808384115,-3.61650772716763,10.4806761862296));
#32976=CARTESIAN_POINT('Ctrl Pts',(6.59890503362463,-0.67706019843569,10.7541136862296));
#32977=CARTESIAN_POINT('Ctrl Pts',(6.29071889456904,2.57648280524436,11.0275511862296));
#32978=CARTESIAN_POINT('Ctrl Pts',(4.43763615904838,5.36472414786668,11.3009886862296));
#32979=CARTESIAN_POINT('Ctrl Pts',(1.41679546752599,6.98434426264517,11.5744261862296));
#32980=CARTESIAN_POINT('Ctrl Pts',(-2.09060353647649,6.98478830439027,11.8478636862296));
#32981=CARTESIAN_POINT('Ctrl Pts',(-5.25256762808581,5.29074314735314,12.1213011862296));
#32982=CARTESIAN_POINT('Ctrl Pts',(-7.28366396008863,2.23768413818047,12.3947386862296));
#32983=CARTESIAN_POINT('Ctrl Pts',(-7.63964788445187,-1.49209743106429,
12.6681761862296));
#32984=CARTESIAN_POINT('Ctrl Pts',(-6.16124287645745,-5.02148052135369,
12.9416136862296));
#32985=CARTESIAN_POINT('Ctrl Pts',(-3.12951586868186,-7.48478049202387,
13.2150511862296));
#32986=CARTESIAN_POINT('Ctrl Pts',(0.784423694468346,-8.23978995732977,
13.4884886862296));
#32987=CARTESIAN_POINT('Ctrl Pts',(4.66731839538705,-7.03372382646324,13.7619261862296));
#32988=CARTESIAN_POINT('Ctrl Pts',(7.57682618381319,-4.08050633609009,14.0353636862296));
#32989=CARTESIAN_POINT('Ctrl Pts',(8.77005220688066,-0.0269941685586276,
14.3088011862296));
#32990=CARTESIAN_POINT('Ctrl Pts',(7.89216487757199,4.18784164814354,14.5822386862296));
#32991=CARTESIAN_POINT('Ctrl Pts',(5.07744150095549,7.55033999019357,14.8556761862296));
#32992=CARTESIAN_POINT('Ctrl Pts',(0.934807181247757,9.21585405947824,15.1291136862296));
#32993=CARTESIAN_POINT('Ctrl Pts',(-3.58279149241298,8.72016297396498,15.4025511862296));
#32994=CARTESIAN_POINT('Ctrl Pts',(-7.39744118846373,6.1058439222562,15.6759886862296));
#32995=CARTESIAN_POINT('Ctrl Pts',(-9.56342834127977,1.9298071872308,15.9494261862296));
#32996=CARTESIAN_POINT('Ctrl Pts',(-9.50116944643463,-2.85393941061368,
16.2228636862296));
#32997=CARTESIAN_POINT('Ctrl Pts',(-7.15015914552224,-7.11198362626506,
16.4963011862296));
#32998=CARTESIAN_POINT('Ctrl Pts',(-3.00102001244598,-9.800045102236,16.7697386862296));
#32999=CARTESIAN_POINT('Ctrl Pts',(2.00510915107979,-10.2187319628188,17.0431761862296));
#33000=CARTESIAN_POINT('Ctrl Pts',(6.68968828391324,-8.19395991762063,17.3166136862296));
#33001=CARTESIAN_POINT('Ctrl Pts',(9.91422457272969,-4.13582455470297,17.5900511862296));
#33002=CARTESIAN_POINT('Ctrl Pts',(10.8567389805573,1.04217067497807,17.8634886862296));
#33003=CARTESIAN_POINT('Ctrl Pts',(9.22016573807034,6.12825217378274,18.1369261862296));
#33004=CARTESIAN_POINT('Ctrl Pts',(5.32009652365252,9.89593632023051,18.4103636862296));
#33005=CARTESIAN_POINT('Ctrl Pts',(0.0269941867807571,11.3996635418602,
18.6838011862296));
#33006=CARTESIAN_POINT('Ctrl Pts',(-5.42743188125695,10.2112749956807,18.9572386862296));
#33007=CARTESIAN_POINT('Ctrl Pts',(-9.73678182437819,6.53837532511846,19.2306761862296));
#33008=CARTESIAN_POINT('Ctrl Pts',(-11.8328032306926,1.19255406565886,19.5041136862296));
#33009=CARTESIAN_POINT('Ctrl Pts',(-11.1496067621611,-4.58909998397742,
19.7775511862296));
#33010=CARTESIAN_POINT('Ctrl Pts',(-7.77405226803399,-9.43015861962389,
20.0509886862296));
#33011=CARTESIAN_POINT('Ctrl Pts',(-2.44281774184841,-12.1425116392031,
20.3244261862296));
#33012=CARTESIAN_POINT('Ctrl Pts',(3.61727295487827,-12.0175521495093,20.5978636862296));
#33013=CARTESIAN_POINT('Ctrl Pts',(8.97140428348781,-9.00957202219596,20.8713011862296));
#33014=CARTESIAN_POINT('Ctrl Pts',(12.3164169277416,-3.7643621286837,21.1447386862296));
#33015=CARTESIAN_POINT('Ctrl Pts',(12.7978346716442,2.5181333530857,21.4181761862296));
#33016=CARTESIAN_POINT('Ctrl Pts',(10.2266397023443,8.35787108599834,21.6916136862296));
#33017=CARTESIAN_POINT('Ctrl Pts',(5.14220776035875,12.3437185723278,21.9650511862296));
#33018=CARTESIAN_POINT('Ctrl Pts',(-1.3000669139,13.473588104748,22.2384886862296));
#33019=CARTESIAN_POINT('Ctrl Pts',(-7.58888416301056,11.4068084361723,22.5119261862296));
#33020=CARTESIAN_POINT('Ctrl Pts',(-12.215688439426,6.55927176480358,22.7853636862296));
#33021=CARTESIAN_POINT('Ctrl Pts',(-13.4233710985539,2.20509366154368,22.9676553528962));
#33022=CARTESIAN_POINT('Ctrl Pts',(-13.4759941699644,1.65033331255753E-14,
23.0588011862296));
#33023=CARTESIAN_POINT('Ctrl Pts',(-3.85691369956507,0.,5.4468630354969));
#33024=CARTESIAN_POINT('Ctrl Pts',(-3.90953677097559,-0.630966749404783,
5.53800886883023));
#33025=CARTESIAN_POINT('Ctrl Pts',(-3.69891600544325,-1.9463368927696,5.7203005354969));
#33026=CARTESIAN_POINT('Ctrl Pts',(-2.43576449828385,-3.59691976012222,
5.99373803549689));
#33027=CARTESIAN_POINT('Ctrl Pts',(-0.468780479590593,-4.48392312081373,
6.2671755354969));
#33028=CARTESIAN_POINT('Ctrl Pts',(1.76322064804953,-4.32731286998429,6.5406130354969));
#33029=CARTESIAN_POINT('Ctrl Pts',(3.72192424077144,-3.08942381824181,6.81405053549689));
#33030=CARTESIAN_POINT('Ctrl Pts',(4.899992955087,-1.00219482411329,7.08748803549689));
#33031=CARTESIAN_POINT('Ctrl Pts',(4.95110729194826,1.47369524249325,7.36092553549689));
#33032=CARTESIAN_POINT('Ctrl Pts',(3.78800811550593,3.7498309986416,7.63436303549691));
#33033=CARTESIAN_POINT('Ctrl Pts',(1.62077383149999,5.24998492856633,7.90780053549689));
#33034=CARTESIAN_POINT('Ctrl Pts',(-1.07749335397341,5.55529322263726,8.18123803549691));
#33035=CARTESIAN_POINT('Ctrl Pts',(-3.67327475134075,4.51844937359048,8.4546755354969));
#33036=CARTESIAN_POINT('Ctrl Pts',(-5.52136147425963,2.31624105270174,8.7281130354969));
#33037=CARTESIAN_POINT('Ctrl Pts',(-6.12483397232732,-0.576118683725451,
9.0015505354969));
#33038=CARTESIAN_POINT('Ctrl Pts',(-5.26669342645748,-3.48662645044473,
9.2749880354969));
#33039=CARTESIAN_POINT('Ctrl Pts',(-3.07869900462109,-5.70257647480552,
9.5484255354969));
#33040=CARTESIAN_POINT('Ctrl Pts',(-0.0269941654760016,-6.64486283266747,
9.8218630354969));
#33041=CARTESIAN_POINT('Ctrl Pts',(3.18603430896873,-6.01791517331201,10.0953005354969));
#33042=CARTESIAN_POINT('Ctrl Pts',(5.7833096032853,-3.89674954414503,10.3687380354969));
#33043=CARTESIAN_POINT('Ctrl Pts',(7.10089804944101,-0.726502195424679,
10.6421755354969));
#33044=CARTESIAN_POINT('Ctrl Pts',(6.7567440056843,2.76951672685838,10.9156130354969));
#33045=CARTESIAN_POINT('Ctrl Pts',(4.75763805358084,5.75464758446472,11.1890505354969));
#33046=CARTESIAN_POINT('Ctrl Pts',(1.51520330728903,7.47907388184584,11.4624880354969));
#33047=CARTESIAN_POINT('Ctrl Pts',(-2.23702949809695,7.46749001014054,11.7359255354969));
#33048=CARTESIAN_POINT('Ctrl Pts',(-5.6092478062507,5.64742332553111,12.0093630354969));
#33049=CARTESIAN_POINT('Ctrl Pts',(-7.76636566586335,2.38411009979269,12.2828005354969));
#33050=CARTESIAN_POINT('Ctrl Pts',(-8.13437750360446,-1.59050527081984,
12.5562380354969));
#33051=CARTESIAN_POINT('Ctrl Pts',(-6.55116631315121,-5.34148241589666,
12.8296755354969));
#33052=CARTESIAN_POINT('Ctrl Pts',(-3.32254979010469,-7.95080560312036,
13.1031130354969));
#33053=CARTESIAN_POINT('Ctrl Pts',(0.833865691075113,-8.74178297318257,
13.3765505354969));
#33054=CARTESIAN_POINT('Ctrl Pts',(4.94756021312872,-7.45313534583507,13.6499880354969));
#33055=CARTESIAN_POINT('Ctrl Pts',(8.02168662365838,-4.3182891951314,13.9234255354969));
#33056=CARTESIAN_POINT('Ctrl Pts',(9.27447415227271,-0.0269941685586289,
14.1968630354969));
#33057=CARTESIAN_POINT('Ctrl Pts',(8.33702531741718,4.42562450718485,14.4703005354969));
#33058=CARTESIAN_POINT('Ctrl Pts',(5.35768331869717,7.96975150956542,14.7437380354969));
#33059=CARTESIAN_POINT('Ctrl Pts',(0.984249177854521,9.71784707533104,15.0171755354969));
#33060=CARTESIAN_POINT('Ctrl Pts',(-3.77582541383581,9.18618808506149,15.2906130354969));
#33061=CARTESIAN_POINT('Ctrl Pts',(-7.78736462515749,6.42584581679915,15.5640505354969));
#33062=CARTESIAN_POINT('Ctrl Pts',(-10.0581579604324,2.02821502698636,15.8374880354969));
#33063=CARTESIAN_POINT('Ctrl Pts',(-9.98387115220935,-3.0003653722259,16.1109255354969));
#33064=CARTESIAN_POINT('Ctrl Pts',(-7.50683932368714,-7.46866380444304,
16.3843630354969));
#33065=CARTESIAN_POINT('Ctrl Pts',(-3.14744597406643,-10.2827468079863,
16.6578005354969));
#33066=CARTESIAN_POINT('Ctrl Pts',(2.10351699084284,-10.7134615820195,16.9312380354969));
#33067=CARTESIAN_POINT('Ctrl Pts',(7.00969017844569,-8.58388335421866,17.2046755354969));
#33068=CARTESIAN_POINT('Ctrl Pts',(10.380249683845,-4.328858476317,17.4781130354969));
#33069=CARTESIAN_POINT('Ctrl Pts',(11.3587319963737,1.09161267196707,17.7515505354969));
#33070=CARTESIAN_POINT('Ctrl Pts',(9.63957725751449,6.40849399076014,18.0249880354969));
#33071=CARTESIAN_POINT('Ctrl Pts',(5.55787938254949,10.340796761604,18.2984255354969));
#33072=CARTESIAN_POINT('Ctrl Pts',(0.0269941870692434,11.9040854841962,
18.5718630354969));
#33073=CARTESIAN_POINT('Ctrl Pts',(-5.66521474087506,10.656135441637,18.8453005354969));
#33074=CARTESIAN_POINT('Ctrl Pts',(-10.1561933425966,6.81861713063972,19.1187380354969));
#33075=CARTESIAN_POINT('Ctrl Pts',(-12.3347962488519,1.24199608670258,19.3921755354969));
#33076=CARTESIAN_POINT('Ctrl Pts',(-11.6156318686455,-4.78213395426646,
19.6656130354969));
#33077=CARTESIAN_POINT('Ctrl Pts',(-8.09405417179972,-9.82008195860066,
19.9390505354969));
#33078=CARTESIAN_POINT('Ctrl Pts',(-2.5412255631613,-12.6372414537589,20.2124880354969));
#33079=CARTESIAN_POINT('Ctrl Pts',(3.76369887961099,-12.5002534645393,20.4859255354969));
#33080=CARTESIAN_POINT('Ctrl Pts',(9.32808453541316,-9.36625298172713,20.7593630354969));
#33081=CARTESIAN_POINT('Ctrl Pts',(12.7991184860202,-3.91078652781669,21.0328005354969));
#33082=CARTESIAN_POINT('Ctrl Pts',(13.2925645857433,2.61653806834808,21.3062380354969));
#33083=CARTESIAN_POINT('Ctrl Pts',(10.6165625492153,8.67787922879281,21.5796755354969));
#33084=CARTESIAN_POINT('Ctrl Pts',(5.33524286154741,12.8097311856283,21.8531130354969));
#33085=CARTESIAN_POINT('Ctrl Pts',(-1.34951127368616,13.9756061552465,22.1265505354969));
#33086=CARTESIAN_POINT('Ctrl Pts',(-7.86912120008815,11.8261693174048,22.3999880354969));
#33087=CARTESIAN_POINT('Ctrl Pts',(-12.6605590748304,6.79716312259906,22.6734255354969));
#33088=CARTESIAN_POINT('Ctrl Pts',(-13.907920338973,2.28416929493079,22.8557172021636));
#33089=CARTESIAN_POINT('Ctrl Pts',(-13.9605434103835,1.70967348018838E-14,
22.9468630354969));
#33090=CARTESIAN_POINT('Ctrl Pts',(-4.,0.,5.14959965017094));
#33091=CARTESIAN_POINT('Ctrl Pts',(-4.05262307141051,-0.654750131429363,
5.24074548350428));
#33092=CARTESIAN_POINT('Ctrl Pts',(-3.8303463039323,-2.01634987255655,5.42303715017094));
#33093=CARTESIAN_POINT('Ctrl Pts',(-2.51853145823641,-3.72091245378127,
5.69647465017095));
#33094=CARTESIAN_POINT('Ctrl Pts',(-0.483390794043284,-4.63215179981628,
5.96991215017094));
#33095=CARTESIAN_POINT('Ctrl Pts',(1.82024275704298,-4.46499525782153,6.24334965017094));
#33096=CARTESIAN_POINT('Ctrl Pts',(3.83709993106723,-3.18393428471325,6.51678715017094));
#33097=CARTESIAN_POINT('Ctrl Pts',(5.04612894468598,-1.03126943103203,6.79022465017094));
#33098=CARTESIAN_POINT('Ctrl Pts',(5.09368931613234,1.51695038887847,7.06366215017095));
#33099=CARTESIAN_POINT('Ctrl Pts',(3.89336594368056,3.85518701637207,7.33709965017094));
#33100=CARTESIAN_POINT('Ctrl Pts',(1.66402563541432,5.39256813596453,7.61053715017095));
#33101=CARTESIAN_POINT('Ctrl Pts',(-1.10656141591542,5.70142806492059,7.88397465017094));
#33102=CARTESIAN_POINT('Ctrl Pts',(-3.76779823668917,4.63362674874576,8.15741215017094));
#33103=CARTESIAN_POINT('Ctrl Pts',(-5.65901785694323,2.3732600965194,8.43084965017094));
#33104=CARTESIAN_POINT('Ctrl Pts',(-6.27311471850686,-0.590723011110406,
8.70428715017094));
#33105=CARTESIAN_POINT('Ctrl Pts',(-5.3905809053663,-3.5694054447107,8.97772465017095));
#33106=CARTESIAN_POINT('Ctrl Pts',(-3.14893627486886,-5.8339811496207,9.25116215017094));
#33107=CARTESIAN_POINT('Ctrl Pts',(-0.0269941647513346,-6.79386104650306,
9.52459965017095));
#33108=CARTESIAN_POINT('Ctrl Pts',(3.256271577405,-6.14931985765915,9.79803715017094));
#33109=CARTESIAN_POINT('Ctrl Pts',(5.90719708527311,-3.97952851458338,10.0714746501709));
#33110=CARTESIAN_POINT('Ctrl Pts',(7.24917878973531,-0.741106572841118,
10.3449121501709));
#33111=CARTESIAN_POINT('Ctrl Pts',(6.89440040000061,2.82653587191529,10.6183496501709));
#33112=CARTESIAN_POINT('Ctrl Pts',(4.85216151573545,5.86982475657732,10.8917871501709));
#33113=CARTESIAN_POINT('Ctrl Pts',(1.54427141557733,7.62520913044859,11.1652246501709));
#33114=CARTESIAN_POINT('Ctrl Pts',(-2.28028139467223,7.61007240487899,11.4386621501709));
#33115=CARTESIAN_POINT('Ctrl Pts',(-5.71460544914113,5.75278096839949,11.7120996501709));
#33116=CARTESIAN_POINT('Ctrl Pts',(-7.9089480605535,2.42736199637475,11.9855371501709));
#33117=CARTESIAN_POINT('Ctrl Pts',(-8.28051275230592,-1.61957337910302,
12.258974650171));
#33118=CARTESIAN_POINT('Ctrl Pts',(-6.66634348506537,-5.43600587807083,
12.5324121501709));
#33119=CARTESIAN_POINT('Ctrl Pts',(-3.37956893555893,-8.0884619973929,12.8058496501709));
#33120=CARTESIAN_POINT('Ctrl Pts',(0.848470069286372,-8.89006371356673,
13.0792871501709));
#33121=CARTESIAN_POINT('Ctrl Pts',(5.03033918197755,-7.57702282764202,13.3527246501709));
#33122=CARTESIAN_POINT('Ctrl Pts',(8.15309131118414,-4.38852646392991,13.6261621501709));
#33123=CARTESIAN_POINT('Ctrl Pts',(9.42347235975202,-0.0269941685586307,
13.8995996501709));
#33124=CARTESIAN_POINT('Ctrl Pts',(8.46843000494294,4.49586177598336,14.1730371501709));
#33125=CARTESIAN_POINT('Ctrl Pts',(5.44046228754599,8.09363899137236,14.446474650171));
#33126=CARTESIAN_POINT('Ctrl Pts',(0.998853556065788,9.86612781571521,14.7199121501709));
#33127=CARTESIAN_POINT('Ctrl Pts',(-3.83284455929006,9.32384447933402,14.993349650171));
#33128=CARTESIAN_POINT('Ctrl Pts',(-7.90254179707164,6.52036927897334,15.2667871501709));
#33129=CARTESIAN_POINT('Ctrl Pts',(-10.2042932091338,2.05728313526953,15.540224650171));
#33130=CARTESIAN_POINT('Ctrl Pts',(-10.1264535468995,-3.04361726880795,
15.8136621501709));
#33131=CARTESIAN_POINT('Ctrl Pts',(-7.61219696657756,-7.57402144731142,
16.087099650171));
#33132=CARTESIAN_POINT('Ctrl Pts',(-3.19069787064171,-10.4253292027247,
16.3605371501709));
#33133=CARTESIAN_POINT('Ctrl Pts',(2.13258509913113,-10.8595968306222,16.6339746501709));
#33134=CARTESIAN_POINT('Ctrl Pts',(7.10421364060031,-8.69906052633126,16.9074121501709));
#33135=CARTESIAN_POINT('Ctrl Pts',(10.5179060781613,-4.3858776213739,17.1808496501709));
#33136=CARTESIAN_POINT('Ctrl Pts',(11.5070127366679,1.1062170493835,17.4542871501709));
#33137=CARTESIAN_POINT('Ctrl Pts',(9.76346473950231,6.4912729611985,17.7277246501709));
#33138=CARTESIAN_POINT('Ctrl Pts',(5.62811665098576,10.4722014459511,18.0011621501709));
#33139=CARTESIAN_POINT('Ctrl Pts',(0.0269941877939141,12.0530836980318,
18.2745996501709));
#33140=CARTESIAN_POINT('Ctrl Pts',(-5.73545201112284,10.7875401164522,18.5480371501709));
#33141=CARTESIAN_POINT('Ctrl Pts',(-10.2800808215054,6.90139612490571,18.8214746501709));
#33142=CARTESIAN_POINT('Ctrl Pts',(-12.4830769950314,1.25660041408754,19.0949121501709));
#33143=CARTESIAN_POINT('Ctrl Pts',(-11.7532882513291,-4.83915299808411,
19.368349650171));
#33144=CARTESIAN_POINT('Ctrl Pts',(-8.18857765714814,-9.93525933375593,
19.6417871501709));
#33145=CARTESIAN_POINT('Ctrl Pts',(-2.57029362510331,-12.7833762960422,
19.915224650171));
#33146=CARTESIAN_POINT('Ctrl Pts',(3.80695068352532,-12.6428366719375,20.1886621501709));
#33147=CARTESIAN_POINT('Ctrl Pts',(9.43344236358779,-9.4716089994576,20.462099650171));
#33148=CARTESIAN_POINT('Ctrl Pts',(12.9417005102043,-3.95404167420191,20.7355371501709));
#33149=CARTESIAN_POINT('Ctrl Pts',(13.4387005753423,2.6456126752668,21.008974650171));
#33150=CARTESIAN_POINT('Ctrl Pts',(10.7317382395111,8.77238969526427,21.2824121501709));
#33151=CARTESIAN_POINT('Ctrl Pts',(5.39226497054085,12.9474135734656,21.555849650171));
#33152=CARTESIAN_POINT('Ctrl Pts',(-1.36412158813886,14.1238348342491,21.8292871501709));
#33153=CARTESIAN_POINT('Ctrl Pts',(-7.9518881600407,11.9501620110638,22.102724650171));
#33154=CARTESIAN_POINT('Ctrl Pts',(-12.7919893733195,6.86717610238603,22.3761621501709));
#33155=CARTESIAN_POINT('Ctrl Pts',(-14.0510066394079,2.30795267695537,22.5584538168376));
#33156=CARTESIAN_POINT('Ctrl Pts',(-14.1036297108185,1.72719649817133E-14,
22.6495996501709));
#33157=CARTESIAN_POINT('Ctrl Pts',(-4.,0.,5.));
#33158=CARTESIAN_POINT('Ctrl Pts',(-4.05262307141051,-0.654498469497874,
5.09114583333333));
#33159=CARTESIAN_POINT('Ctrl Pts',(-3.83031081101585,-2.0164870728516,5.2734375));
#33160=CARTESIAN_POINT('Ctrl Pts',(-2.51852354898032,-3.7208214715467,5.546875));
#33161=CARTESIAN_POINT('Ctrl Pts',(-0.483385262891241,-4.63216118014149,
5.82031249999999));
#33162=CARTESIAN_POINT('Ctrl Pts',(1.8202315402997,-4.46495458019068,6.09375000000001));
#33163=CARTESIAN_POINT('Ctrl Pts',(3.83708110788313,-3.18392684763,6.36718749999999));
#33164=CARTESIAN_POINT('Ctrl Pts',(5.04610371647275,-1.03126017046504,6.640625));
#33165=CARTESIAN_POINT('Ctrl Pts',(5.09366526266359,1.51694087528755,6.9140625));
#33166=CARTESIAN_POINT('Ctrl Pts',(3.89334793428042,3.85517018194508,7.1875));
#33167=CARTESIAN_POINT('Ctrl Pts',(1.66401832874098,5.39254335225655,7.4609375));
#33168=CARTESIAN_POINT('Ctrl Pts',(-1.10655649717025,5.70140348716183,7.73437499999999));
#33169=CARTESIAN_POINT('Ctrl Pts',(-3.76778215269101,4.63360702978987,8.0078125));
#33170=CARTESIAN_POINT('Ctrl Pts',(-5.65899445677288,2.37325046891981,8.28125));
#33171=CARTESIAN_POINT('Ctrl Pts',(-6.27308950292314,-0.59072056165688,
8.5546875));
#33172=CARTESIAN_POINT('Ctrl Pts',(-5.39055984190282,-3.56939135267172,
8.828125));
#33173=CARTESIAN_POINT('Ctrl Pts',(-3.14892433147632,-5.83395881494245,
9.10156249999999));
#33174=CARTESIAN_POINT('Ctrl Pts',(-0.0269941651234124,-6.79383570767807,
9.375));
#33175=CARTESIAN_POINT('Ctrl Pts',(3.25625963494257,-6.14929751664737,9.64843749999999));
#33176=CARTESIAN_POINT('Ctrl Pts',(5.90717602022873,-3.9795144383767,9.921875));
#33177=CARTESIAN_POINT('Ctrl Pts',(7.24915357717334,-0.741104090144106,
10.1953125));
#33178=CARTESIAN_POINT('Ctrl Pts',(6.89437699385751,2.82652617704715,10.46875));
#33179=CARTESIAN_POINT('Ctrl Pts',(4.85214544364602,5.8698051725334,10.7421875));
#33180=CARTESIAN_POINT('Ctrl Pts',(1.54426647303593,7.62518428271038,11.015625));
#33181=CARTESIAN_POINT('Ctrl Pts',(-2.28027404042269,7.61004816114384,11.2890625));
#33182=CARTESIAN_POINT('Ctrl Pts',(-5.71458753487403,5.75276305414747,11.5625));
#33183=CARTESIAN_POINT('Ctrl Pts',(-7.90892381685067,2.42735464211985,11.8359375));
#33184=CARTESIAN_POINT('Ctrl Pts',(-8.280487904502,-1.61956843656331,12.109375));
#33185=CARTESIAN_POINT('Ctrl Pts',(-6.66632390115336,-5.43598980597183,
12.3828125));
#33186=CARTESIAN_POINT('Ctrl Pts',(-3.37955924042675,-8.08843859127204,
12.65625));
#33187=CARTESIAN_POINT('Ctrl Pts',(0.848467586061227,-8.89003850095873,
12.9296875));
#33188=CARTESIAN_POINT('Ctrl Pts',(5.03032510682704,-7.57700176269046,13.203125));
#33189=CARTESIAN_POINT('Ctrl Pts',(8.15306896806033,-4.38851452128152,13.4765625));
#33190=CARTESIAN_POINT('Ctrl Pts',(9.42344702515047,-0.0269941685586242,
13.75));
#33191=CARTESIAN_POINT('Ctrl Pts',(8.46840766181913,4.49584983333495,14.0234375));
#33192=CARTESIAN_POINT('Ctrl Pts',(5.44044821239548,8.09361792642082,14.296875));
#33193=CARTESIAN_POINT('Ctrl Pts',(0.998851072840637,9.86610260310719,14.5703125));
#33194=CARTESIAN_POINT('Ctrl Pts',(-3.83283486415787,9.32382107321317,14.84375));
#33195=CARTESIAN_POINT('Ctrl Pts',(-7.90252221315964,6.52035320687432,15.1171875));
#33196=CARTESIAN_POINT('Ctrl Pts',(-10.2042683613299,2.05727819272983,15.390625));
#33197=CARTESIAN_POINT('Ctrl Pts',(-10.1264293031967,-3.04360991455306,
15.6640625));
#33198=CARTESIAN_POINT('Ctrl Pts',(-7.61217905231046,-7.57400353305939,
15.9375));
#33199=CARTESIAN_POINT('Ctrl Pts',(-3.19069051639217,-10.4253049589896,
16.2109375));
#33200=CARTESIAN_POINT('Ctrl Pts',(2.13258015658974,-10.859571982884,16.484375));
#33201=CARTESIAN_POINT('Ctrl Pts',(7.10419756851087,-8.69904094228735,16.7578125));
#33202=CARTESIAN_POINT('Ctrl Pts',(10.5178826720182,-4.38586792650576,17.03125));
#33203=CARTESIAN_POINT('Ctrl Pts',(11.506987524106,1.10621456668648,17.3046875));
#33204=CARTESIAN_POINT('Ctrl Pts',(9.76344367445795,6.49125888499182,17.578125));
#33205=CARTESIAN_POINT('Ctrl Pts',(5.62810470852332,10.4721791049393,17.8515625));
#33206=CARTESIAN_POINT('Ctrl Pts',(0.0269941874218459,12.0530583592068,
18.125));
#33207=CARTESIAN_POINT('Ctrl Pts',(-5.73544006773032,10.7875177817739,18.3984375));
#33208=CARTESIAN_POINT('Ctrl Pts',(-10.2800597580419,6.90138203286673,18.671875));
#33209=CARTESIAN_POINT('Ctrl Pts',(-12.4830517794477,1.25659796463401,18.9453125));
#33210=CARTESIAN_POINT('Ctrl Pts',(-11.7532648511587,-4.83914337048452,
19.21875));
#33211=CARTESIAN_POINT('Ctrl Pts',(-8.18856157315,-9.93523961480004,19.4921875));
#33212=CARTESIAN_POINT('Ctrl Pts',(-2.57028870635813,-12.7833517182835,
19.765625));
#33213=CARTESIAN_POINT('Ctrl Pts',(3.80694337685198,-12.6428118882295,20.0390625));
#33214=CARTESIAN_POINT('Ctrl Pts',(9.43342435418766,-9.47159216503061,20.3125));
#33215=CARTESIAN_POINT('Ctrl Pts',(12.9416764567355,-3.95403216061098,20.5859375));
#33216=CARTESIAN_POINT('Ctrl Pts',(13.4386753471291,2.64560341469982,20.859375));
#33217=CARTESIAN_POINT('Ctrl Pts',(10.731719416327,8.77238225818101,21.1328125));
#33218=CARTESIAN_POINT('Ctrl Pts',(5.39225375379758,12.9473728958347,21.40625));
#33219=CARTESIAN_POINT('Ctrl Pts',(-1.36411605698682,14.1238442145743,21.6796875));
#33220=CARTESIAN_POINT('Ctrl Pts',(-7.95188025078462,11.9500710288293,21.953125));
#33221=CARTESIAN_POINT('Ctrl Pts',(-12.791953880403,6.86731330268108,22.2265625));
#33222=CARTESIAN_POINT('Ctrl Pts',(-14.0510066394079,2.30770101502388,22.4088541666667));
#33223=CARTESIAN_POINT('Ctrl Pts',(-14.1036297108185,1.72719649817133E-14,
22.5));
#33224=CARTESIAN_POINT('',(-4.,0.,5.));
#33225=CARTESIAN_POINT('Ctrl Pts',(-4.,0.,5.));
#33226=CARTESIAN_POINT('Ctrl Pts',(-4.,0.,4.99313090468968));
#33227=CARTESIAN_POINT('Ctrl Pts',(-3.99984912800787,-7.31607958282715E-11,
4.98626238012908));
#33228=CARTESIAN_POINT('Ctrl Pts',(-3.99665140600643,-7.31607958282715E-11,
4.91292688069719));
#33229=CARTESIAN_POINT('Ctrl Pts',(-3.97984082732515,-7.31754050494978E-11,
4.84714403296737));
#33230=CARTESIAN_POINT('Ctrl Pts',(-3.92504698362485,-7.31754050494978E-11,
4.73052812084229));
#33231=CARTESIAN_POINT('Ctrl Pts',(-3.88837099959727,-7.3182295505018E-11,
4.6787736262658));
#33232=CARTESIAN_POINT('Ctrl Pts',(-3.79060884070887,-7.3182295505018E-11,
4.58558772856037));
#33233=CARTESIAN_POINT('Ctrl Pts',(-3.73360882255537,-7.3222926866944E-11,
4.5543170883066));
#33234=CARTESIAN_POINT('Ctrl Pts',(-3.62062886145855,-7.3222926866944E-11,
4.51106951053573));
#33235=CARTESIAN_POINT('Ctrl Pts',(-3.55498900661372,-7.33122171618315E-11,
4.49929281521309));
#33236=CARTESIAN_POINT('Ctrl Pts',(-3.42514177672713,-7.33122171618315E-11,
4.50114804373618));
#33237=CARTESIAN_POINT('Ctrl Pts',(-3.36273596280029,-7.34200079994916E-11,
4.51448293356282));
#33238=CARTESIAN_POINT('Ctrl Pts',(-3.24209738586254,-7.34200079994916E-11,
4.56698211807808));
#33239=CARTESIAN_POINT('Ctrl Pts',(-3.18605812158766,-7.35736907335013E-11,
4.60594883894128));
#33240=CARTESIAN_POINT('Ctrl Pts',(-3.10316353487479,-7.35736907335013E-11,
4.69113814536176));
#33241=CARTESIAN_POINT('Ctrl Pts',(-3.06529482757558,-7.36685445914362E-11,
4.7410844949528));
#33242=CARTESIAN_POINT('Ctrl Pts',(-3.01284056824797,-7.36685445914362E-11,
4.86734749872617));
#33243=CARTESIAN_POINT('Ctrl Pts',(-3.00033399986338,-3.99897980483117E-9,
4.93376452822198));
#33244=CARTESIAN_POINT('Ctrl Pts',(-3.00057394652585,-3.99897980483117E-9,
5.06669212380191));
#33245=CARTESIAN_POINT('Ctrl Pts',(-3.01349577924023,-4.99214209269255E-11,
5.13354317521189));
#33246=CARTESIAN_POINT('Ctrl Pts',(-3.06714330922775,-4.99214209269255E-11,
5.26131316399762));
#33247=CARTESIAN_POINT('Ctrl Pts',(-3.10587060337886,-4.98538136835682E-11,
5.31167639465468));
#33248=CARTESIAN_POINT('Ctrl Pts',(-3.18918143195268,-4.98538136835682E-11,
5.39664026609539));
#33249=CARTESIAN_POINT('Ctrl Pts',(-3.24557401970868,-4.97487385594604E-11,
5.43554633184094));
#33250=CARTESIAN_POINT('Ctrl Pts',(-3.36161420616976,-4.97487385594604E-11,
5.48509146894737));
#33251=CARTESIAN_POINT('Ctrl Pts',(-3.42258429650568,-4.96782254655346E-11,
5.49971498392992));
#33252=CARTESIAN_POINT('Ctrl Pts',(-3.55707996410541,-4.96782254655346E-11,
5.50070596657406));
#33253=CARTESIAN_POINT('Ctrl Pts',(-3.6224276251006,-4.96189542105038E-11,
5.48850912970297));
#33254=CARTESIAN_POINT('Ctrl Pts',(-3.73518454380962,-4.96189542105038E-11,
5.44464447877917));
#33255=CARTESIAN_POINT('Ctrl Pts',(-3.79238690270398,-4.95907660412871E-11,
5.41288812863561));
#33256=CARTESIAN_POINT('Ctrl Pts',(-3.89031170630778,-4.95907660412871E-11,
5.31852450471732));
#33257=CARTESIAN_POINT('Ctrl Pts',(-3.92692344562731,-4.9585361853769E-11,
5.26626913463268));
#33258=CARTESIAN_POINT('Ctrl Pts',(-3.98096251721357,-4.9585361853769E-11,
5.14916603469699));
#33259=CARTESIAN_POINT('Ctrl Pts',(-3.99724813668202,-4.95755933351878E-11,
5.08357638654045));
#33260=CARTESIAN_POINT('Ctrl Pts',(-3.99989324026065,-4.95755933351878E-11,
5.01155755660981));
#33261=CARTESIAN_POINT('Ctrl Pts',(-4.,-1.30506089359971E-54,5.00577896782872));
#33262=CARTESIAN_POINT('Ctrl Pts',(-4.,-1.30506089359971E-54,5.));
#33263=CARTESIAN_POINT('',(-14.1036297108185,1.72719649817133E-14,22.5));
#33264=CARTESIAN_POINT('Ctrl Pts',(-4.,0.,5.));
#33265=CARTESIAN_POINT('Ctrl Pts',(-4.05262307141051,-0.654498469497874,
5.09114583333333));
#33266=CARTESIAN_POINT('Ctrl Pts',(-3.83031081101585,-2.0164870728516,5.2734375));
#33267=CARTESIAN_POINT('Ctrl Pts',(-2.51852354898032,-3.7208214715467,5.546875));
#33268=CARTESIAN_POINT('Ctrl Pts',(-0.483385262891241,-4.63216118014149,
5.82031249999999));
#33269=CARTESIAN_POINT('Ctrl Pts',(1.8202315402997,-4.46495458019068,6.09375000000001));
#33270=CARTESIAN_POINT('Ctrl Pts',(3.83708110788313,-3.18392684763,6.36718749999999));
#33271=CARTESIAN_POINT('Ctrl Pts',(5.04610371647275,-1.03126017046504,6.640625));
#33272=CARTESIAN_POINT('Ctrl Pts',(5.09366526266359,1.51694087528755,6.9140625));
#33273=CARTESIAN_POINT('Ctrl Pts',(3.89334793428042,3.85517018194508,7.1875));
#33274=CARTESIAN_POINT('Ctrl Pts',(1.66401832874098,5.39254335225655,7.4609375));
#33275=CARTESIAN_POINT('Ctrl Pts',(-1.10655649717025,5.70140348716183,7.73437499999999));
#33276=CARTESIAN_POINT('Ctrl Pts',(-3.76778215269101,4.63360702978987,8.0078125));
#33277=CARTESIAN_POINT('Ctrl Pts',(-5.65899445677288,2.37325046891981,8.28125));
#33278=CARTESIAN_POINT('Ctrl Pts',(-6.27308950292314,-0.59072056165688,
8.5546875));
#33279=CARTESIAN_POINT('Ctrl Pts',(-5.39055984190282,-3.56939135267172,
8.828125));
#33280=CARTESIAN_POINT('Ctrl Pts',(-3.14892433147632,-5.83395881494245,
9.10156249999999));
#33281=CARTESIAN_POINT('Ctrl Pts',(-0.0269941651234124,-6.79383570767807,
9.375));
#33282=CARTESIAN_POINT('Ctrl Pts',(3.25625963494257,-6.14929751664737,9.64843749999999));
#33283=CARTESIAN_POINT('Ctrl Pts',(5.90717602022873,-3.9795144383767,9.921875));
#33284=CARTESIAN_POINT('Ctrl Pts',(7.24915357717334,-0.741104090144106,
10.1953125));
#33285=CARTESIAN_POINT('Ctrl Pts',(6.89437699385751,2.82652617704715,10.46875));
#33286=CARTESIAN_POINT('Ctrl Pts',(4.85214544364602,5.8698051725334,10.7421875));
#33287=CARTESIAN_POINT('Ctrl Pts',(1.54426647303593,7.62518428271038,11.015625));
#33288=CARTESIAN_POINT('Ctrl Pts',(-2.28027404042269,7.61004816114384,11.2890625));
#33289=CARTESIAN_POINT('Ctrl Pts',(-5.71458753487403,5.75276305414747,11.5625));
#33290=CARTESIAN_POINT('Ctrl Pts',(-7.90892381685067,2.42735464211985,11.8359375));
#33291=CARTESIAN_POINT('Ctrl Pts',(-8.280487904502,-1.61956843656331,12.109375));
#33292=CARTESIAN_POINT('Ctrl Pts',(-6.66632390115336,-5.43598980597183,
12.3828125));
#33293=CARTESIAN_POINT('Ctrl Pts',(-3.37955924042675,-8.08843859127204,
12.65625));
#33294=CARTESIAN_POINT('Ctrl Pts',(0.848467586061227,-8.89003850095873,
12.9296875));
#33295=CARTESIAN_POINT('Ctrl Pts',(5.03032510682704,-7.57700176269046,13.203125));
#33296=CARTESIAN_POINT('Ctrl Pts',(8.15306896806033,-4.38851452128152,13.4765625));
#33297=CARTESIAN_POINT('Ctrl Pts',(9.42344702515047,-0.0269941685586242,
13.75));
#33298=CARTESIAN_POINT('Ctrl Pts',(8.46840766181913,4.49584983333495,14.0234375));
#33299=CARTESIAN_POINT('Ctrl Pts',(5.44044821239548,8.09361792642082,14.296875));
#33300=CARTESIAN_POINT('Ctrl Pts',(0.998851072840637,9.86610260310719,14.5703125));
#33301=CARTESIAN_POINT('Ctrl Pts',(-3.83283486415787,9.32382107321317,14.84375));
#33302=CARTESIAN_POINT('Ctrl Pts',(-7.90252221315964,6.52035320687432,15.1171875));
#33303=CARTESIAN_POINT('Ctrl Pts',(-10.2042683613299,2.05727819272983,15.390625));
#33304=CARTESIAN_POINT('Ctrl Pts',(-10.1264293031967,-3.04360991455306,
15.6640625));
#33305=CARTESIAN_POINT('Ctrl Pts',(-7.61217905231046,-7.57400353305939,
15.9375));
#33306=CARTESIAN_POINT('Ctrl Pts',(-3.19069051639217,-10.4253049589896,
16.2109375));
#33307=CARTESIAN_POINT('Ctrl Pts',(2.13258015658974,-10.859571982884,16.484375));
#33308=CARTESIAN_POINT('Ctrl Pts',(7.10419756851087,-8.69904094228735,16.7578125));
#33309=CARTESIAN_POINT('Ctrl Pts',(10.5178826720182,-4.38586792650576,17.03125));
#33310=CARTESIAN_POINT('Ctrl Pts',(11.506987524106,1.10621456668648,17.3046875));
#33311=CARTESIAN_POINT('Ctrl Pts',(9.76344367445795,6.49125888499182,17.578125));
#33312=CARTESIAN_POINT('Ctrl Pts',(5.62810470852332,10.4721791049393,17.8515625));
#33313=CARTESIAN_POINT('Ctrl Pts',(0.0269941874218459,12.0530583592068,
18.125));
#33314=CARTESIAN_POINT('Ctrl Pts',(-5.73544006773032,10.7875177817739,18.3984375));
#33315=CARTESIAN_POINT('Ctrl Pts',(-10.2800597580419,6.90138203286673,18.671875));
#33316=CARTESIAN_POINT('Ctrl Pts',(-12.4830517794477,1.25659796463401,18.9453125));
#33317=CARTESIAN_POINT('Ctrl Pts',(-11.7532648511587,-4.83914337048452,
19.21875));
#33318=CARTESIAN_POINT('Ctrl Pts',(-8.18856157315,-9.93523961480004,19.4921875));
#33319=CARTESIAN_POINT('Ctrl Pts',(-2.57028870635813,-12.7833517182835,
19.765625));
#33320=CARTESIAN_POINT('Ctrl Pts',(3.80694337685198,-12.6428118882295,20.0390625));
#33321=CARTESIAN_POINT('Ctrl Pts',(9.43342435418766,-9.47159216503061,20.3125));
#33322=CARTESIAN_POINT('Ctrl Pts',(12.9416764567355,-3.95403216061098,20.5859375));
#33323=CARTESIAN_POINT('Ctrl Pts',(13.4386753471291,2.64560341469982,20.859375));
#33324=CARTESIAN_POINT('Ctrl Pts',(10.731719416327,8.77238225818101,21.1328125));
#33325=CARTESIAN_POINT('Ctrl Pts',(5.39225375379758,12.9473728958347,21.40625));
#33326=CARTESIAN_POINT('Ctrl Pts',(-1.36411605698682,14.1238442145743,21.6796875));
#33327=CARTESIAN_POINT('Ctrl Pts',(-7.95188025078462,11.9500710288293,21.953125));
#33328=CARTESIAN_POINT('Ctrl Pts',(-12.791953880403,6.86731330268108,22.2265625));
#33329=CARTESIAN_POINT('Ctrl Pts',(-14.0510066394079,2.30770101502388,22.4088541666667));
#33330=CARTESIAN_POINT('Ctrl Pts',(-14.1036297108185,1.72719649817133E-14,
22.5));
#33331=CARTESIAN_POINT('Ctrl Pts',(-14.1036297108185,1.66533453693773E-14,
22.5));
#33332=CARTESIAN_POINT('Ctrl Pts',(-14.1036297108185,1.66533453693773E-14,
22.4931309043374));
#33333=CARTESIAN_POINT('Ctrl Pts',(-14.1034788387995,1.66531662825221E-14,
22.4862623794188));
#33334=CARTESIAN_POINT('Ctrl Pts',(-14.1002811166966,1.66492502023841E-14,
22.4129268800063));
#33335=CARTESIAN_POINT('Ctrl Pts',(-14.0834705379208,1.66292904606448E-14,
22.347144032276));
#33336=CARTESIAN_POINT('Ctrl Pts',(-14.0286766940609,1.65621873551489E-14,
22.2305281202362));
#33337=CARTESIAN_POINT('Ctrl Pts',(-13.9920007099842,1.65187598746323E-14,
22.1787736257353));
#33338=CARTESIAN_POINT('Ctrl Pts',(-13.8942385509797,1.63990357595296E-14,
22.0855877281671));
#33339=CARTESIAN_POINT('Ctrl Pts',(-13.8372385327547,1.65612167903603E-14,
22.0543170879823));
#33340=CARTESIAN_POINT('Ctrl Pts',(-13.7242585716272,1.64228562425978E-14,
22.0110695103706));
#33341=CARTESIAN_POINT('Ctrl Pts',(-13.6586187167909,1.63472900537156E-14,
21.9992928151312));
#33342=CARTESIAN_POINT('Ctrl Pts',(-13.528771486911,1.61882730592651E-14,
22.0011480438118));
#33343=CARTESIAN_POINT('Ctrl Pts',(-13.4663656730128,1.66245598057237E-14,
22.0144829337249));
#33344=CARTESIAN_POINT('Ctrl Pts',(-13.3457270961587,1.64768201587257E-14,
22.0669821183785));
#33345=CARTESIAN_POINT('Ctrl Pts',(-13.2896878319382,1.64156409587601E-14,
22.1059488392955));
#33346=CARTESIAN_POINT('Ctrl Pts',(-13.2067932453118,1.63141243685814E-14,
22.1911381458157));
#33347=CARTESIAN_POINT('Ctrl Pts',(-13.168924538057,1.55630875029458E-14,
22.2410844954725));
#33348=CARTESIAN_POINT('Ctrl Pts',(-13.1164702794208,1.54988495630052E-14,
22.3673474980845));
#33349=CARTESIAN_POINT('Ctrl Pts',(-13.1039637101555,1.54821629830264E-14,
22.4337645256774));
#33350=CARTESIAN_POINT('Ctrl Pts',(-13.1042036570148,1.54824568331797E-14,
22.5666921253015));
#33351=CARTESIAN_POINT('Ctrl Pts',(-13.1171254904007,1.54984491412652E-14,
22.6335431762745));
#33352=CARTESIAN_POINT('Ctrl Pts',(-13.1707730203801,1.55641484171366E-14,
22.7613131645324));
#33353=CARTESIAN_POINT('Ctrl Pts',(-13.2095003145773,1.6725202005197E-14,
22.8116763951221));
#33354=CARTESIAN_POINT('Ctrl Pts',(-13.2928111432349,1.68272283448469E-14,
22.896640266457));
#33355=CARTESIAN_POINT('Ctrl Pts',(-13.3492037310432,1.69009548416532E-14,
22.9355463321452));
#33356=CARTESIAN_POINT('Ctrl Pts',(-13.4652439179706,1.70430630851463E-14,
22.9850914692808));
#33357=CARTESIAN_POINT('Ctrl Pts',(-13.5262140083287,1.55816880134289E-14,
22.999714984015));
#33358=CARTESIAN_POINT('Ctrl Pts',(-13.6607096755624,1.57463977018059E-14,
23.0007059664907));
#33359=CARTESIAN_POINT('Ctrl Pts',(-13.7260573365682,1.58201349665679E-14,
22.9885091295348));
#33360=CARTESIAN_POINT('Ctrl Pts',(-13.8388142552453,1.59582223661075E-14,
22.9446444784495));
#33361=CARTESIAN_POINT('Ctrl Pts',(-13.8960166140677,1.66282530092132E-14,
22.9128881282363));
#33362=CARTESIAN_POINT('Ctrl Pts',(-13.9939414175529,1.67481763063585E-14,
22.8185245041776));
#33363=CARTESIAN_POINT('Ctrl Pts',(-14.0305531568207,1.67881918203982E-14,
22.7662691340177));
#33364=CARTESIAN_POINT('Ctrl Pts',(-14.0845922282433,1.68543705962449E-14,
22.649166033998));
#33365=CARTESIAN_POINT('Ctrl Pts',(-14.1008778476158,1.68694037472559E-14,
22.5835763858428));
#33366=CARTESIAN_POINT('Ctrl Pts',(-14.1035229510752,1.68726430647407E-14,
22.5115575563802));
#33367=CARTESIAN_POINT('Ctrl Pts',(-14.1036297108185,1.68723542082194E-14,
22.5057789677136));
#33368=CARTESIAN_POINT('Ctrl Pts',(-14.1036297108185,1.68723542082194E-14,
22.5));
#33369=CARTESIAN_POINT('Origin',(-13.6036297108184,1.66596415821396E-14,
22.5));
#33370=CARTESIAN_POINT('Origin',(-3.5,0.,5.));
#33371=CARTESIAN_POINT('',(0.,0.,0.));
#33372=CARTESIAN_POINT('Origin',(0.00181468412045555,4.04249959269282,3.2));
#33373=CARTESIAN_POINT('',(5.58144376948235E-15,4.04145188432738,0.285124696255161));
#33374=CARTESIAN_POINT('',(5.95743279803446E-15,4.04145188432738,2.91487530374485));
#33375=CARTESIAN_POINT('',(5.55111512312578E-15,4.04145188432738,3.2));
#33376=CARTESIAN_POINT('',(-3.5,2.02072594216369,0.285124696255161));
#33377=CARTESIAN_POINT('Ctrl Pts',(-3.5,2.02072594216369,0.285124696255161));
#33378=CARTESIAN_POINT('Ctrl Pts',(-1.75,3.03108891324554,-0.186015294676542));
#33379=CARTESIAN_POINT('Ctrl Pts',(5.58144376948235E-15,4.04145188432738,
0.285124696255161));
#33380=CARTESIAN_POINT('',(-3.5,2.02072594216369,2.91487530374484));
#33381=CARTESIAN_POINT('',(-3.5,2.02072594216369,3.2));
#33382=CARTESIAN_POINT('Ctrl Pts',(5.95743279803446E-15,4.04145188432738,
2.91487530374485));
#33383=CARTESIAN_POINT('Ctrl Pts',(-1.75,3.03108891324554,3.38601529467654));
#33384=CARTESIAN_POINT('Ctrl Pts',(-3.5,2.02072594216369,2.91487530374484));
#33385=CARTESIAN_POINT('Origin',(-3.5,2.02282135889456,3.2));
#33386=CARTESIAN_POINT('',(-3.5,-2.02072594216369,0.285124696255161));
#33387=CARTESIAN_POINT('Ctrl Pts',(-3.5,-2.02072594216369,0.285124696255161));
#33388=CARTESIAN_POINT('Ctrl Pts',(-3.5,3.05311331771918E-15,-0.186015294676541));
#33389=CARTESIAN_POINT('Ctrl Pts',(-3.5,2.02072594216369,0.285124696255161));
#33390=CARTESIAN_POINT('',(-3.5,-2.02072594216369,2.91487530374484));
#33391=CARTESIAN_POINT('',(-3.5,-2.02072594216369,3.2));
#33392=CARTESIAN_POINT('Ctrl Pts',(-3.5,2.02072594216369,2.91487530374484));
#33393=CARTESIAN_POINT('Ctrl Pts',(-3.5,3.60822483003176E-15,3.38601529467654));
#33394=CARTESIAN_POINT('Ctrl Pts',(-3.5,-2.02072594216369,2.91487530374484));
#33395=CARTESIAN_POINT('Origin',(0.,0.,0.142806720309968));
#33396=CARTESIAN_POINT('',(3.43,-4.20053852107542E-16,-5.20417042793042E-16));
#33397=CARTESIAN_POINT('Origin',(0.,0.,-2.77555756156289E-16));
#33398=CARTESIAN_POINT('',(3.5,-4.0750745167651E-16,0.032641536070849));
#33399=CARTESIAN_POINT('',(3.73625,-4.5755866033143E-16,0.142806720309968));
#33400=CARTESIAN_POINT('',(3.5,-2.02072594216369,0.285124696255161));
#33401=CARTESIAN_POINT('Ctrl Pts',(3.5,-3.86388523651447E-16,0.032641536070849));
#33402=CARTESIAN_POINT('Ctrl Pts',(3.5,-0.937822173508931,0.0326415360708487));
#33403=CARTESIAN_POINT('Ctrl Pts',(3.5,-2.02072594216369,0.285124696255161));
#33404=CARTESIAN_POINT('',(-3.69459687690438E-15,-4.04145188432738,0.285124696255161));
#33405=CARTESIAN_POINT('Ctrl Pts',(3.5,-2.02072594216369,0.285124696255161));
#33406=CARTESIAN_POINT('Ctrl Pts',(1.75,-3.03108891324554,-0.186015294676541));
#33407=CARTESIAN_POINT('Ctrl Pts',(-3.69459687690438E-15,-4.04145188432738,
0.285124696255161));
#33408=CARTESIAN_POINT('Ctrl Pts',(-3.59512132757884E-15,-4.04145188432738,
0.285124696255161));
#33409=CARTESIAN_POINT('Ctrl Pts',(-1.75000000000001,-3.03108891324553,
-0.186015294676541));
#33410=CARTESIAN_POINT('Ctrl Pts',(-3.5,-2.02072594216369,0.285124696255161));
#33411=CARTESIAN_POINT('',(3.5,2.02072594216369,0.285124696255161));
#33412=CARTESIAN_POINT('Ctrl Pts',(5.57202476310889E-15,4.04145188432738,
0.285124696255161));
#33413=CARTESIAN_POINT('Ctrl Pts',(1.75,3.03108891324553,-0.186015294676541));
#33414=CARTESIAN_POINT('Ctrl Pts',(3.5,2.02072594216369,0.285124696255161));
#33415=CARTESIAN_POINT('Ctrl Pts',(3.5,2.02072594216369,0.285124696255161));
#33416=CARTESIAN_POINT('Ctrl Pts',(3.5,0.937822173508927,0.0326415360708494));
#33417=CARTESIAN_POINT('Ctrl Pts',(3.5,-3.86388523651447E-16,0.032641536070849));
#33418=CARTESIAN_POINT('Origin',(3.50181468412045,2.01967823379825,3.2));
#33419=CARTESIAN_POINT('',(3.5,2.02072594216369,2.91487530374484));
#33420=CARTESIAN_POINT('Ctrl Pts',(3.5,2.02072594216369,2.91487530374484));
#33421=CARTESIAN_POINT('Ctrl Pts',(1.75,3.03108891324553,3.38601529467654));
#33422=CARTESIAN_POINT('Ctrl Pts',(6.00171568051692E-15,4.04145188432738,
2.91487530374485));
#33423=CARTESIAN_POINT('',(3.5,2.02072594216369,3.2));
#33424=CARTESIAN_POINT('Origin',(3.5,-2.02282135889456,3.2));
#33425=CARTESIAN_POINT('',(3.5,-3.75308408038889E-16,3.16735846392915));
#33426=CARTESIAN_POINT('Ctrl Pts',(3.5,-3.21990436376205E-16,3.16735846392915));
#33427=CARTESIAN_POINT('Ctrl Pts',(3.5,0.937822173508926,3.16735846392915));
#33428=CARTESIAN_POINT('Ctrl Pts',(3.5,2.02072594216369,2.91487530374484));
#33429=CARTESIAN_POINT('',(3.5,-2.02072594216369,2.91487530374485));
#33430=CARTESIAN_POINT('Ctrl Pts',(3.5,-2.02072594216369,2.91487530374485));
#33431=CARTESIAN_POINT('Ctrl Pts',(3.5,-0.937822173508929,3.16735846392915));
#33432=CARTESIAN_POINT('Ctrl Pts',(3.5,-3.21990436376205E-16,3.16735846392915));
#33433=CARTESIAN_POINT('',(3.5,-2.02072594216369,3.2));
#33434=CARTESIAN_POINT('Origin',(-0.00181468412045332,-4.04249959269282,
3.2));
#33435=CARTESIAN_POINT('',(-3.93275951036187E-15,-4.04145188432738,2.91487530374484));
#33436=CARTESIAN_POINT('Ctrl Pts',(-3.93275951036187E-15,-4.04145188432738,
2.91487530374484));
#33437=CARTESIAN_POINT('Ctrl Pts',(1.75,-3.03108891324553,3.38601529467654));
#33438=CARTESIAN_POINT('Ctrl Pts',(3.5,-2.02072594216369,2.91487530374485));
#33439=CARTESIAN_POINT('',(-3.33066907387547E-15,-4.04145188432738,3.2));
#33440=CARTESIAN_POINT('Origin',(-3.50181468412045,-2.01967823379825,3.2));
#33441=CARTESIAN_POINT('Ctrl Pts',(-3.5,-2.02072594216369,2.91487530374484));
#33442=CARTESIAN_POINT('Ctrl Pts',(-1.75,-3.03108891324553,3.38601529467654));
#33443=CARTESIAN_POINT('Ctrl Pts',(-4.00462178560693E-15,-4.04145188432738,
2.91487530374484));
#33444=CARTESIAN_POINT('Origin',(-3.43,0.,3.2));
#33445=CARTESIAN_POINT('',(3.43,-4.20053852107542E-16,3.2));
#33446=CARTESIAN_POINT('Origin',(0.,0.,3.2));
#33447=CARTESIAN_POINT('',(1.666,2.04026156737949E-16,3.2));
#33448=CARTESIAN_POINT('Origin',(0.,0.,3.2));
#33449=CARTESIAN_POINT('Origin',(0.,0.,3.05719327969003));
#33450=CARTESIAN_POINT('',(3.73625,-4.5755866033143E-16,3.05719327969003));
#33451=CARTESIAN_POINT('Origin',(-2.,0.,-2.19122965386544E-16));
#33452=CARTESIAN_POINT('',(1.666,-2.04026156737949E-16,-2.77555756156289E-16));
#33453=CARTESIAN_POINT('Origin',(0.,0.,-2.77555756156289E-16));
#33454=CARTESIAN_POINT('Origin',(0.,0.,1.6));
#33455=CARTESIAN_POINT('',(1.666,-2.04026156737949E-16,1.6));
#33456=CARTESIAN_POINT('',(0.,0.,0.));
#33457=CARTESIAN_POINT('',(1.78656643754897E-14,4.82373817799193E-20,-0.00116585095294108));
#33458=CARTESIAN_POINT('',(0.,0.,0.));
#33459=CARTESIAN_POINT('',(0.,0.,0.));
#33460=CARTESIAN_POINT('',(0.,0.,26.4971806130173));
#33461=UNCERTAINTY_MEASURE_WITH_UNIT(LENGTH_MEASURE(0.01),#33475,
'DISTANCE_ACCURACY_VALUE',
'Maximum model space distance between geometric entities at asserted c
onnectivities');
#33462=UNCERTAINTY_MEASURE_WITH_UNIT(LENGTH_MEASURE(0.01),#33475,
'DISTANCE_ACCURACY_VALUE',
'Maximum model space distance between geometric entities at asserted c
onnectivities');
#33463=UNCERTAINTY_MEASURE_WITH_UNIT(LENGTH_MEASURE(0.01),#33475,
'DISTANCE_ACCURACY_VALUE',
'Maximum model space distance between geometric entities at asserted c
onnectivities');
#33464=UNCERTAINTY_MEASURE_WITH_UNIT(LENGTH_MEASURE(0.01),#33475,
'DISTANCE_ACCURACY_VALUE',
'Maximum model space distance between geometric entities at asserted c
onnectivities');
#33465=UNCERTAINTY_MEASURE_WITH_UNIT(LENGTH_MEASURE(0.01),#33475,
'DISTANCE_ACCURACY_VALUE',
'Maximum model space distance between geometric entities at asserted c
onnectivities');
#33466=UNCERTAINTY_MEASURE_WITH_UNIT(LENGTH_MEASURE(0.01),#33475,
'DISTANCE_ACCURACY_VALUE',
'Maximum model space distance between geometric entities at asserted c
onnectivities');
#33467=UNCERTAINTY_MEASURE_WITH_UNIT(LENGTH_MEASURE(0.01),#33475,
'DISTANCE_ACCURACY_VALUE',
'Maximum model space distance between geometric entities at asserted c
onnectivities');
#33468=(
GEOMETRIC_REPRESENTATION_CONTEXT(3)
GLOBAL_UNCERTAINTY_ASSIGNED_CONTEXT((#33461))
GLOBAL_UNIT_ASSIGNED_CONTEXT((#33475,#33477,#33478))
REPRESENTATION_CONTEXT('','3D')
);
#33469=(
GEOMETRIC_REPRESENTATION_CONTEXT(3)
GLOBAL_UNCERTAINTY_ASSIGNED_CONTEXT((#33462))
GLOBAL_UNIT_ASSIGNED_CONTEXT((#33475,#33477,#33478))
REPRESENTATION_CONTEXT('','3D')
);
#33470=(
GEOMETRIC_REPRESENTATION_CONTEXT(3)
GLOBAL_UNCERTAINTY_ASSIGNED_CONTEXT((#33463))
GLOBAL_UNIT_ASSIGNED_CONTEXT((#33475,#33477,#33478))
REPRESENTATION_CONTEXT('','3D')
);
#33471=(
GEOMETRIC_REPRESENTATION_CONTEXT(3)
GLOBAL_UNCERTAINTY_ASSIGNED_CONTEXT((#33464))
GLOBAL_UNIT_ASSIGNED_CONTEXT((#33475,#33477,#33478))
REPRESENTATION_CONTEXT('','3D')
);
#33472=(
GEOMETRIC_REPRESENTATION_CONTEXT(3)
GLOBAL_UNCERTAINTY_ASSIGNED_CONTEXT((#33465))
GLOBAL_UNIT_ASSIGNED_CONTEXT((#33475,#33477,#33478))
REPRESENTATION_CONTEXT('','3D')
);
#33473=(
GEOMETRIC_REPRESENTATION_CONTEXT(3)
GLOBAL_UNCERTAINTY_ASSIGNED_CONTEXT((#33466))
GLOBAL_UNIT_ASSIGNED_CONTEXT((#33475,#33477,#33478))
REPRESENTATION_CONTEXT('','3D')
);
#33474=(
GEOMETRIC_REPRESENTATION_CONTEXT(3)
GLOBAL_UNCERTAINTY_ASSIGNED_CONTEXT((#33467))
GLOBAL_UNIT_ASSIGNED_CONTEXT((#33475,#33477,#33478))
REPRESENTATION_CONTEXT('','3D')
);
#33475=(
LENGTH_UNIT()
NAMED_UNIT(*)
SI_UNIT(.MILLI.,.METRE.)
);
#33476=(
LENGTH_UNIT()
NAMED_UNIT(*)
SI_UNIT($,.METRE.)
);
#33477=(
NAMED_UNIT(*)
PLANE_ANGLE_UNIT()
SI_UNIT($,.RADIAN.)
);
#33478=(
NAMED_UNIT(*)
SI_UNIT($,.STERADIAN.)
SOLID_ANGLE_UNIT()
);
#33479=SHAPE_DEFINITION_REPRESENTATION(#33485,#33496);
#33480=SHAPE_DEFINITION_REPRESENTATION(#33486,#33497);
#33481=SHAPE_DEFINITION_REPRESENTATION(#33487,#33498);
#33482=SHAPE_DEFINITION_REPRESENTATION(#33488,#33499);
#33483=SHAPE_DEFINITION_REPRESENTATION(#33489,#33500);
#33484=SHAPE_DEFINITION_REPRESENTATION(#33490,#33501);
#33485=PRODUCT_DEFINITION_SHAPE('',$,#33503);
#33486=PRODUCT_DEFINITION_SHAPE('',$,#33504);
#33487=PRODUCT_DEFINITION_SHAPE('',$,#33505);
#33488=PRODUCT_DEFINITION_SHAPE('',$,#33506);
#33489=PRODUCT_DEFINITION_SHAPE('',$,#33507);
#33490=PRODUCT_DEFINITION_SHAPE('',$,#33508);
#33491=PRODUCT_DEFINITION_SHAPE($,$,#26);
#33492=PRODUCT_DEFINITION_SHAPE($,$,#27);
#33493=PRODUCT_DEFINITION_SHAPE($,$,#28);
#33494=PRODUCT_DEFINITION_SHAPE($,$,#29);
#33495=PRODUCT_DEFINITION_SHAPE($,$,#30);
#33496=SHAPE_REPRESENTATION('',(#2868,#3144,#3145,#3146,#3147,#3148),#33468);
#33497=SHAPE_REPRESENTATION('',(#2869),#33469);
#33498=SHAPE_REPRESENTATION('',(#3089),#33470);
#33499=SHAPE_REPRESENTATION('',(#3107),#33471);
#33500=SHAPE_REPRESENTATION('',(#3125),#33472);
#33501=SHAPE_REPRESENTATION('',(#3128),#33473);
#33502=PRODUCT_DEFINITION_CONTEXT('part definition',#33522,'design');
#33503=PRODUCT_DEFINITION('BR-106','BR-106',#33509,#33502);
#33504=PRODUCT_DEFINITION('Screw','Screw',#33510,#33502);
#33505=PRODUCT_DEFINITION('Disc_01','Disc_01',#33511,#33502);
#33506=PRODUCT_DEFINITION('Disc_02','Disc_02',#33512,#33502);
#33507=PRODUCT_DEFINITION('Spring','Spring',#33513,#33502);
#33508=PRODUCT_DEFINITION('2026-10-04-16-34-53-963','Nut',#33514,#33502);
#33509=PRODUCT_DEFINITION_FORMATION('',$,#33524);
#33510=PRODUCT_DEFINITION_FORMATION('',$,#33525);
#33511=PRODUCT_DEFINITION_FORMATION('',$,#33526);
#33512=PRODUCT_DEFINITION_FORMATION('',$,#33527);
#33513=PRODUCT_DEFINITION_FORMATION('',$,#33528);
#33514=PRODUCT_DEFINITION_FORMATION('',$,#33529);
#33515=PRODUCT_RELATED_PRODUCT_CATEGORY('BR-106','BR-106',(#33524));
#33516=PRODUCT_RELATED_PRODUCT_CATEGORY('Screw','Screw',(#33525));
#33517=PRODUCT_RELATED_PRODUCT_CATEGORY('Disc_01','Disc_01',(#33526));
#33518=PRODUCT_RELATED_PRODUCT_CATEGORY('Disc_02','Disc_02',(#33527));
#33519=PRODUCT_RELATED_PRODUCT_CATEGORY('Spring','Spring',(#33528));
#33520=PRODUCT_RELATED_PRODUCT_CATEGORY('Nut','Nut',(#33529));
#33521=APPLICATION_PROTOCOL_DEFINITION('international standard',
'automotive_design',2009,#33522);
#33522=APPLICATION_CONTEXT(
'Core Data for Automotive Mechanical Design Process');
#33523=PRODUCT_CONTEXT('part definition',#33522,'mechanical');
#33524=PRODUCT('BR-106','BR-106',$,(#33523));
#33525=PRODUCT('Screw','Screw',$,(#33523));
#33526=PRODUCT('Disc_01','Disc_01',$,(#33523));
#33527=PRODUCT('Disc_02','Disc_02',$,(#33523));
#33528=PRODUCT('Spring','Spring',$,(#33523));
#33529=PRODUCT('2026-10-04-16-34-53-963','Nut',
'Hex Nut Style 1 ASME B18.2.4.1M - M4',(#33523));
#33530=PRESENTATION_STYLE_ASSIGNMENT((#33532));
#33531=PRESENTATION_STYLE_ASSIGNMENT((#33533));
#33532=SURFACE_STYLE_USAGE(.BOTH.,#33534);
#33533=SURFACE_STYLE_USAGE(.BOTH.,#33535);
#33534=SURFACE_SIDE_STYLE('',(#33536));
#33535=SURFACE_SIDE_STYLE('',(#33537));
#33536=SURFACE_STYLE_FILL_AREA(#33538);
#33537=SURFACE_STYLE_FILL_AREA(#33539);
#33538=FILL_AREA_STYLE('Steel - Satin',(#33540));
#33539=FILL_AREA_STYLE('Opaque(203,203,203)',(#33541));
#33540=FILL_AREA_STYLE_COLOUR('Steel - Satin',#33542);
#33541=FILL_AREA_STYLE_COLOUR('Opaque(203,203,203)',#33543);
#33542=COLOUR_RGB('Steel - Satin', 0.72549020, 0.75294118, 0.79215686);
#33543=COLOUR_RGB('Opaque(203,203,203)', 0.09019608, 0.27058824, 0.51372549);
ENDSEC;
END-ISO-10303-21;
